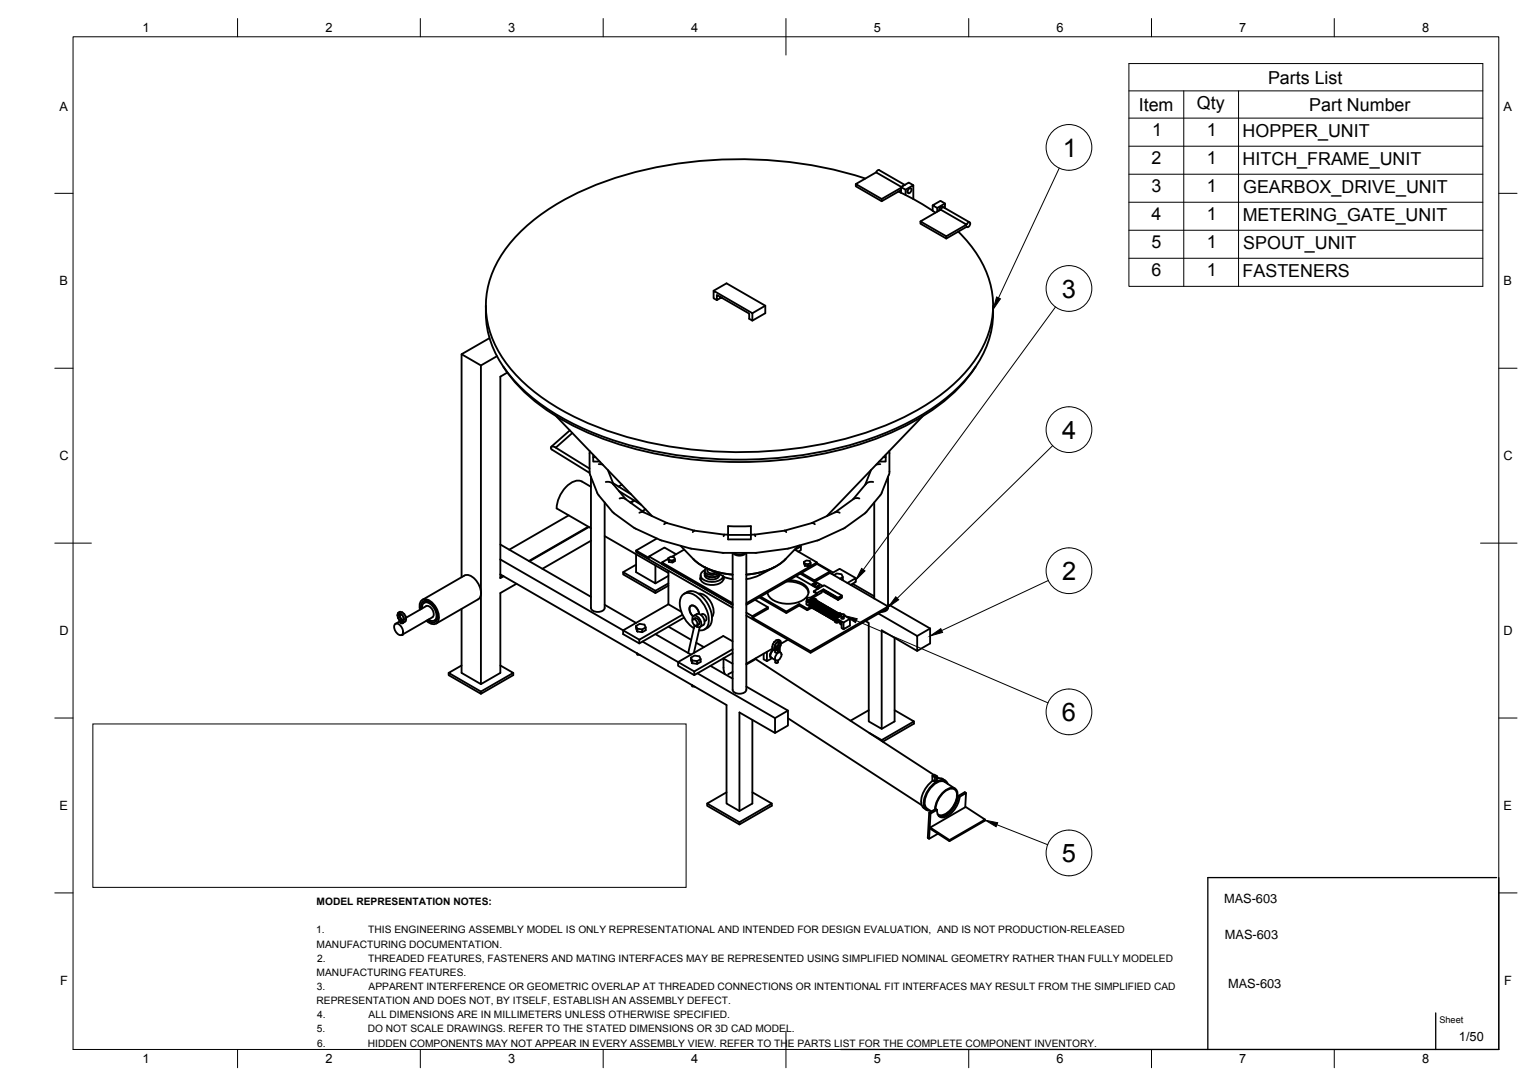
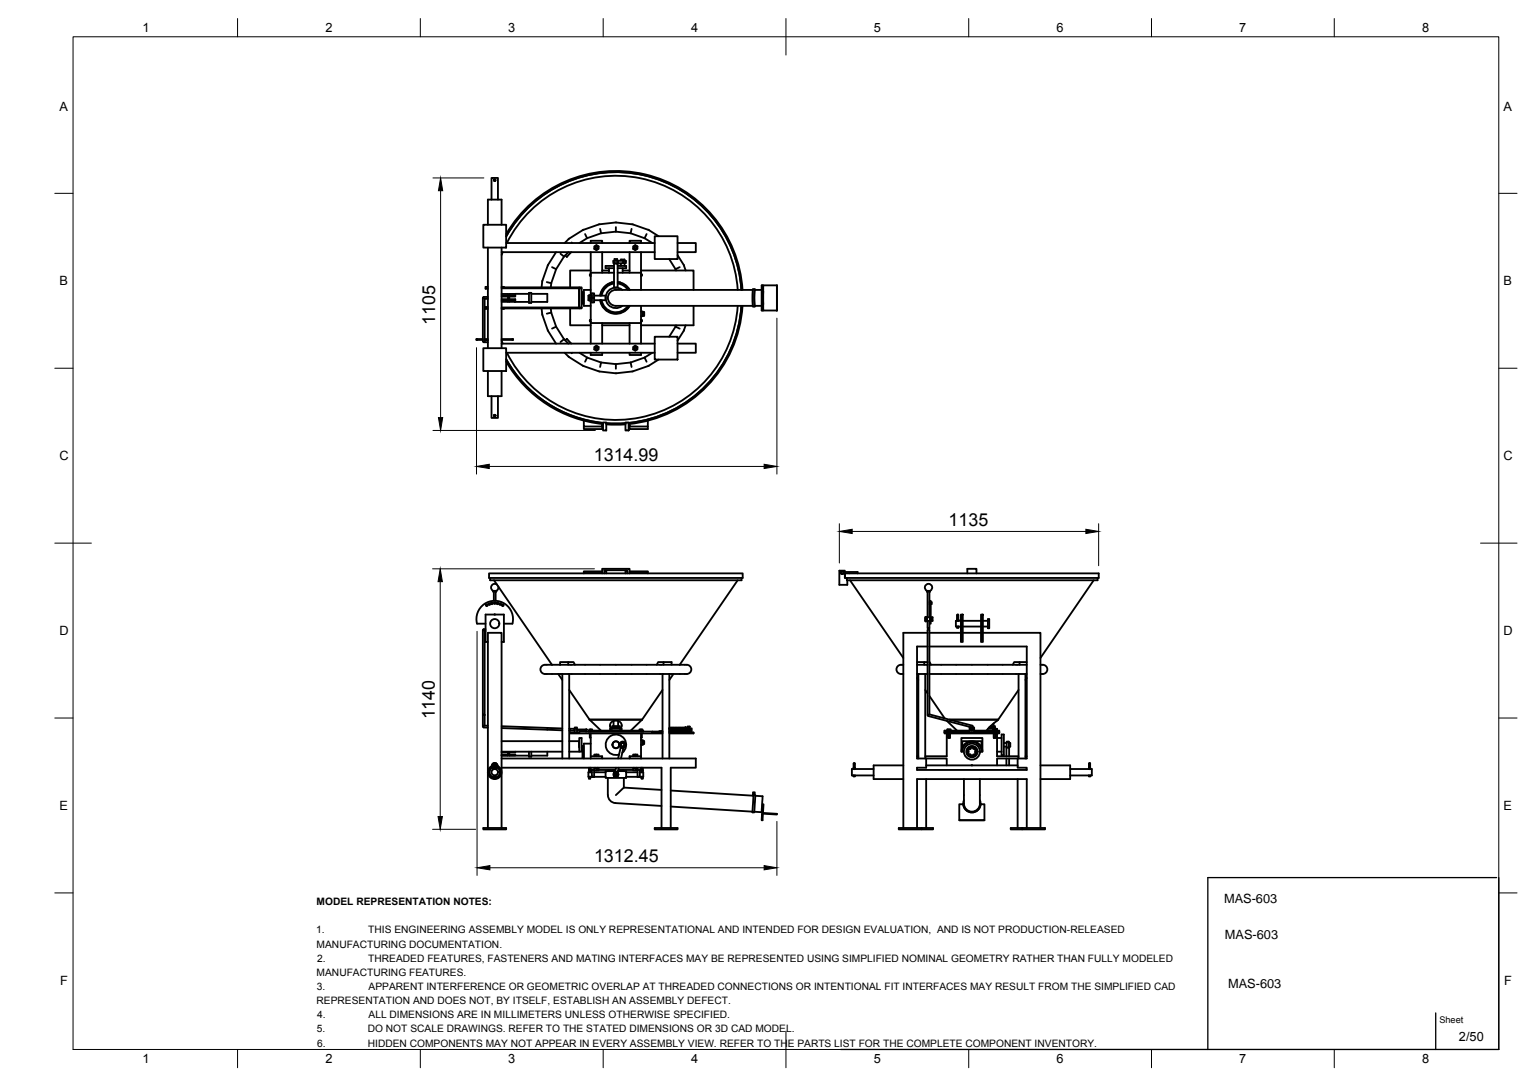
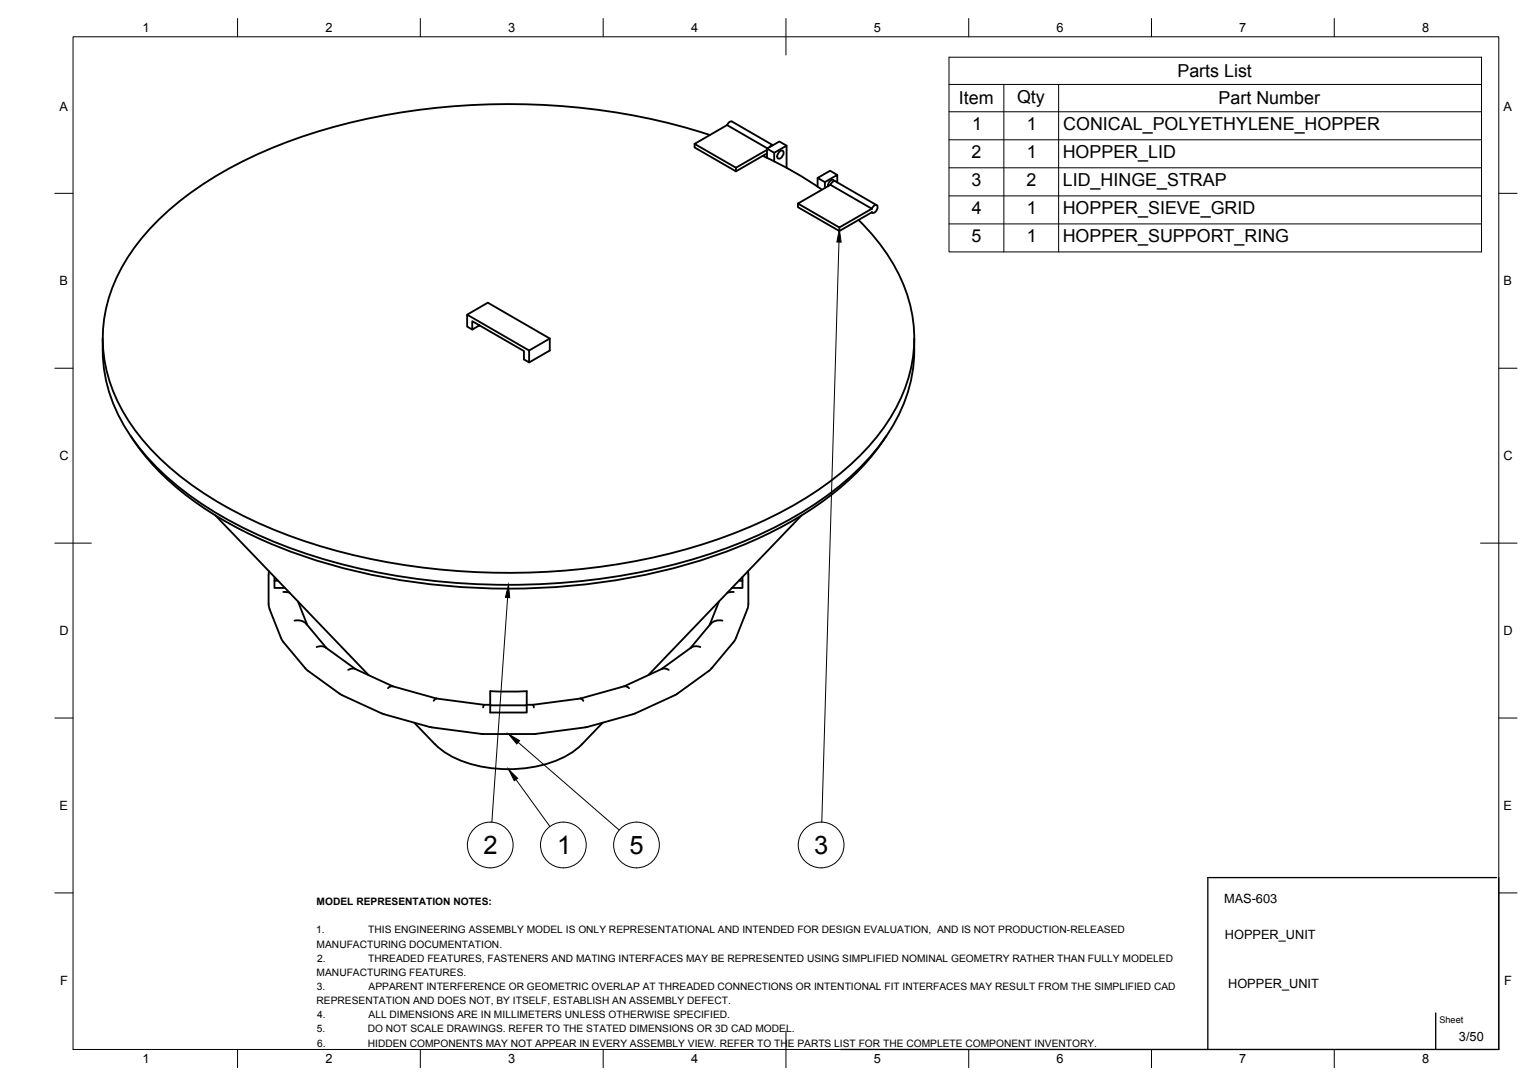
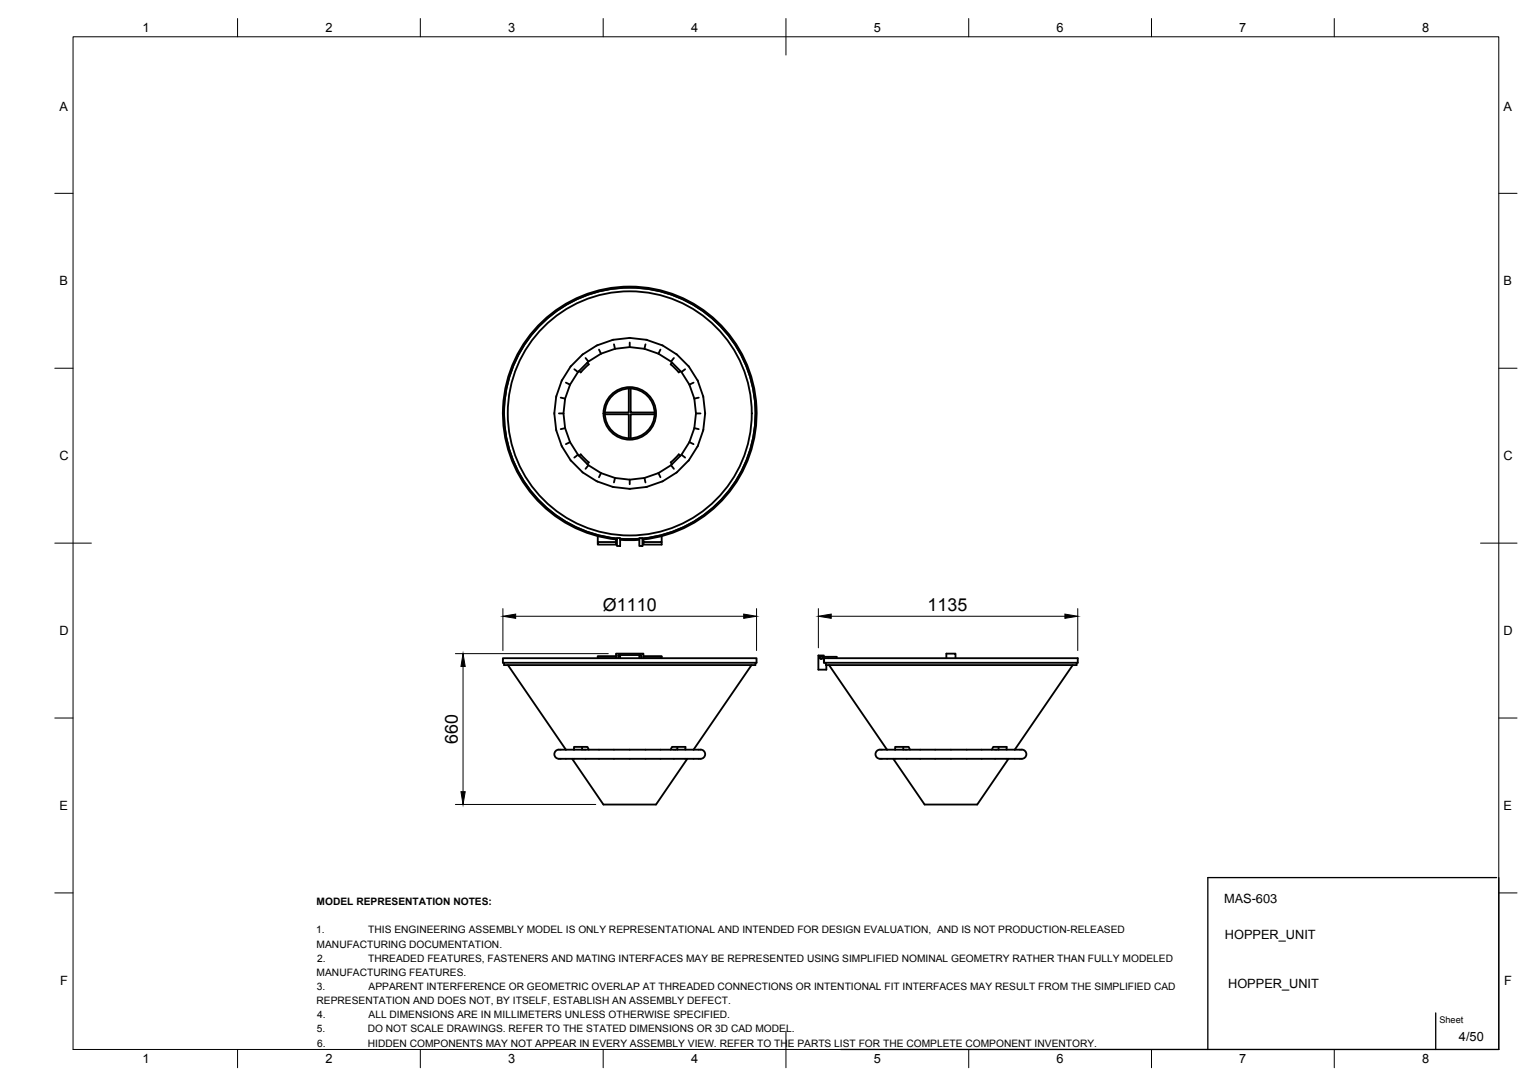
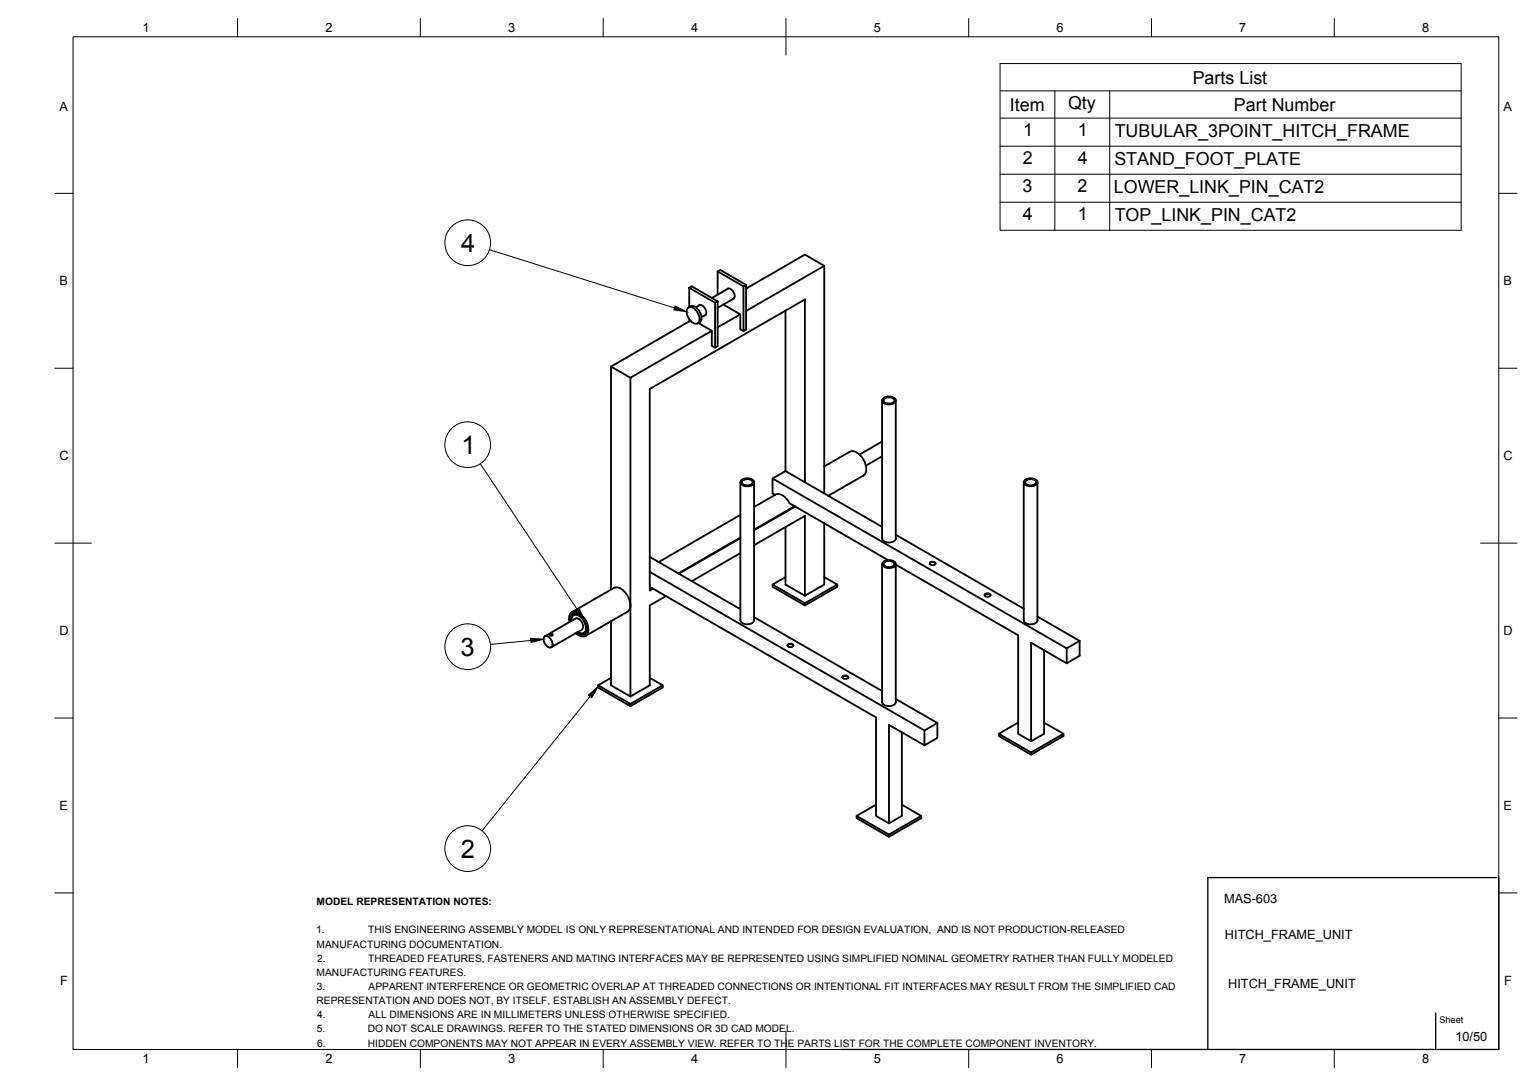
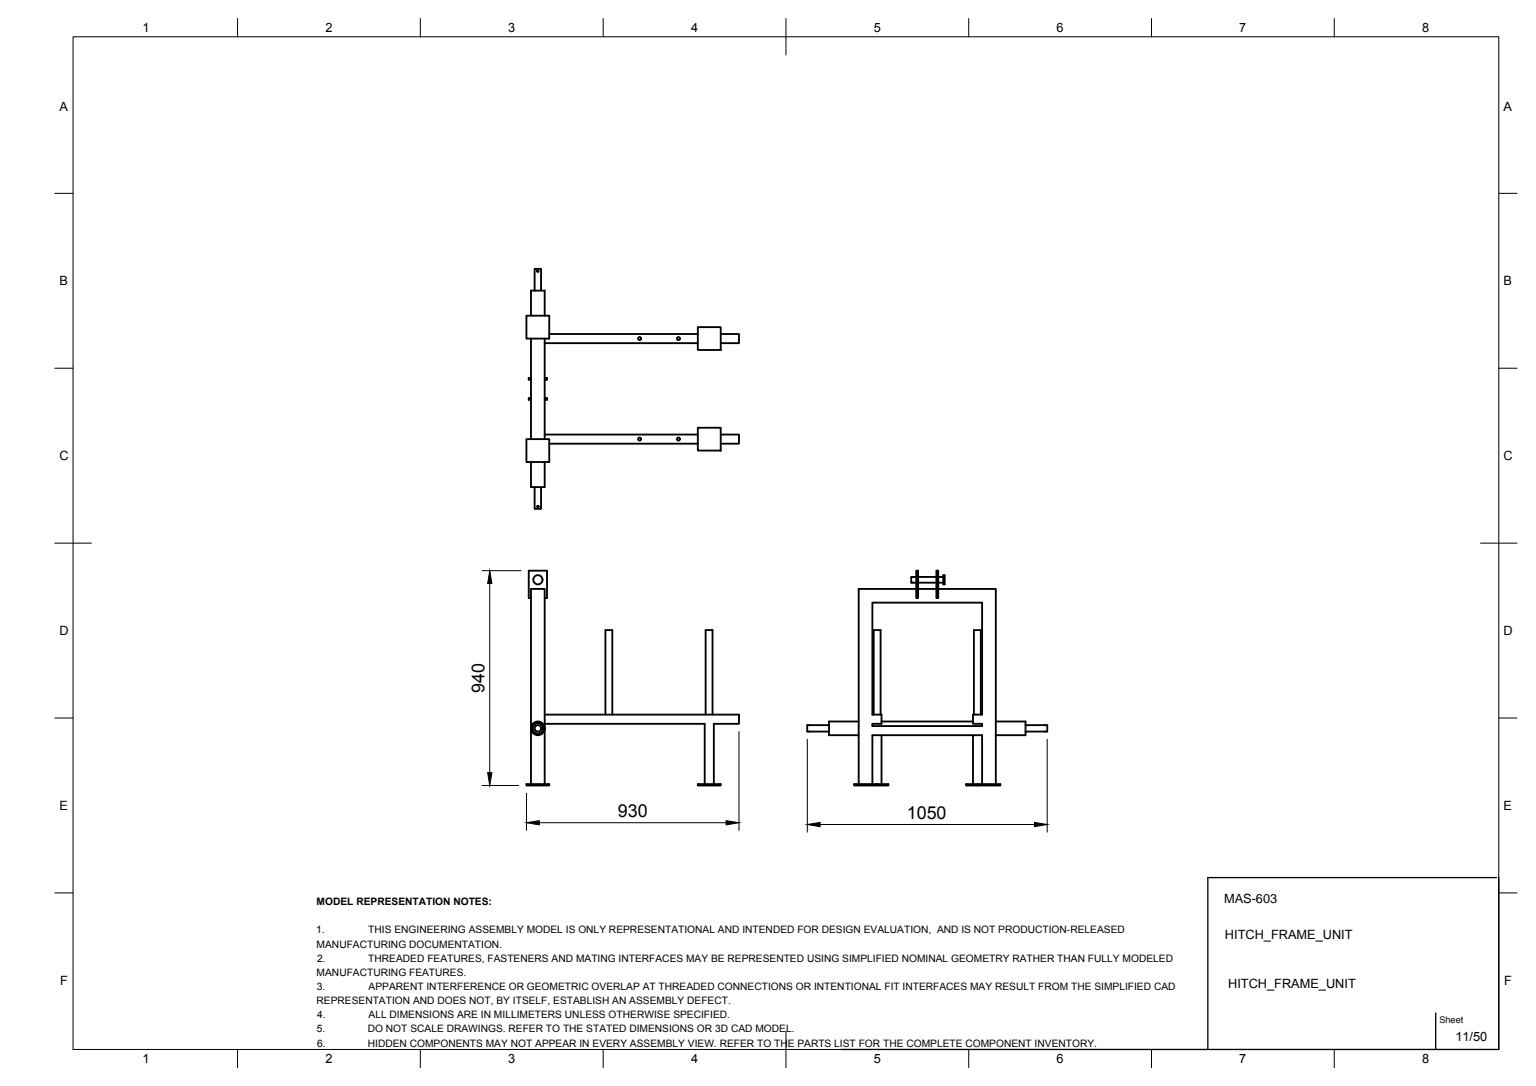
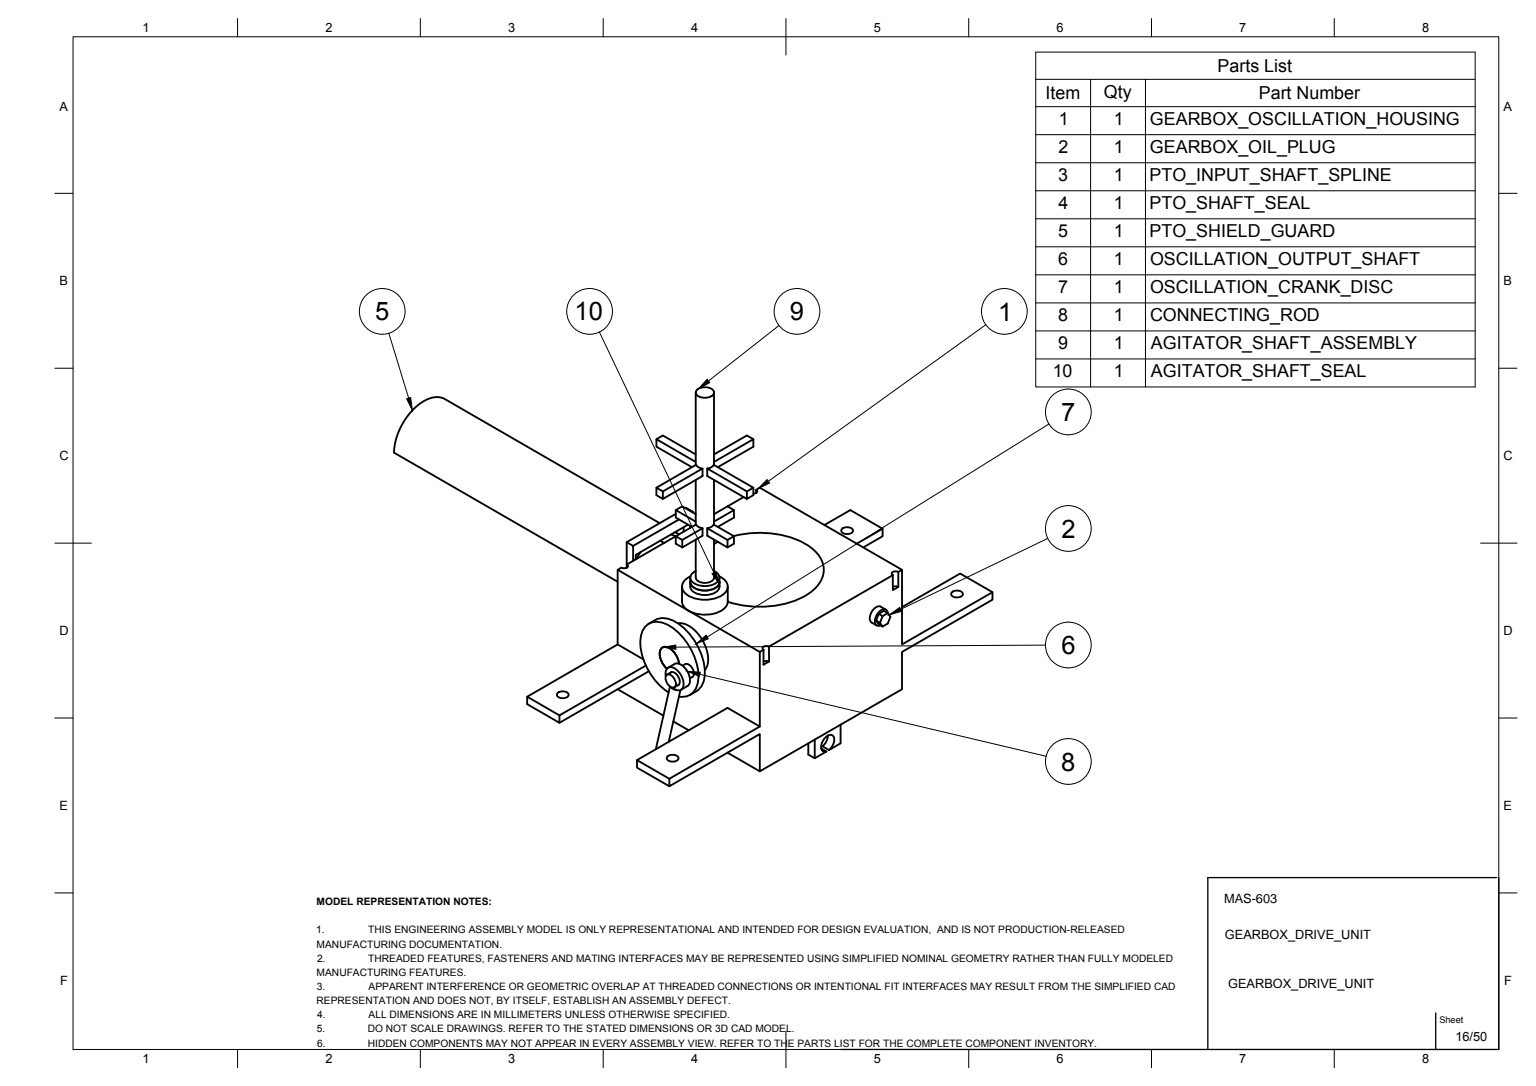
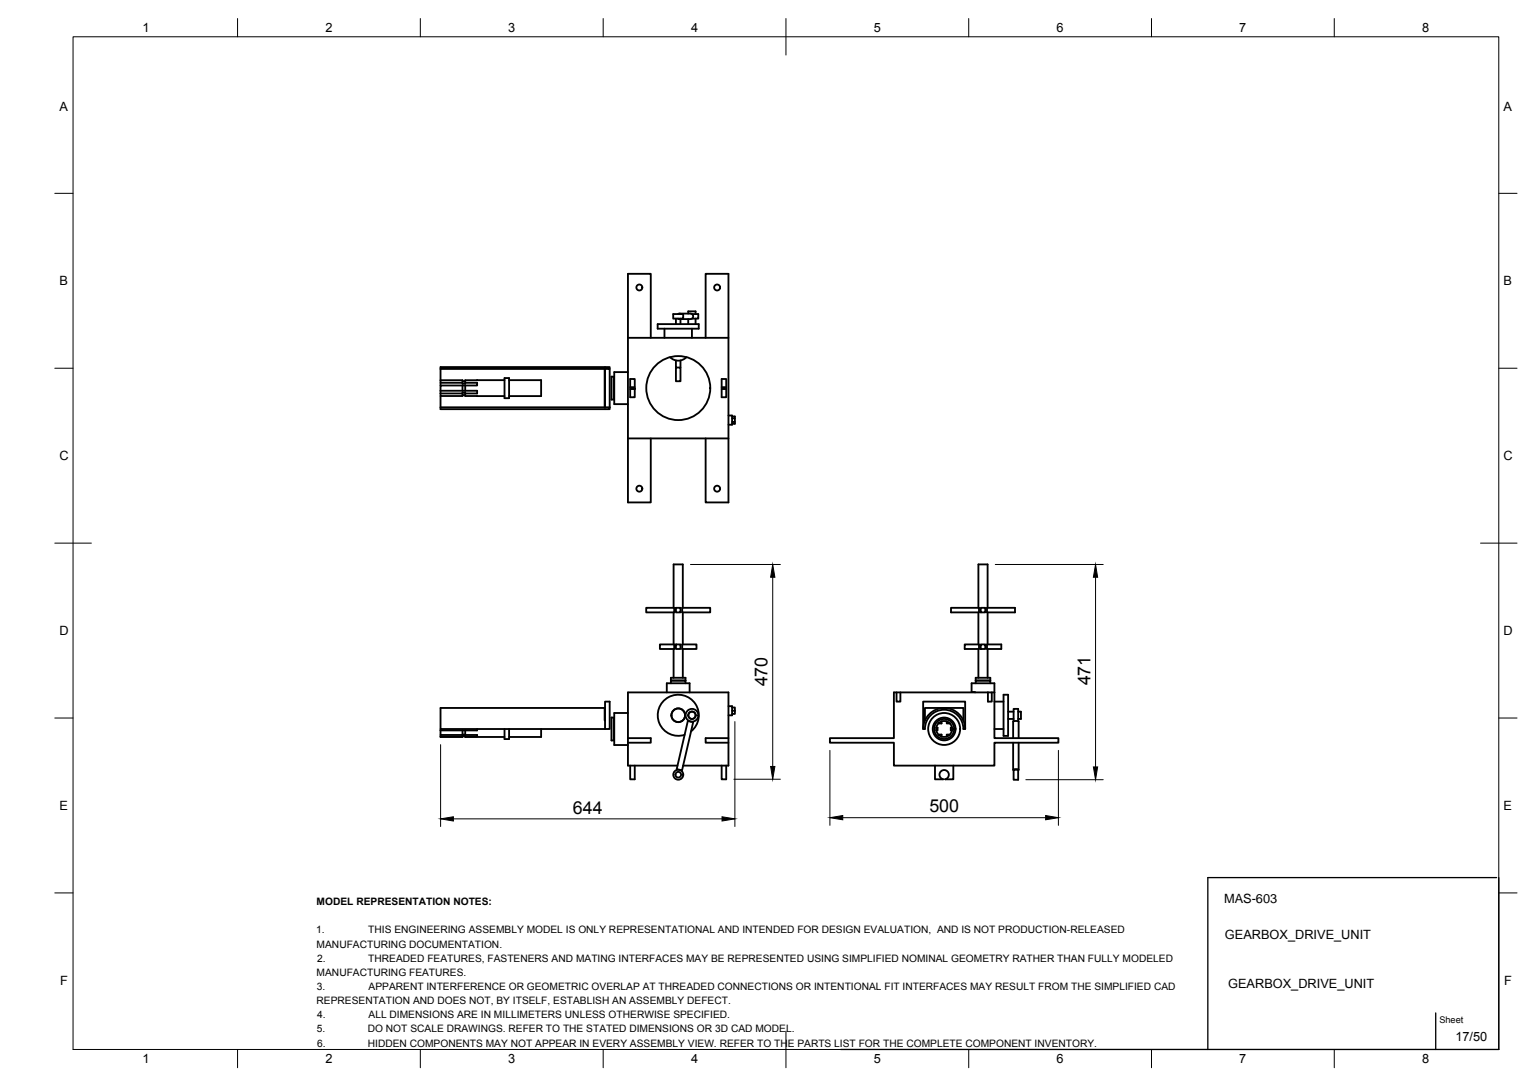
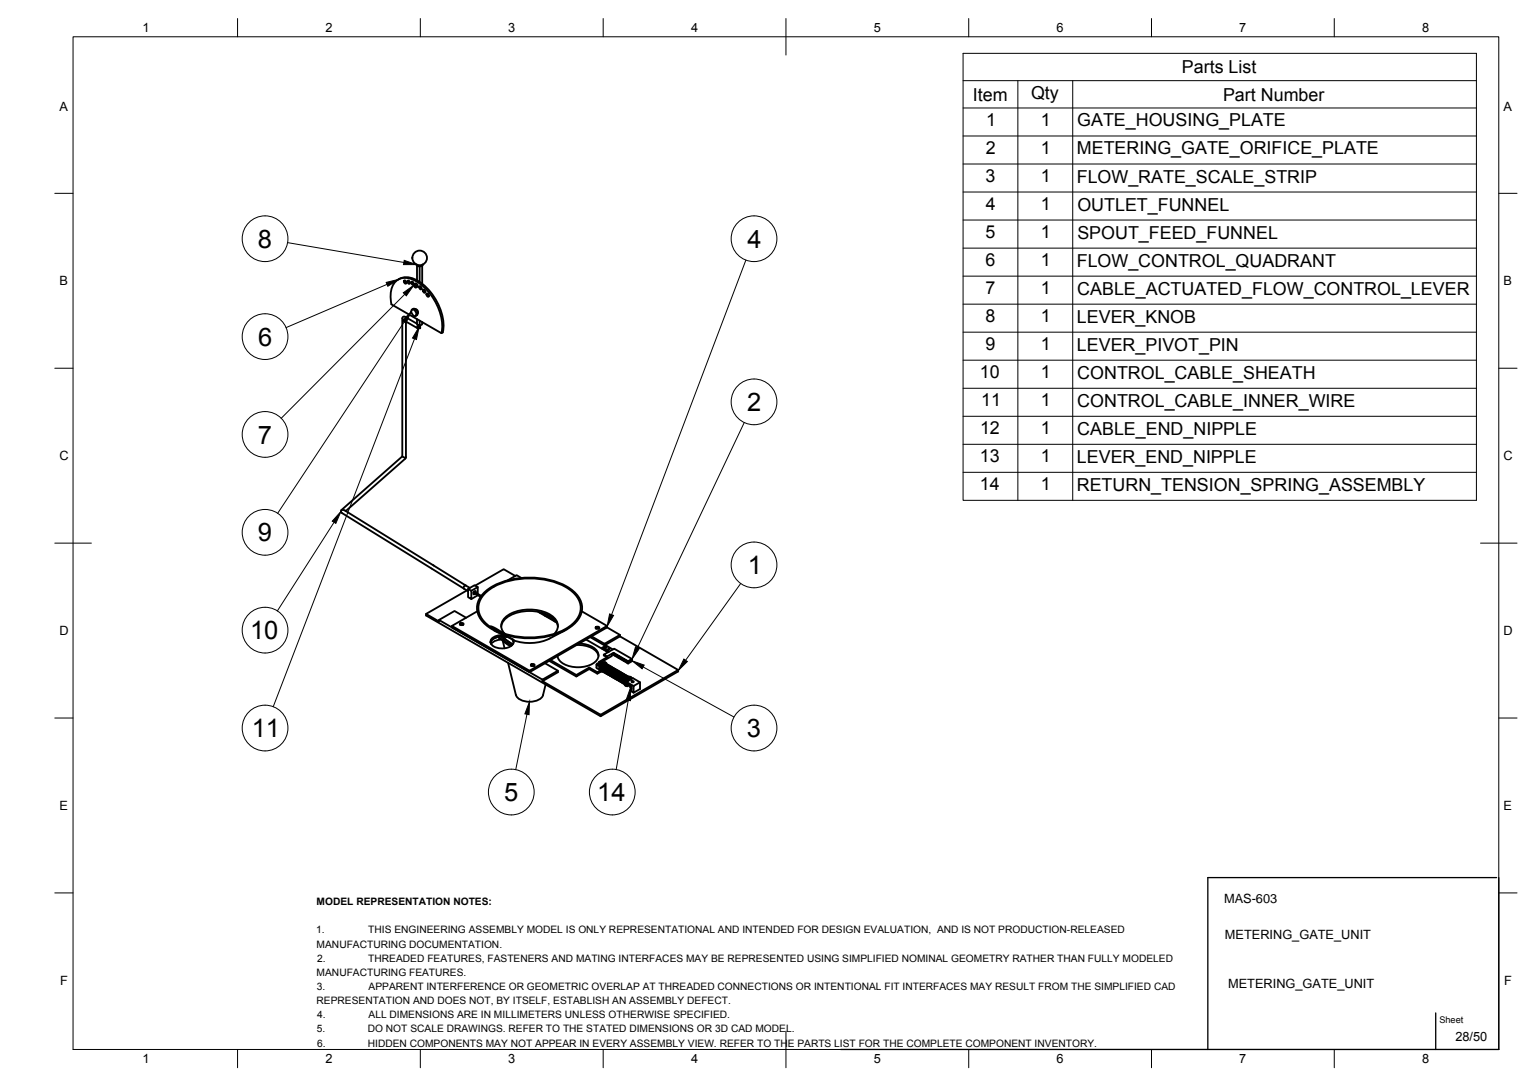
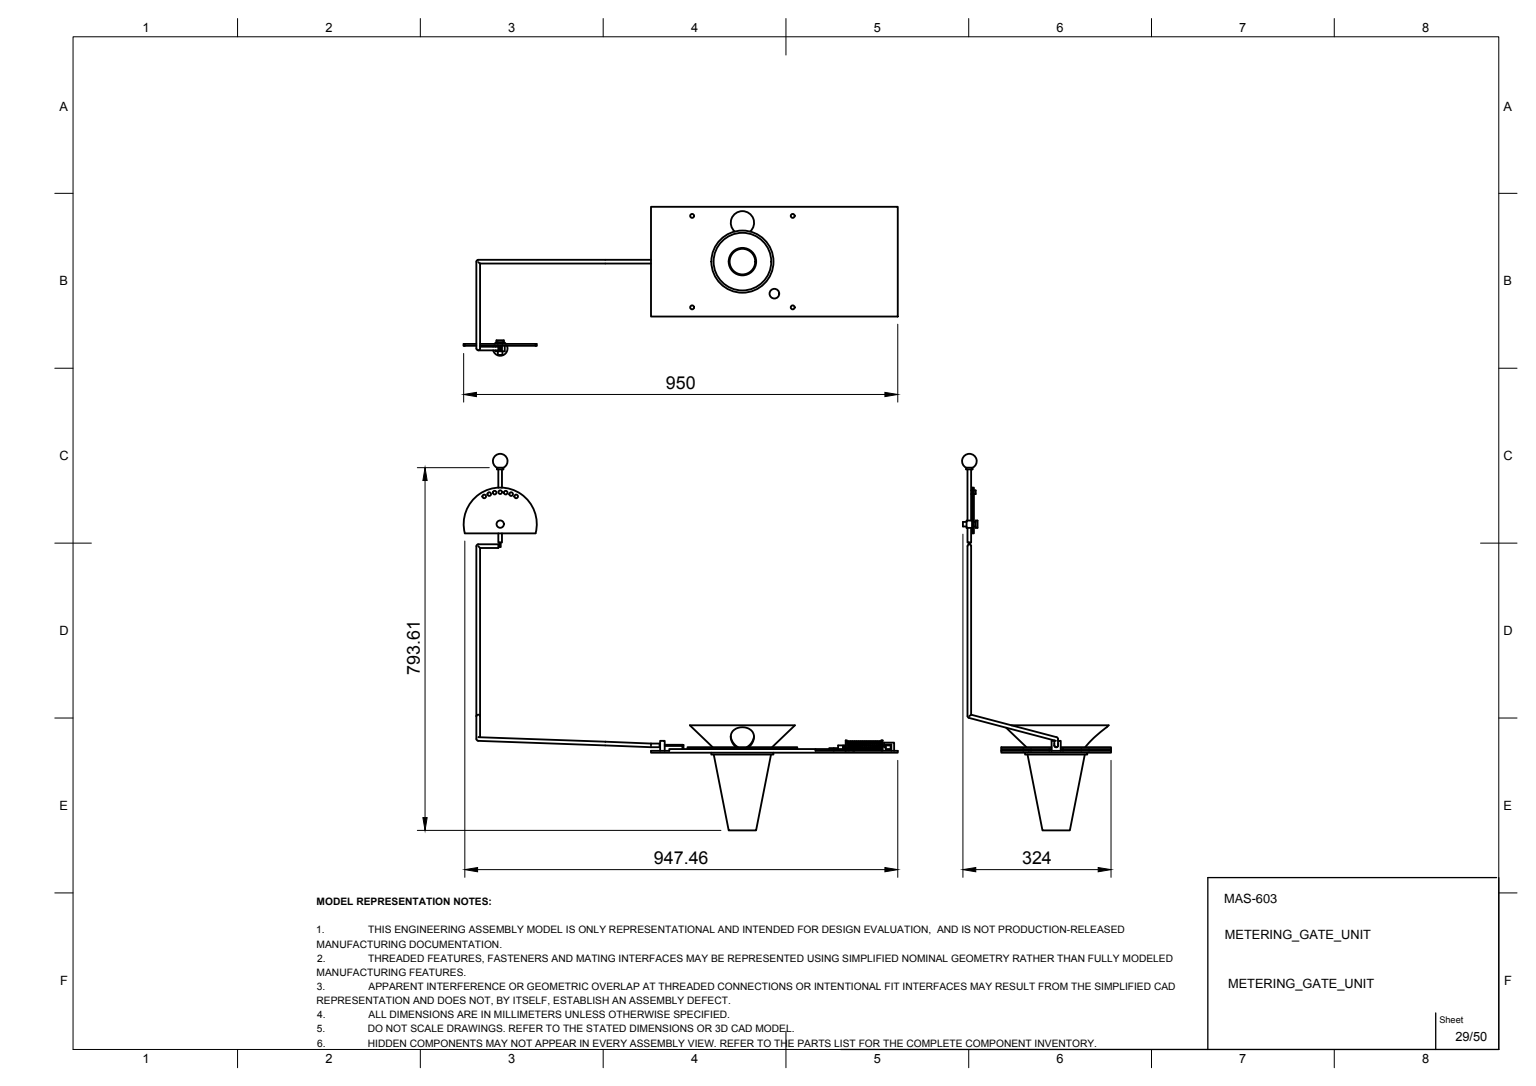
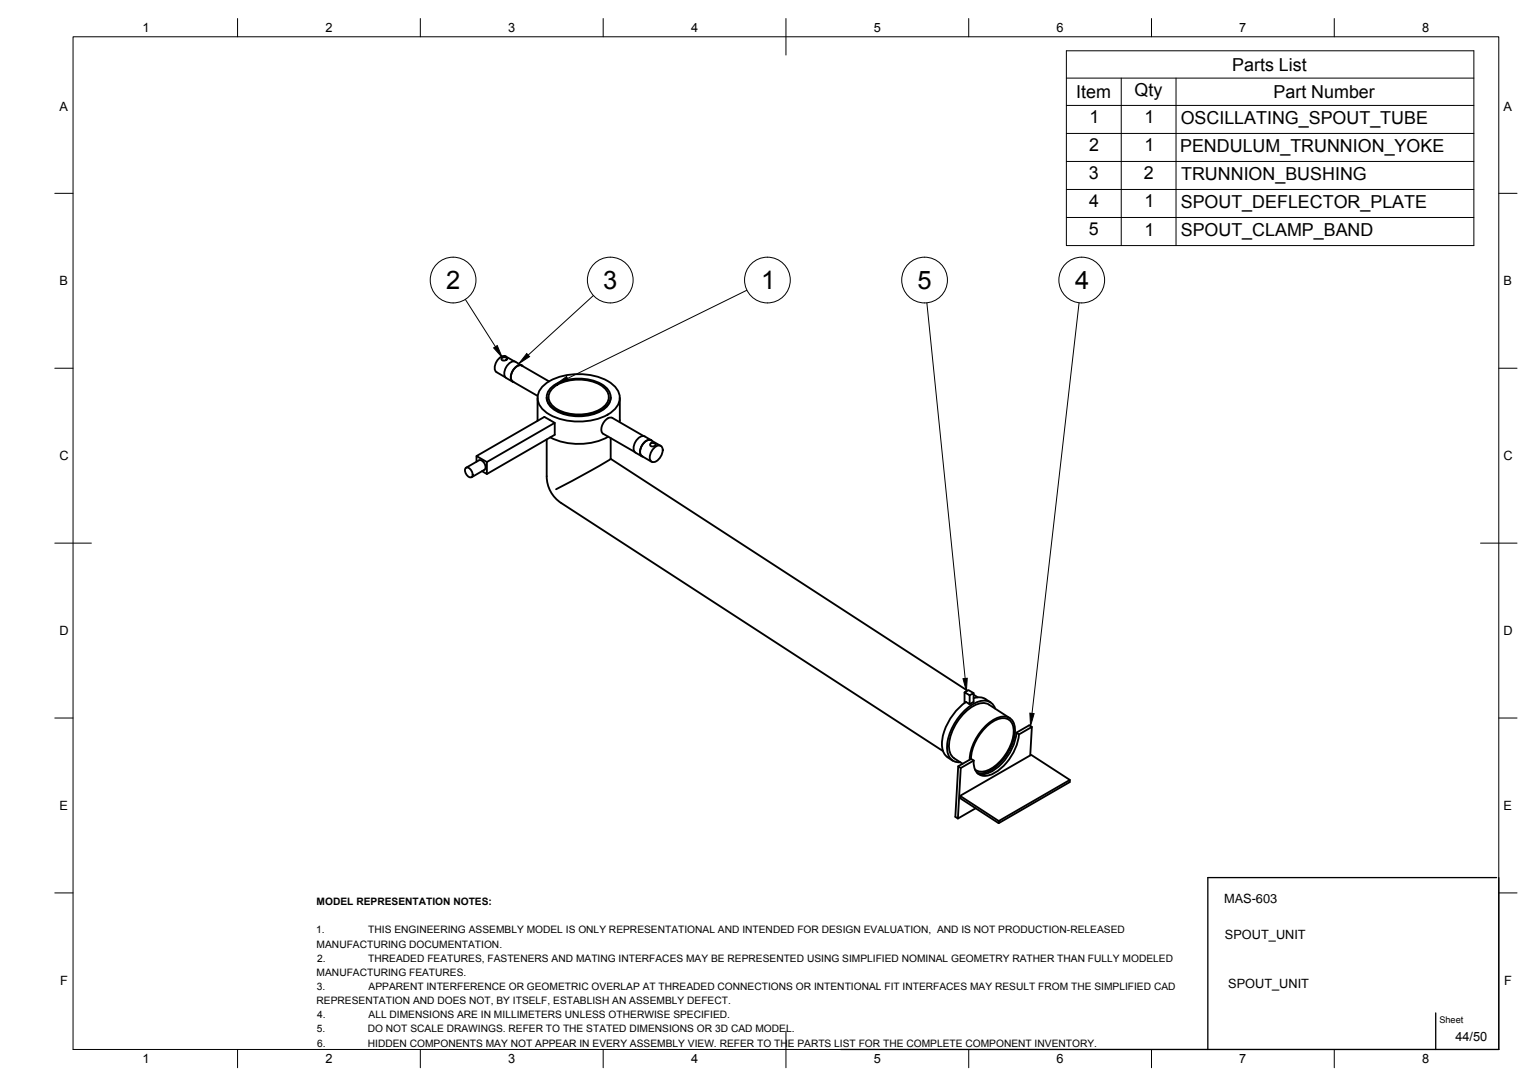
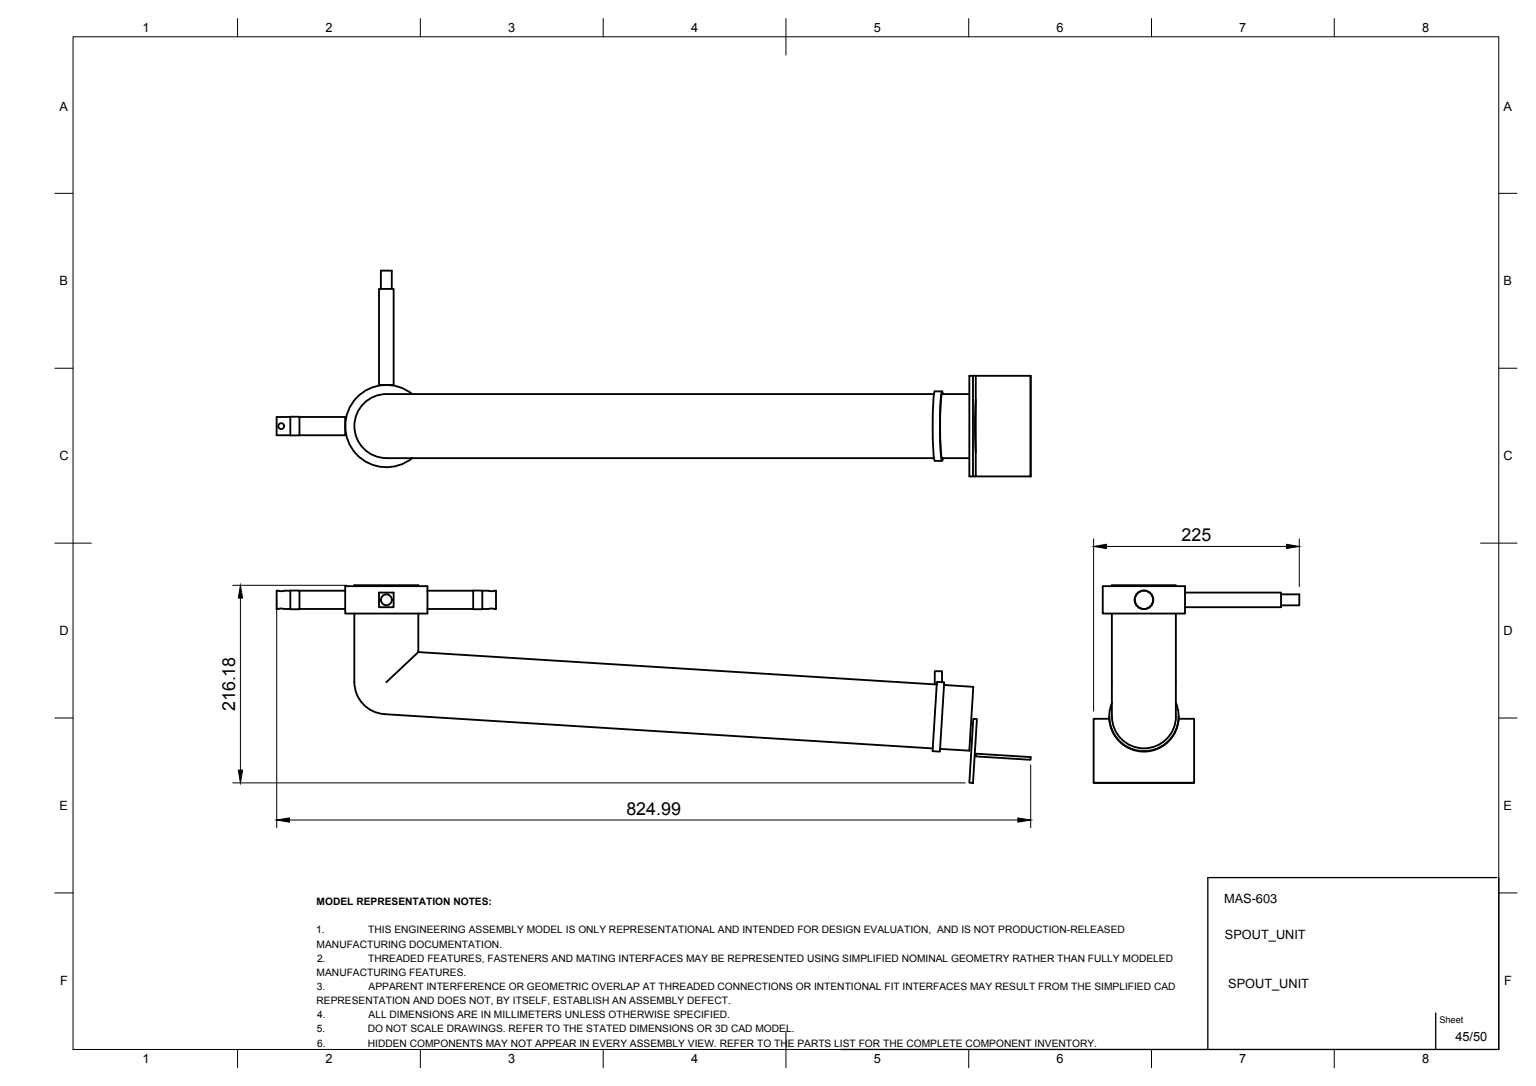
ISO-10303-21;
HEADER;
FILE_DESCRIPTION((''),'2;1');
FILE_NAME('MAS-603','2026-10-01T22:06:14-07:00',(''),(''),'','','');
FILE_SCHEMA (('AUTOMOTIVE_DESIGN { 1 0 10303 214 3 1 1 }'));
ENDSEC;
DATA;
#10 = MECHANICAL_DESIGN_GEOMETRIC_PRESENTATION_REPRESENTATION('',(#981,#982,
#983,#984,#985,#986,#987,#988,#989,#990,#991,#992,#993,#994,#995,#996,#997,
#998,#999,#1000,#1001,#1002,#1003,#1004,#1005,#1006,#1007,#1008,#1009,#1010,
#1011,#1012,#1013,#1014,#1015,#1016,#1017,#1018,#1019,#1020,#1021,#1022,
#1023,#1024,#1025,#1026,#1027,#1028,#1029,#1030,#1031,#1032,#1033,#1034,
#1035,#1036),#50440) ;
#11 = B_SPLINE_CURVE_WITH_KNOTS('',3,(#44873,#44874,#44875,#44876,#44877,
#44878,#44879,#44880,#44881,#44882,#44883,#44884,#44885,#44886,#44887,#44888,
#44889,#44890),.UNSPECIFIED.,.F.,.F.,(4,2,2,2,2,2,2,2,4),(0.,0.13245688121231,
0.264913762424621,0.39735212380502,0.529790485185418,0.662228846565817,
0.794667207946216,0.927124089158526,1.05958097037084),.UNSPECIFIED.) ;
#12 = B_SPLINE_CURVE_WITH_KNOTS('',3,(#44891,#44892,#44893,#44894,#44895,
#44896,#44897,#44898,#44899,#44900,#44901,#44902,#44903,#44904,#44905,#44906,
#44907,#44908),.UNSPECIFIED.,.F.,.F.,(4,2,2,2,2,2,2,2,4),(1.05958097037084,
1.19203785158315,1.32449473279546,1.45693309417586,1.58937145555626,1.72180981693665,
1.85424817831705,1.98670505952936,2.11916194074167),.UNSPECIFIED.) ;
#13 = B_SPLINE_CURVE_WITH_KNOTS('',3,(#44912,#44913,#44914,#44915,#44916,
#44917,#44918,#44919,#44920,#44921,#44922,#44923,#44924,#44925,#44926,#44927,
#44928,#44929),.UNSPECIFIED.,.F.,.F.,(4,2,2,2,2,2,2,2,4),(0.,0.13245688121231,
0.264913762424621,0.39735212380502,0.529790485185418,0.662228846565817,
0.794667207946216,0.927124089158526,1.05958097037084),.UNSPECIFIED.) ;
#14 = B_SPLINE_CURVE_WITH_KNOTS('',3,(#44930,#44931,#44932,#44933,#44934,
#44935,#44936,#44937,#44938,#44939,#44940,#44941,#44942,#44943,#44944,#44945,
#44946,#44947),.UNSPECIFIED.,.F.,.F.,(4,2,2,2,2,2,2,2,4),(1.05958097037084,
1.19203785158315,1.32449473279546,1.45693309417586,1.58937145555626,1.72180981693665,
1.85424817831705,1.98670505952936,2.11916194074167),.UNSPECIFIED.) ;
#15 = B_SPLINE_CURVE_WITH_KNOTS('',3,(#44967,#44968,#44969,#44970,#44971,
#44972,#44973,#44974,#44975,#44976,#44977,#44978,#44979,#44980,#44981,#44982,
#44983,#44984),.UNSPECIFIED.,.F.,.F.,(4,2,2,2,2,2,2,2,4),(0.,0.132623145855944,
0.265246291711889,0.39783980012189,0.530433308531892,0.663026816941894,
0.795620325351895,0.92824347120784,1.06086661706378),.UNSPECIFIED.) ;
#16 = B_SPLINE_CURVE_WITH_KNOTS('',3,(#44985,#44986,#44987,#44988,#44989,
#44990,#44991,#44992,#44993,#44994,#44995,#44996,#44997,#44998,#44999,#45000,
#45001,#45002),.UNSPECIFIED.,.F.,.F.,(4,2,2,2,2,2,2,2,4),(1.06086661706378,
1.19348976291973,1.32611290877567,1.45870641718567,1.59129992559568,1.72389343400568,
1.85648694241568,1.98911008827162,2.12173323412757),.UNSPECIFIED.) ;
#17 = B_SPLINE_CURVE_WITH_KNOTS('',3,(#45006,#45007,#45008,#45009,#45010,
#45011,#45012,#45013,#45014,#45015,#45016,#45017,#45018,#45019,#45020,#45021,
#45022,#45023),.UNSPECIFIED.,.F.,.F.,(4,2,2,2,2,2,2,2,4),(0.,0.132623145855943,
0.265246291711887,0.397839800121889,0.530433308531891,0.663026816941892,
0.795620325351894,0.928243471207838,1.06086661706378),.UNSPECIFIED.) ;
#18 = B_SPLINE_CURVE_WITH_KNOTS('',3,(#45024,#45025,#45026,#45027,#45028,
#45029,#45030,#45031,#45032,#45033,#45034,#45035,#45036,#45037,#45038,#45039,
#45040,#45041),.UNSPECIFIED.,.F.,.F.,(4,2,2,2,2,2,2,2,4),(1.06086661706378,
1.19348976291973,1.32611290877567,1.45870641718567,1.59129992559567,1.72389343400568,
1.85648694241568,1.98911008827162,2.12173323412757),.UNSPECIFIED.) ;
#19 = B_SPLINE_CURVE_WITH_KNOTS('',3,(#46833,#46834,#46835,#46836,#46837,
#46838,#46839,#46840,#46841,#46842,#46843,#46844,#46845,#46846,#46847,#46848,
#46849,#46850,#46851,#46852,#46853,#46854,#46855,#46856,#46857,#46858,#46859,
#46860,#46861,#46862,#46863,#46864,#46865,#46866,#46867,#46868,#46869,#46870,
#46871,#46872,#46873,#46874,#46875,#46876,#46877,#46878,#46879),
 .UNSPECIFIED.,.F.,.F.,(4,2,2,2,2,2,2,2,2,2,2,2,2,2,2,2,2,2,2,3,2,2,4),
(-13.6435660379385,-13.1032156835778,-11.9806697877857,-10.8581238919937,
-10.1062638186437,-9.35440374529371,-8.60254367194372,-7.85068359859374,
-7.19512813941189,-6.53957268023004,-5.98431731311344,-5.42906194599684,
-4.87380657888023,-4.31855121176363,-3.66299575258178,-3.00744029339993,
-2.25558022004995,-1.50372014669997,-0.751860073349981,0.,1.12254589579207,
2.24509179158414,2.78544215194592),.UNSPECIFIED.) ;
#20 = B_SPLINE_CURVE_WITH_KNOTS('',3,(#46883,#46884,#46885,#46886,#46887,
#46888,#46889,#46890,#46891,#46892,#46893,#46894,#46895,#46896,#46897,#46898,
#46899,#46900,#46901,#46902,#46903,#46904,#46905,#46906,#46907,#46908,#46909,
#46910,#46911,#46912,#46913,#46914,#46915,#46916,#46917,#46918,#46919,#46920,
#46921,#46922,#46923,#46924,#46925),.UNSPECIFIED.,.F.,.F.,(4,2,3,2,2,2,
2,2,2,2,2,2,2,2,2,2,2,2,2,2,4),(-2.23663632321178,-1.12254589579207,0.,
0.751860073349982,1.50372014669996,2.25558022004995,3.00744029339993,3.66299575258178,
4.31855121176363,4.87380657888023,5.42906194599683,5.98431731311343,6.53957268023004,
7.19512813941189,7.85068359859374,8.60254367194372,9.3544037452937,10.1062638186437,
10.8581238919937,11.9806697877857,13.0947602152054),.UNSPECIFIED.) ;
#21 = B_SPLINE_CURVE_WITH_KNOTS('',3,(#47253,#47254,#47255,#47256,#47257,
#47258,#47259,#47260,#47261,#47262),.UNSPECIFIED.,.F.,.F.,(4,2,2,2,4),(0.22845269137107,
0.285543988105223,0.342635284839377,0.399770333790758,0.45690538274214),
 .UNSPECIFIED.) ;
#22 = B_SPLINE_CURVE_WITH_KNOTS('',3,(#47263,#47264,#47265,#47266,#47267,
#47268,#47269,#47270,#47271,#47272),.UNSPECIFIED.,.F.,.F.,(4,2,2,2,4),(0.,
0.0571350489513819,0.114270097902764,0.171361394636917,0.22845269137107),
 .UNSPECIFIED.) ;
#23 = B_SPLINE_CURVE_WITH_KNOTS('',3,(#47334,#47335,#47336,#47337,#47338,
#47339,#47340,#47341,#47342,#47343,#47344,#47345,#47346,#47347,#47348,#47349,
#47350,#47351),.UNSPECIFIED.,.F.,.F.,(4,2,2,2,2,2,2,2,4),(-0.453190854157869,
-0.399487512163789,-0.342402977588613,-0.285344500479048,-0.228286023369483,
-0.171227546259919,-0.114169069150354,-0.0570845345751771,-0.00338119258109968),
 .UNSPECIFIED.) ;
#24 = B_SPLINE_CURVE_WITH_KNOTS('',3,(#47365,#47366,#47367,#47368,#47369,
#47370,#47371,#47372,#47373,#47374,#47375,#47376,#47377,#47378),
 .UNSPECIFIED.,.F.,.F.,(4,2,2,2,2,2,4),(0.577610065542725,0.589037524605606,
0.645581544002731,0.702125563399856,0.758669582796981,0.815213602194107,
0.826641061257004),.UNSPECIFIED.) ;
#25 = B_SPLINE_CURVE_WITH_KNOTS('',3,(#47382,#47383,#47384,#47385,#47386,
#47387,#47388,#47389,#47390,#47391,#47392,#47393,#47394,#47395,#47396,#47397,
#47398,#47399),.UNSPECIFIED.,.F.,.F.,(4,2,2,2,2,2,2,2,4),(0.00338117995301888,
0.0570585291380164,0.114117058276033,0.171201519148796,0.228285980021559,
0.285370440894324,0.342454901767089,0.399513430905107,0.453190780090104),
 .UNSPECIFIED.) ;
#26 = B_SPLINE_CURVE_WITH_KNOTS('',3,(#47419,#47420,#47421,#47422,#47423,
#47424,#47425,#47426,#47427,#47428,#47429,#47430,#47431,#47432,#47433,#47434,
#47435,#47436),.UNSPECIFIED.,.F.,.F.,(4,2,2,2,2,2,2,2,4),(-0.456905382742139,
-0.399770333790757,-0.342635284839376,-0.285543988105223,-0.228452691371069,
-0.171361394636916,-0.114270097902762,-0.0571350489513811,0.),
 .UNSPECIFIED.) ;
#27 = B_SPLINE_CURVE_WITH_KNOTS('',3,(#47442,#47443,#47444,#47445,#47446,
#47447,#47448,#47449,#47450,#47451,#47452,#47453,#47454,#47455),
 .UNSPECIFIED.,.F.,.F.,(4,2,2,2,2,2,4),(0.102836390905491,0.113768884994942,
0.170566995159794,0.227365105324647,0.2841632154895,0.340961325654353,0.351893819743812),
 .UNSPECIFIED.) ;
#28 = B_SPLINE_CURVE_WITH_KNOTS('',3,(#47529,#47530,#47531,#47532,#47533,
#47534,#47535,#47536,#47537,#47538),.UNSPECIFIED.,.F.,.F.,(4,2,2,2,4),(0.,
0.0609860967122279,0.121972193424456,0.180509993590844,0.239047793757233),
 .UNSPECIFIED.) ;
#29 = B_SPLINE_CURVE_WITH_KNOTS('',3,(#47539,#47540,#47541,#47542,#47543,
#47544,#47545,#47546,#47547,#47548,#47549,#47550,#47551,#47552,#47553,#47554,
#47555,#47556,#47557,#47558,#47559,#47560,#47561,#47562,#47563,#47564),
 .UNSPECIFIED.,.F.,.F.,(4,2,2,2,2,2,2,2,2,2,2,2,4),(0.239047793757233,0.297585593923622,
0.35612339409001,0.417109490802238,0.478095587514466,0.536342851072485,
0.594590114630504,0.651016946753083,0.707443778875663,0.763870610998243,
0.820297443120823,0.878544706678841,0.93679197023686),.UNSPECIFIED.) ;
#30 = B_SPLINE_CURVE_WITH_KNOTS('',3,(#47597,#47598,#47599,#47600,#47601,
#47602,#47603,#47604,#47605,#47606),.UNSPECIFIED.,.F.,.F.,(4,2,2,2,4),(1.59601342827562,
1.72868455666642,1.90688135822923,2.08609099459942,2.19153831493185),
 .UNSPECIFIED.) ;
#31 = B_SPLINE_CURVE_WITH_KNOTS('',3,(#47608,#47609,#47610,#47611,#47612,
#47613,#47614,#47615,#47616,#47617),.UNSPECIFIED.,.F.,.F.,(4,2,2,2,4),(1.59601342827561,
1.72868455666641,1.90688135822922,2.0860909945994,2.19148469566779),
 .UNSPECIFIED.) ;
#32 = B_SPLINE_CURVE_WITH_KNOTS('',3,(#47619,#47620,#47621,#47622,#47623,
#47624),.UNSPECIFIED.,.F.,.F.,(4,2,4),(1.93627902173741,2.08609099459941,
2.19148469566782),.UNSPECIFIED.) ;
#33 = B_SPLINE_CURVE_WITH_KNOTS('',3,(#49299,#49300,#49301,#49302,#49303,
#49304,#49305,#49306,#49307,#49308,#49309,#49310,#49311,#49312,#49313,#49314,
#49315,#49316),.UNSPECIFIED.,.F.,.F.,(4,2,2,2,2,2,2,2,4),(0.228893413219578,
0.285350813018225,0.341808212816873,0.399797519628014,0.457786826439155,
0.518403668051846,0.579020509664538,0.637418929805441,0.695817349946344),
 .UNSPECIFIED.) ;
#34 = B_SPLINE_CURVE_WITH_KNOTS('',3,(#49321,#49322,#49323,#49324,#49325,
#49326,#49327,#49328,#49329,#49330),.UNSPECIFIED.,.F.,.F.,(4,2,2,2,4),(0.,
0.0579893068111412,0.115978613622282,0.17243601342093,0.228893413219578),
 .UNSPECIFIED.) ;
#35 = B_SPLINE_CURVE_WITH_KNOTS('',3,(#49331,#49332,#49333,#49334,#49335,
#49336,#49337,#49338,#49339,#49340),.UNSPECIFIED.,.F.,.F.,(4,2,2,2,4),(0.695817349946344,
0.754215770087248,0.812614190228152,0.873231031840842,0.933847873453534),
 .UNSPECIFIED.) ;
#36 = B_SPLINE_CURVE_WITH_KNOTS('',3,(#49390,#49391,#49392,#49393,#49394,
#49395,#49396,#49397,#49398,#49399,#49400,#49401,#49402,#49403,#49404,#49405,
#49406,#49407,#49408,#49409,#49410,#49411,#49412,#49413,#49414,#49415,#49416,
#49417,#49418,#49419,#49420,#49421,#49422,#49423,#49424,#49425,#49426,#49427),
 .UNSPECIFIED.,.F.,.F.,(4,2,2,2,2,2,2,2,2,2,2,2,2,2,2,2,2,2,4),(11.701609895415,
11.9954810277209,12.363235333761,13.0987439458412,13.8342525579214,14.5697611700016,
15.2442090288987,15.9186568877959,16.593104746693,17.2675526055902,17.9420004644874,
18.6164483233845,19.2908961822817,19.9653440411788,20.700852653259,21.4363612653392,
22.1718698774194,22.5396241834595,22.8334953157654),.UNSPECIFIED.) ;
#37 = B_SPLINE_CURVE_WITH_KNOTS('',3,(#49445,#49446,#49447,#49448,#49449,
#49450,#49451,#49452,#49453,#49454,#49455,#49456,#49457,#49458,#49459,#49460,
#49461,#49462,#49463,#49464,#49465,#49466,#49467,#49468,#49469,#49470,#49471,
#49472,#49473,#49474,#49475,#49476,#49477,#49478,#49479,#49480,#49481,#49482),
 .UNSPECIFIED.,.F.,.F.,(4,2,2,2,2,2,2,2,2,2,2,2,2,2,2,2,2,2,4),(0.0738831737341421,
0.367754306040092,0.735508612080185,1.47101722416037,2.20652583624055,2.94203444832074,
3.61648230721789,4.29093016611505,4.9653780250122,5.63982588390936,6.31427374280651,
6.98872160170367,7.66316946060082,8.33761731949797,9.07312593157816,9.80863454365834,
10.5441431557385,10.9118974617786,11.2057685940846),.UNSPECIFIED.) ;
#38 = B_SPLINE_CURVE_WITH_KNOTS('',3,(#49556,#49557,#49558,#49559,#49560,
#49561,#49562,#49563,#49564,#49565,#49566,#49567,#49568,#49569,#49570,#49571,
#49572,#49573,#49574),.UNSPECIFIED.,.F.,.F.,(4,2,2,2,3,2,2,2,4),(1.45762049263555,
1.57906514727215,1.70050980190876,1.82200189604475,1.94349399018073,2.06498608431671,
2.18647817845269,2.3079228330893,2.42936748772591),.UNSPECIFIED.) ;
#39 = B_SPLINE_CURVE_WITH_KNOTS('',3,(#49577,#49578,#49579,#49580,#49581,
#49582,#49583,#49584,#49585,#49586,#49587,#49588,#49589,#49590,#49591,#49592,
#49593,#49594),.UNSPECIFIED.,.F.,.F.,(4,2,2,2,2,2,2,2,4),(0.485873497545182,
0.60731815218179,0.728762806818399,0.850254900954381,0.971746995090364,
1.09323908922635,1.21473118336233,1.33617583799894,1.45762049263555),
 .UNSPECIFIED.) ;
#40 = B_SPLINE_CURVE_WITH_KNOTS('',3,(#49597,#49598,#49599,#49600,#49601,
#49602,#49603,#49604,#49605,#49606,#49607,#49608,#49609,#49610,#49611,#49612,
#49613,#49614),.UNSPECIFIED.,.F.,.F.,(4,2,2,2,2,2,2,2,4),(0.485873497545182,
0.607318152181791,0.728762806818399,0.850254900954382,0.971746995090364,
1.09323908922635,1.21473118336233,1.33617583799894,1.45762049263555),
 .UNSPECIFIED.) ;
#41 = B_SPLINE_CURVE_WITH_KNOTS('',3,(#49615,#49616,#49617,#49618,#49619,
#49620,#49621,#49622,#49623,#49624,#49625,#49626,#49627,#49628,#49629,#49630,
#49631,#49632,#49633),.UNSPECIFIED.,.F.,.F.,(4,2,2,2,3,2,2,2,4),(1.45762049263555,
1.57906514727215,1.70050980190876,1.82200189604475,1.94349399018073,2.06498608431671,
2.18647817845269,2.3079228330893,2.42936748772591),.UNSPECIFIED.) ;
#42 = B_SPLINE_CURVE_WITH_KNOTS('',3,(#49640,#49641,#49642,#49643,#49644,
#49645,#49646,#49647,#49648,#49649,#49650,#49651,#49652,#49653,#49654,#49655,
#49656,#49657),.UNSPECIFIED.,.F.,.F.,(4,2,2,2,2,2,2,2,4),(0.485873497545182,
0.607318152181791,0.728762806818399,0.850254900954382,0.971746995090364,
1.09323908922635,1.21473118336233,1.33617583799894,1.45762049263555),
 .UNSPECIFIED.) ;
#43 = B_SPLINE_CURVE_WITH_KNOTS('',3,(#49658,#49659,#49660,#49661,#49662,
#49663,#49664,#49665,#49666,#49667,#49668,#49669,#49670,#49671,#49672,#49673,
#49674,#49675,#49676),.UNSPECIFIED.,.F.,.F.,(4,2,2,2,3,2,2,2,4),(1.45762049263555,
1.57906514727215,1.70050980190876,1.82200189604475,1.94349399018073,2.06498608431671,
2.18647817845269,2.3079228330893,2.42936748772591),.UNSPECIFIED.) ;
#44 = B_SPLINE_CURVE_WITH_KNOTS('',3,(#49680,#49681,#49682,#49683,#49684,
#49685,#49686,#49687,#49688,#49689,#49690,#49691,#49692,#49693,#49694,#49695,
#49696,#49697,#49698),.UNSPECIFIED.,.F.,.F.,(4,2,2,2,3,2,2,2,4),(1.45762049263555,
1.57906514727215,1.70050980190876,1.82200189604475,1.94349399018073,2.06498608431671,
2.18647817845269,2.3079228330893,2.42936748772591),.UNSPECIFIED.) ;
#45 = B_SPLINE_CURVE_WITH_KNOTS('',3,(#49699,#49700,#49701,#49702,#49703,
#49704,#49705,#49706,#49707,#49708,#49709,#49710,#49711,#49712,#49713,#49714,
#49715,#49716),.UNSPECIFIED.,.F.,.F.,(4,2,2,2,2,2,2,2,4),(0.485873497545182,
0.60731815218179,0.728762806818399,0.850254900954381,0.971746995090364,
1.09323908922635,1.21473118336233,1.33617583799894,1.45762049263555),
 .UNSPECIFIED.) ;
#46 = B_SPLINE_CURVE_WITH_KNOTS('',3,(#50119,#50120,#50121,#50122,#50123,
#50124,#50125,#50126,#50127,#50128,#50129,#50130,#50131,#50132,#50133,#50134,
#50135,#50136,#50137,#50138,#50139,#50140),.UNSPECIFIED.,.F.,.F.,(4,2,2,
2,2,2,2,2,2,2,4),(0.921102242512175,0.924013514464762,0.972179762855851,
1.06851225963803,1.16823933679329,1.26796641394856,1.36769349110382,1.46742056825909,
1.56375306504127,1.61191931343235,1.61483058538494),.UNSPECIFIED.) ;
#47 = B_SPLINE_CURVE_WITH_KNOTS('',3,(#50266,#50267,#50268,#50269,#50270,
#50271,#50272,#50273,#50274,#50275,#50276,#50277),.UNSPECIFIED.,.F.,.F.,
(4,2,2,2,2,4),(0.0455189062767866,0.0517682265718383,0.103536453143677,
0.207072906287353,0.299969895185651,0.392866884083948),.UNSPECIFIED.) ;
#48 = B_SPLINE_CURVE_WITH_KNOTS('',3,(#50281,#50282,#50283,#50284,#50285,
#50286,#50287,#50288,#50289,#50290,#50291,#50292),.UNSPECIFIED.,.F.,.F.,
(4,2,2,2,2,4),(0.392866884083948,0.485763872982246,0.578660861880544,0.68219731502422,
0.733965541596058,0.74021486189111),.UNSPECIFIED.) ;
#49 = ORIENTED_CLOSED_SHELL('',*,#28635,.F.) ;
#50 = ORIENTED_CLOSED_SHELL('',*,#28636,.F.) ;
#51 = ORIENTED_CLOSED_SHELL('',*,#28637,.F.) ;
#52 = ORIENTED_CLOSED_SHELL('',*,#28638,.F.) ;
#53 = ORIENTED_CLOSED_SHELL('',*,#28639,.F.) ;
#54 = ORIENTED_CLOSED_SHELL('',*,#28640,.F.) ;
#55 = ORIENTED_CLOSED_SHELL('',*,#28641,.F.) ;
#56 = ORIENTED_CLOSED_SHELL('',*,#28642,.F.) ;
#57 = ORIENTED_CLOSED_SHELL('',*,#28643,.F.) ;
#58 = ORIENTED_CLOSED_SHELL('',*,#28644,.F.) ;
#59 = ORIENTED_CLOSED_SHELL('',*,#28645,.F.) ;
#60 = ORIENTED_CLOSED_SHELL('',*,#28646,.F.) ;
#61 = ORIENTED_CLOSED_SHELL('',*,#28647,.F.) ;
#62 = ORIENTED_CLOSED_SHELL('',*,#28648,.F.) ;
#63 = ORIENTED_CLOSED_SHELL('',*,#28649,.F.) ;
#64 = ORIENTED_CLOSED_SHELL('',*,#28650,.F.) ;
#65 = ORIENTED_CLOSED_SHELL('',*,#28651,.F.) ;
#66 = ORIENTED_CLOSED_SHELL('',*,#28652,.F.) ;
#67 = ORIENTED_CLOSED_SHELL('',*,#28653,.F.) ;
#68 = ORIENTED_CLOSED_SHELL('',*,#28679,.F.) ;
#69 = ORIENTED_CLOSED_SHELL('',*,#28680,.F.) ;
#70 = ORIENTED_CLOSED_SHELL('',*,#28681,.F.) ;
#71 = ORIENTED_CLOSED_SHELL('',*,#28682,.F.) ;
#72 = ORIENTED_CLOSED_SHELL('',*,#28684,.F.) ;
#73 = ORIENTED_CLOSED_SHELL('',*,#28685,.F.) ;
#74 = ORIENTED_CLOSED_SHELL('',*,#28686,.F.) ;
#75 = ORIENTED_CLOSED_SHELL('',*,#28687,.F.) ;
#76 = ORIENTED_CLOSED_SHELL('',*,#28688,.F.) ;
#77 = ORIENTED_CLOSED_SHELL('',*,#28697,.F.) ;
#78 = ORIENTED_CLOSED_SHELL('',*,#28698,.F.) ;
#79 = BREP_WITH_VOIDS('TUBULAR_3POINT_HITCH_FRAME',#28634,(#49,#50,#51,#52,
#53,#54,#55,#56,#57,#58,#59,#60,#61,#62,#63,#64,#65,#66,#67)) ;
#80 = BREP_WITH_VOIDS('CONTROL_CABLE_SHEATH',#28683,(#68,#69,#70,#71,#72,
#73,#74,#75,#76)) ;
#81 = BREP_WITH_VOIDS('OSCILLATING_SPOUT_TUBE',#28699,(#77,#78)) ;
#82 = ITEM_DEFINED_TRANSFORMATION($,$,#29213,#29914) ;
#83 = ITEM_DEFINED_TRANSFORMATION($,$,#29312,#29915) ;
#84 = ITEM_DEFINED_TRANSFORMATION($,$,#29330,#29916) ;
#85 = ITEM_DEFINED_TRANSFORMATION($,$,#29330,#29917) ;
#86 = ITEM_DEFINED_TRANSFORMATION($,$,#29339,#29918) ;
#87 = ITEM_DEFINED_TRANSFORMATION($,$,#29730,#29919) ;
#88 = ITEM_DEFINED_TRANSFORMATION($,$,#29921,#30275) ;
#89 = ITEM_DEFINED_TRANSFORMATION($,$,#30246,#30276) ;
#90 = ITEM_DEFINED_TRANSFORMATION($,$,#30246,#30277) ;
#91 = ITEM_DEFINED_TRANSFORMATION($,$,#30246,#30278) ;
#92 = ITEM_DEFINED_TRANSFORMATION($,$,#30246,#30279) ;
#93 = ITEM_DEFINED_TRANSFORMATION($,$,#30253,#30280) ;
#94 = ITEM_DEFINED_TRANSFORMATION($,$,#30253,#30281) ;
#95 = ITEM_DEFINED_TRANSFORMATION($,$,#30264,#30282) ;
#96 = ITEM_DEFINED_TRANSFORMATION($,$,#30284,#30663) ;
#97 = ITEM_DEFINED_TRANSFORMATION($,$,#30394,#30664) ;
#98 = ITEM_DEFINED_TRANSFORMATION($,$,#30407,#30665) ;
#99 = ITEM_DEFINED_TRANSFORMATION($,$,#30509,#30666) ;
#100 = ITEM_DEFINED_TRANSFORMATION($,$,#30518,#30667) ;
#101 = ITEM_DEFINED_TRANSFORMATION($,$,#30539,#30668) ;
#102 = ITEM_DEFINED_TRANSFORMATION($,$,#30545,#30669) ;
#103 = ITEM_DEFINED_TRANSFORMATION($,$,#30558,#30670) ;
#104 = ITEM_DEFINED_TRANSFORMATION($,$,#30580,#30671) ;
#105 = ITEM_DEFINED_TRANSFORMATION($,$,#30654,#30672) ;
#106 = ITEM_DEFINED_TRANSFORMATION($,$,#30674,#32067) ;
#107 = ITEM_DEFINED_TRANSFORMATION($,$,#30734,#32068) ;
#108 = ITEM_DEFINED_TRANSFORMATION($,$,#30765,#32069) ;
#109 = ITEM_DEFINED_TRANSFORMATION($,$,#30808,#32070) ;
#110 = ITEM_DEFINED_TRANSFORMATION($,$,#30841,#32071) ;
#111 = ITEM_DEFINED_TRANSFORMATION($,$,#30860,#32072) ;
#112 = ITEM_DEFINED_TRANSFORMATION($,$,#30891,#32073) ;
#113 = ITEM_DEFINED_TRANSFORMATION($,$,#30925,#32074) ;
#114 = ITEM_DEFINED_TRANSFORMATION($,$,#30932,#32075) ;
#115 = ITEM_DEFINED_TRANSFORMATION($,$,#30942,#32076) ;
#116 = ITEM_DEFINED_TRANSFORMATION($,$,#31036,#32077) ;
#117 = ITEM_DEFINED_TRANSFORMATION($,$,#31057,#32078) ;
#118 = ITEM_DEFINED_TRANSFORMATION($,$,#31063,#32079) ;
#119 = ITEM_DEFINED_TRANSFORMATION($,$,#31069,#32080) ;
#120 = ITEM_DEFINED_TRANSFORMATION($,$,#32082,#32200) ;
#121 = ITEM_DEFINED_TRANSFORMATION($,$,#32118,#32201) ;
#122 = ITEM_DEFINED_TRANSFORMATION($,$,#32157,#32202) ;
#123 = ITEM_DEFINED_TRANSFORMATION($,$,#32157,#32203) ;
#124 = ITEM_DEFINED_TRANSFORMATION($,$,#32166,#32204) ;
#125 = ITEM_DEFINED_TRANSFORMATION($,$,#32183,#32205) ;
#126 = ITEM_DEFINED_TRANSFORMATION($,$,#32277,#32365) ;
#127 = ITEM_DEFINED_TRANSFORMATION($,$,#32277,#32366) ;
#128 = ITEM_DEFINED_TRANSFORMATION($,$,#32277,#32367) ;
#129 = ITEM_DEFINED_TRANSFORMATION($,$,#32207,#32368) ;
#130 = ITEM_DEFINED_TRANSFORMATION($,$,#32207,#32369) ;
#131 = ITEM_DEFINED_TRANSFORMATION($,$,#32207,#32370) ;
#132 = ITEM_DEFINED_TRANSFORMATION($,$,#32207,#32371) ;
#133 = ITEM_DEFINED_TRANSFORMATION($,$,#32220,#32372) ;
#134 = ITEM_DEFINED_TRANSFORMATION($,$,#32220,#32373) ;
#135 = ITEM_DEFINED_TRANSFORMATION($,$,#32220,#32374) ;
#136 = ITEM_DEFINED_TRANSFORMATION($,$,#32220,#32375) ;
#137 = ITEM_DEFINED_TRANSFORMATION($,$,#32232,#32376) ;
#138 = ITEM_DEFINED_TRANSFORMATION($,$,#32232,#32377) ;
#139 = ITEM_DEFINED_TRANSFORMATION($,$,#32232,#32378) ;
#140 = ITEM_DEFINED_TRANSFORMATION($,$,#32232,#32379) ;
#141 = ITEM_DEFINED_TRANSFORMATION($,$,#32245,#32380) ;
#142 = ITEM_DEFINED_TRANSFORMATION($,$,#32257,#32381) ;
#143 = ITEM_DEFINED_TRANSFORMATION($,$,#32267,#32382) ;
#144 = ITEM_DEFINED_TRANSFORMATION($,$,#32277,#32383) ;
#145 = ITEM_DEFINED_TRANSFORMATION($,$,#32277,#32384) ;
#146 = ITEM_DEFINED_TRANSFORMATION($,$,#29212,#32385) ;
#147 = ITEM_DEFINED_TRANSFORMATION($,$,#29920,#32386) ;
#148 = ITEM_DEFINED_TRANSFORMATION($,$,#30283,#32387) ;
#149 = ITEM_DEFINED_TRANSFORMATION($,$,#30673,#32388) ;
#150 = ITEM_DEFINED_TRANSFORMATION($,$,#32081,#32389) ;
#151 = ITEM_DEFINED_TRANSFORMATION($,$,#32206,#32390) ;
#152 = (
REPRESENTATION_RELATIONSHIP($,$,#50621,#50620)
REPRESENTATION_RELATIONSHIP_WITH_TRANSFORMATION(#82)
SHAPE_REPRESENTATION_RELATIONSHIP()
) ;
#153 = (
REPRESENTATION_RELATIONSHIP($,$,#50622,#50620)
REPRESENTATION_RELATIONSHIP_WITH_TRANSFORMATION(#83)
SHAPE_REPRESENTATION_RELATIONSHIP()
) ;
#154 = (
REPRESENTATION_RELATIONSHIP($,$,#50623,#50620)
REPRESENTATION_RELATIONSHIP_WITH_TRANSFORMATION(#84)
SHAPE_REPRESENTATION_RELATIONSHIP()
) ;
#155 = (
REPRESENTATION_RELATIONSHIP($,$,#50623,#50620)
REPRESENTATION_RELATIONSHIP_WITH_TRANSFORMATION(#85)
SHAPE_REPRESENTATION_RELATIONSHIP()
) ;
#156 = (
REPRESENTATION_RELATIONSHIP($,$,#50624,#50620)
REPRESENTATION_RELATIONSHIP_WITH_TRANSFORMATION(#86)
SHAPE_REPRESENTATION_RELATIONSHIP()
) ;
#157 = (
REPRESENTATION_RELATIONSHIP($,$,#50625,#50620)
REPRESENTATION_RELATIONSHIP_WITH_TRANSFORMATION(#87)
SHAPE_REPRESENTATION_RELATIONSHIP()
) ;
#158 = (
REPRESENTATION_RELATIONSHIP($,$,#50627,#50626)
REPRESENTATION_RELATIONSHIP_WITH_TRANSFORMATION(#88)
SHAPE_REPRESENTATION_RELATIONSHIP()
) ;
#159 = (
REPRESENTATION_RELATIONSHIP($,$,#50628,#50626)
REPRESENTATION_RELATIONSHIP_WITH_TRANSFORMATION(#89)
SHAPE_REPRESENTATION_RELATIONSHIP()
) ;
#160 = (
REPRESENTATION_RELATIONSHIP($,$,#50628,#50626)
REPRESENTATION_RELATIONSHIP_WITH_TRANSFORMATION(#90)
SHAPE_REPRESENTATION_RELATIONSHIP()
) ;
#161 = (
REPRESENTATION_RELATIONSHIP($,$,#50628,#50626)
REPRESENTATION_RELATIONSHIP_WITH_TRANSFORMATION(#91)
SHAPE_REPRESENTATION_RELATIONSHIP()
) ;
#162 = (
REPRESENTATION_RELATIONSHIP($,$,#50628,#50626)
REPRESENTATION_RELATIONSHIP_WITH_TRANSFORMATION(#92)
SHAPE_REPRESENTATION_RELATIONSHIP()
) ;
#163 = (
REPRESENTATION_RELATIONSHIP($,$,#50629,#50626)
REPRESENTATION_RELATIONSHIP_WITH_TRANSFORMATION(#93)
SHAPE_REPRESENTATION_RELATIONSHIP()
) ;
#164 = (
REPRESENTATION_RELATIONSHIP($,$,#50629,#50626)
REPRESENTATION_RELATIONSHIP_WITH_TRANSFORMATION(#94)
SHAPE_REPRESENTATION_RELATIONSHIP()
) ;
#165 = (
REPRESENTATION_RELATIONSHIP($,$,#50630,#50626)
REPRESENTATION_RELATIONSHIP_WITH_TRANSFORMATION(#95)
SHAPE_REPRESENTATION_RELATIONSHIP()
) ;
#166 = (
REPRESENTATION_RELATIONSHIP($,$,#50632,#50631)
REPRESENTATION_RELATIONSHIP_WITH_TRANSFORMATION(#96)
SHAPE_REPRESENTATION_RELATIONSHIP()
) ;
#167 = (
REPRESENTATION_RELATIONSHIP($,$,#50633,#50631)
REPRESENTATION_RELATIONSHIP_WITH_TRANSFORMATION(#97)
SHAPE_REPRESENTATION_RELATIONSHIP()
) ;
#168 = (
REPRESENTATION_RELATIONSHIP($,$,#50634,#50631)
REPRESENTATION_RELATIONSHIP_WITH_TRANSFORMATION(#98)
SHAPE_REPRESENTATION_RELATIONSHIP()
) ;
#169 = (
REPRESENTATION_RELATIONSHIP($,$,#50635,#50631)
REPRESENTATION_RELATIONSHIP_WITH_TRANSFORMATION(#99)
SHAPE_REPRESENTATION_RELATIONSHIP()
) ;
#170 = (
REPRESENTATION_RELATIONSHIP($,$,#50636,#50631)
REPRESENTATION_RELATIONSHIP_WITH_TRANSFORMATION(#100)
SHAPE_REPRESENTATION_RELATIONSHIP()
) ;
#171 = (
REPRESENTATION_RELATIONSHIP($,$,#50637,#50631)
REPRESENTATION_RELATIONSHIP_WITH_TRANSFORMATION(#101)
SHAPE_REPRESENTATION_RELATIONSHIP()
) ;
#172 = (
REPRESENTATION_RELATIONSHIP($,$,#50638,#50631)
REPRESENTATION_RELATIONSHIP_WITH_TRANSFORMATION(#102)
SHAPE_REPRESENTATION_RELATIONSHIP()
) ;
#173 = (
REPRESENTATION_RELATIONSHIP($,$,#50639,#50631)
REPRESENTATION_RELATIONSHIP_WITH_TRANSFORMATION(#103)
SHAPE_REPRESENTATION_RELATIONSHIP()
) ;
#174 = (
REPRESENTATION_RELATIONSHIP($,$,#50640,#50631)
REPRESENTATION_RELATIONSHIP_WITH_TRANSFORMATION(#104)
SHAPE_REPRESENTATION_RELATIONSHIP()
) ;
#175 = (
REPRESENTATION_RELATIONSHIP($,$,#50641,#50631)
REPRESENTATION_RELATIONSHIP_WITH_TRANSFORMATION(#105)
SHAPE_REPRESENTATION_RELATIONSHIP()
) ;
#176 = (
REPRESENTATION_RELATIONSHIP($,$,#50643,#50642)
REPRESENTATION_RELATIONSHIP_WITH_TRANSFORMATION(#106)
SHAPE_REPRESENTATION_RELATIONSHIP()
) ;
#177 = (
REPRESENTATION_RELATIONSHIP($,$,#50644,#50642)
REPRESENTATION_RELATIONSHIP_WITH_TRANSFORMATION(#107)
SHAPE_REPRESENTATION_RELATIONSHIP()
) ;
#178 = (
REPRESENTATION_RELATIONSHIP($,$,#50645,#50642)
REPRESENTATION_RELATIONSHIP_WITH_TRANSFORMATION(#108)
SHAPE_REPRESENTATION_RELATIONSHIP()
) ;
#179 = (
REPRESENTATION_RELATIONSHIP($,$,#50646,#50642)
REPRESENTATION_RELATIONSHIP_WITH_TRANSFORMATION(#109)
SHAPE_REPRESENTATION_RELATIONSHIP()
) ;
#180 = (
REPRESENTATION_RELATIONSHIP($,$,#50647,#50642)
REPRESENTATION_RELATIONSHIP_WITH_TRANSFORMATION(#110)
SHAPE_REPRESENTATION_RELATIONSHIP()
) ;
#181 = (
REPRESENTATION_RELATIONSHIP($,$,#50648,#50642)
REPRESENTATION_RELATIONSHIP_WITH_TRANSFORMATION(#111)
SHAPE_REPRESENTATION_RELATIONSHIP()
) ;
#182 = (
REPRESENTATION_RELATIONSHIP($,$,#50649,#50642)
REPRESENTATION_RELATIONSHIP_WITH_TRANSFORMATION(#112)
SHAPE_REPRESENTATION_RELATIONSHIP()
) ;
#183 = (
REPRESENTATION_RELATIONSHIP($,$,#50650,#50642)
REPRESENTATION_RELATIONSHIP_WITH_TRANSFORMATION(#113)
SHAPE_REPRESENTATION_RELATIONSHIP()
) ;
#184 = (
REPRESENTATION_RELATIONSHIP($,$,#50651,#50642)
REPRESENTATION_RELATIONSHIP_WITH_TRANSFORMATION(#114)
SHAPE_REPRESENTATION_RELATIONSHIP()
) ;
#185 = (
REPRESENTATION_RELATIONSHIP($,$,#50652,#50642)
REPRESENTATION_RELATIONSHIP_WITH_TRANSFORMATION(#115)
SHAPE_REPRESENTATION_RELATIONSHIP()
) ;
#186 = (
REPRESENTATION_RELATIONSHIP($,$,#50653,#50642)
REPRESENTATION_RELATIONSHIP_WITH_TRANSFORMATION(#116)
SHAPE_REPRESENTATION_RELATIONSHIP()
) ;
#187 = (
REPRESENTATION_RELATIONSHIP($,$,#50654,#50642)
REPRESENTATION_RELATIONSHIP_WITH_TRANSFORMATION(#117)
SHAPE_REPRESENTATION_RELATIONSHIP()
) ;
#188 = (
REPRESENTATION_RELATIONSHIP($,$,#50655,#50642)
REPRESENTATION_RELATIONSHIP_WITH_TRANSFORMATION(#118)
SHAPE_REPRESENTATION_RELATIONSHIP()
) ;
#189 = (
REPRESENTATION_RELATIONSHIP($,$,#50656,#50642)
REPRESENTATION_RELATIONSHIP_WITH_TRANSFORMATION(#119)
SHAPE_REPRESENTATION_RELATIONSHIP()
) ;
#190 = (
REPRESENTATION_RELATIONSHIP($,$,#50658,#50657)
REPRESENTATION_RELATIONSHIP_WITH_TRANSFORMATION(#120)
SHAPE_REPRESENTATION_RELATIONSHIP()
) ;
#191 = (
REPRESENTATION_RELATIONSHIP($,$,#50659,#50657)
REPRESENTATION_RELATIONSHIP_WITH_TRANSFORMATION(#121)
SHAPE_REPRESENTATION_RELATIONSHIP()
) ;
#192 = (
REPRESENTATION_RELATIONSHIP($,$,#50660,#50657)
REPRESENTATION_RELATIONSHIP_WITH_TRANSFORMATION(#122)
SHAPE_REPRESENTATION_RELATIONSHIP()
) ;
#193 = (
REPRESENTATION_RELATIONSHIP($,$,#50660,#50657)
REPRESENTATION_RELATIONSHIP_WITH_TRANSFORMATION(#123)
SHAPE_REPRESENTATION_RELATIONSHIP()
) ;
#194 = (
REPRESENTATION_RELATIONSHIP($,$,#50661,#50657)
REPRESENTATION_RELATIONSHIP_WITH_TRANSFORMATION(#124)
SHAPE_REPRESENTATION_RELATIONSHIP()
) ;
#195 = (
REPRESENTATION_RELATIONSHIP($,$,#50662,#50657)
REPRESENTATION_RELATIONSHIP_WITH_TRANSFORMATION(#125)
SHAPE_REPRESENTATION_RELATIONSHIP()
) ;
#196 = (
REPRESENTATION_RELATIONSHIP($,$,#50670,#50663)
REPRESENTATION_RELATIONSHIP_WITH_TRANSFORMATION(#126)
SHAPE_REPRESENTATION_RELATIONSHIP()
) ;
#197 = (
REPRESENTATION_RELATIONSHIP($,$,#50670,#50663)
REPRESENTATION_RELATIONSHIP_WITH_TRANSFORMATION(#127)
SHAPE_REPRESENTATION_RELATIONSHIP()
) ;
#198 = (
REPRESENTATION_RELATIONSHIP($,$,#50670,#50663)
REPRESENTATION_RELATIONSHIP_WITH_TRANSFORMATION(#128)
SHAPE_REPRESENTATION_RELATIONSHIP()
) ;
#199 = (
REPRESENTATION_RELATIONSHIP($,$,#50664,#50663)
REPRESENTATION_RELATIONSHIP_WITH_TRANSFORMATION(#129)
SHAPE_REPRESENTATION_RELATIONSHIP()
) ;
#200 = (
REPRESENTATION_RELATIONSHIP($,$,#50664,#50663)
REPRESENTATION_RELATIONSHIP_WITH_TRANSFORMATION(#130)
SHAPE_REPRESENTATION_RELATIONSHIP()
) ;
#201 = (
REPRESENTATION_RELATIONSHIP($,$,#50664,#50663)
REPRESENTATION_RELATIONSHIP_WITH_TRANSFORMATION(#131)
SHAPE_REPRESENTATION_RELATIONSHIP()
) ;
#202 = (
REPRESENTATION_RELATIONSHIP($,$,#50664,#50663)
REPRESENTATION_RELATIONSHIP_WITH_TRANSFORMATION(#132)
SHAPE_REPRESENTATION_RELATIONSHIP()
) ;
#203 = (
REPRESENTATION_RELATIONSHIP($,$,#50665,#50663)
REPRESENTATION_RELATIONSHIP_WITH_TRANSFORMATION(#133)
SHAPE_REPRESENTATION_RELATIONSHIP()
) ;
#204 = (
REPRESENTATION_RELATIONSHIP($,$,#50665,#50663)
REPRESENTATION_RELATIONSHIP_WITH_TRANSFORMATION(#134)
SHAPE_REPRESENTATION_RELATIONSHIP()
) ;
#205 = (
REPRESENTATION_RELATIONSHIP($,$,#50665,#50663)
REPRESENTATION_RELATIONSHIP_WITH_TRANSFORMATION(#135)
SHAPE_REPRESENTATION_RELATIONSHIP()
) ;
#206 = (
REPRESENTATION_RELATIONSHIP($,$,#50665,#50663)
REPRESENTATION_RELATIONSHIP_WITH_TRANSFORMATION(#136)
SHAPE_REPRESENTATION_RELATIONSHIP()
) ;
#207 = (
REPRESENTATION_RELATIONSHIP($,$,#50666,#50663)
REPRESENTATION_RELATIONSHIP_WITH_TRANSFORMATION(#137)
SHAPE_REPRESENTATION_RELATIONSHIP()
) ;
#208 = (
REPRESENTATION_RELATIONSHIP($,$,#50666,#50663)
REPRESENTATION_RELATIONSHIP_WITH_TRANSFORMATION(#138)
SHAPE_REPRESENTATION_RELATIONSHIP()
) ;
#209 = (
REPRESENTATION_RELATIONSHIP($,$,#50666,#50663)
REPRESENTATION_RELATIONSHIP_WITH_TRANSFORMATION(#139)
SHAPE_REPRESENTATION_RELATIONSHIP()
) ;
#210 = (
REPRESENTATION_RELATIONSHIP($,$,#50666,#50663)
REPRESENTATION_RELATIONSHIP_WITH_TRANSFORMATION(#140)
SHAPE_REPRESENTATION_RELATIONSHIP()
) ;
#211 = (
REPRESENTATION_RELATIONSHIP($,$,#50667,#50663)
REPRESENTATION_RELATIONSHIP_WITH_TRANSFORMATION(#141)
SHAPE_REPRESENTATION_RELATIONSHIP()
) ;
#212 = (
REPRESENTATION_RELATIONSHIP($,$,#50668,#50663)
REPRESENTATION_RELATIONSHIP_WITH_TRANSFORMATION(#142)
SHAPE_REPRESENTATION_RELATIONSHIP()
) ;
#213 = (
REPRESENTATION_RELATIONSHIP($,$,#50669,#50663)
REPRESENTATION_RELATIONSHIP_WITH_TRANSFORMATION(#143)
SHAPE_REPRESENTATION_RELATIONSHIP()
) ;
#214 = (
REPRESENTATION_RELATIONSHIP($,$,#50670,#50663)
REPRESENTATION_RELATIONSHIP_WITH_TRANSFORMATION(#144)
SHAPE_REPRESENTATION_RELATIONSHIP()
) ;
#215 = (
REPRESENTATION_RELATIONSHIP($,$,#50670,#50663)
REPRESENTATION_RELATIONSHIP_WITH_TRANSFORMATION(#145)
SHAPE_REPRESENTATION_RELATIONSHIP()
) ;
#216 = (
REPRESENTATION_RELATIONSHIP($,$,#50620,#50619)
REPRESENTATION_RELATIONSHIP_WITH_TRANSFORMATION(#146)
SHAPE_REPRESENTATION_RELATIONSHIP()
) ;
#217 = (
REPRESENTATION_RELATIONSHIP($,$,#50626,#50619)
REPRESENTATION_RELATIONSHIP_WITH_TRANSFORMATION(#147)
SHAPE_REPRESENTATION_RELATIONSHIP()
) ;
#218 = (
REPRESENTATION_RELATIONSHIP($,$,#50631,#50619)
REPRESENTATION_RELATIONSHIP_WITH_TRANSFORMATION(#148)
SHAPE_REPRESENTATION_RELATIONSHIP()
) ;
#219 = (
REPRESENTATION_RELATIONSHIP($,$,#50642,#50619)
REPRESENTATION_RELATIONSHIP_WITH_TRANSFORMATION(#149)
SHAPE_REPRESENTATION_RELATIONSHIP()
) ;
#220 = (
REPRESENTATION_RELATIONSHIP($,$,#50657,#50619)
REPRESENTATION_RELATIONSHIP_WITH_TRANSFORMATION(#150)
SHAPE_REPRESENTATION_RELATIONSHIP()
) ;
#221 = (
REPRESENTATION_RELATIONSHIP($,$,#50663,#50619)
REPRESENTATION_RELATIONSHIP_WITH_TRANSFORMATION(#151)
SHAPE_REPRESENTATION_RELATIONSHIP()
) ;
#222 = CONTEXT_DEPENDENT_SHAPE_REPRESENTATION(#152,#50504) ;
#223 = CONTEXT_DEPENDENT_SHAPE_REPRESENTATION(#153,#50505) ;
#224 = CONTEXT_DEPENDENT_SHAPE_REPRESENTATION(#154,#50506) ;
#225 = CONTEXT_DEPENDENT_SHAPE_REPRESENTATION(#155,#50507) ;
#226 = CONTEXT_DEPENDENT_SHAPE_REPRESENTATION(#156,#50508) ;
#227 = CONTEXT_DEPENDENT_SHAPE_REPRESENTATION(#157,#50509) ;
#228 = CONTEXT_DEPENDENT_SHAPE_REPRESENTATION(#158,#50515) ;
#229 = CONTEXT_DEPENDENT_SHAPE_REPRESENTATION(#159,#50516) ;
#230 = CONTEXT_DEPENDENT_SHAPE_REPRESENTATION(#160,#50517) ;
#231 = CONTEXT_DEPENDENT_SHAPE_REPRESENTATION(#161,#50518) ;
#232 = CONTEXT_DEPENDENT_SHAPE_REPRESENTATION(#162,#50519) ;
#233 = CONTEXT_DEPENDENT_SHAPE_REPRESENTATION(#163,#50520) ;
#234 = CONTEXT_DEPENDENT_SHAPE_REPRESENTATION(#164,#50521) ;
#235 = CONTEXT_DEPENDENT_SHAPE_REPRESENTATION(#165,#50522) ;
#236 = CONTEXT_DEPENDENT_SHAPE_REPRESENTATION(#166,#50534) ;
#237 = CONTEXT_DEPENDENT_SHAPE_REPRESENTATION(#167,#50535) ;
#238 = CONTEXT_DEPENDENT_SHAPE_REPRESENTATION(#168,#50536) ;
#239 = CONTEXT_DEPENDENT_SHAPE_REPRESENTATION(#169,#50537) ;
#240 = CONTEXT_DEPENDENT_SHAPE_REPRESENTATION(#170,#50538) ;
#241 = CONTEXT_DEPENDENT_SHAPE_REPRESENTATION(#171,#50539) ;
#242 = CONTEXT_DEPENDENT_SHAPE_REPRESENTATION(#172,#50540) ;
#243 = CONTEXT_DEPENDENT_SHAPE_REPRESENTATION(#173,#50541) ;
#244 = CONTEXT_DEPENDENT_SHAPE_REPRESENTATION(#174,#50542) ;
#245 = CONTEXT_DEPENDENT_SHAPE_REPRESENTATION(#175,#50543) ;
#246 = CONTEXT_DEPENDENT_SHAPE_REPRESENTATION(#176,#50559) ;
#247 = CONTEXT_DEPENDENT_SHAPE_REPRESENTATION(#177,#50560) ;
#248 = CONTEXT_DEPENDENT_SHAPE_REPRESENTATION(#178,#50561) ;
#249 = CONTEXT_DEPENDENT_SHAPE_REPRESENTATION(#179,#50562) ;
#250 = CONTEXT_DEPENDENT_SHAPE_REPRESENTATION(#180,#50563) ;
#251 = CONTEXT_DEPENDENT_SHAPE_REPRESENTATION(#181,#50564) ;
#252 = CONTEXT_DEPENDENT_SHAPE_REPRESENTATION(#182,#50565) ;
#253 = CONTEXT_DEPENDENT_SHAPE_REPRESENTATION(#183,#50566) ;
#254 = CONTEXT_DEPENDENT_SHAPE_REPRESENTATION(#184,#50567) ;
#255 = CONTEXT_DEPENDENT_SHAPE_REPRESENTATION(#185,#50568) ;
#256 = CONTEXT_DEPENDENT_SHAPE_REPRESENTATION(#186,#50569) ;
#257 = CONTEXT_DEPENDENT_SHAPE_REPRESENTATION(#187,#50570) ;
#258 = CONTEXT_DEPENDENT_SHAPE_REPRESENTATION(#188,#50571) ;
#259 = CONTEXT_DEPENDENT_SHAPE_REPRESENTATION(#189,#50572) ;
#260 = CONTEXT_DEPENDENT_SHAPE_REPRESENTATION(#190,#50579) ;
#261 = CONTEXT_DEPENDENT_SHAPE_REPRESENTATION(#191,#50580) ;
#262 = CONTEXT_DEPENDENT_SHAPE_REPRESENTATION(#192,#50581) ;
#263 = CONTEXT_DEPENDENT_SHAPE_REPRESENTATION(#193,#50582) ;
#264 = CONTEXT_DEPENDENT_SHAPE_REPRESENTATION(#194,#50583) ;
#265 = CONTEXT_DEPENDENT_SHAPE_REPRESENTATION(#195,#50584) ;
#266 = CONTEXT_DEPENDENT_SHAPE_REPRESENTATION(#196,#50593) ;
#267 = CONTEXT_DEPENDENT_SHAPE_REPRESENTATION(#197,#50594) ;
#268 = CONTEXT_DEPENDENT_SHAPE_REPRESENTATION(#198,#50595) ;
#269 = CONTEXT_DEPENDENT_SHAPE_REPRESENTATION(#199,#50596) ;
#270 = CONTEXT_DEPENDENT_SHAPE_REPRESENTATION(#200,#50597) ;
#271 = CONTEXT_DEPENDENT_SHAPE_REPRESENTATION(#201,#50598) ;
#272 = CONTEXT_DEPENDENT_SHAPE_REPRESENTATION(#202,#50599) ;
#273 = CONTEXT_DEPENDENT_SHAPE_REPRESENTATION(#203,#50600) ;
#274 = CONTEXT_DEPENDENT_SHAPE_REPRESENTATION(#204,#50601) ;
#275 = CONTEXT_DEPENDENT_SHAPE_REPRESENTATION(#205,#50602) ;
#276 = CONTEXT_DEPENDENT_SHAPE_REPRESENTATION(#206,#50603) ;
#277 = CONTEXT_DEPENDENT_SHAPE_REPRESENTATION(#207,#50604) ;
#278 = CONTEXT_DEPENDENT_SHAPE_REPRESENTATION(#208,#50605) ;
#279 = CONTEXT_DEPENDENT_SHAPE_REPRESENTATION(#209,#50606) ;
#280 = CONTEXT_DEPENDENT_SHAPE_REPRESENTATION(#210,#50607) ;
#281 = CONTEXT_DEPENDENT_SHAPE_REPRESENTATION(#211,#50608) ;
#282 = CONTEXT_DEPENDENT_SHAPE_REPRESENTATION(#212,#50609) ;
#283 = CONTEXT_DEPENDENT_SHAPE_REPRESENTATION(#213,#50610) ;
#284 = CONTEXT_DEPENDENT_SHAPE_REPRESENTATION(#214,#50611) ;
#285 = CONTEXT_DEPENDENT_SHAPE_REPRESENTATION(#215,#50612) ;
#286 = CONTEXT_DEPENDENT_SHAPE_REPRESENTATION(#216,#50613) ;
#287 = CONTEXT_DEPENDENT_SHAPE_REPRESENTATION(#217,#50614) ;
#288 = CONTEXT_DEPENDENT_SHAPE_REPRESENTATION(#218,#50615) ;
#289 = CONTEXT_DEPENDENT_SHAPE_REPRESENTATION(#219,#50616) ;
#290 = CONTEXT_DEPENDENT_SHAPE_REPRESENTATION(#220,#50617) ;
#291 = CONTEXT_DEPENDENT_SHAPE_REPRESENTATION(#221,#50618) ;
#292 = NEXT_ASSEMBLY_USAGE_OCCURRENCE('CONICAL_POLYETHYLENE_HOPPER:1',
'CONICAL_POLYETHYLENE_HOPPER:1','CONICAL_POLYETHYLENE_HOPPER:1',#50673,
#50674,'CONICAL_POLYETHYLENE_HOPPER:1') ;
#293 = NEXT_ASSEMBLY_USAGE_OCCURRENCE('HOPPER_LID:1','HOPPER_LID:1',
'HOPPER_LID:1',#50673,#50675,'HOPPER_LID:1') ;
#294 = NEXT_ASSEMBLY_USAGE_OCCURRENCE('LID_HINGE_STRAP:1',
'LID_HINGE_STRAP:1','LID_HINGE_STRAP:1',#50673,#50676,
'LID_HINGE_STRAP:1') ;
#295 = NEXT_ASSEMBLY_USAGE_OCCURRENCE('LID_HINGE_STRAP:2',
'LID_HINGE_STRAP:2','LID_HINGE_STRAP:2',#50673,#50676,
'LID_HINGE_STRAP:2') ;
#296 = NEXT_ASSEMBLY_USAGE_OCCURRENCE('HOPPER_SIEVE_GRID:1',
'HOPPER_SIEVE_GRID:1','HOPPER_SIEVE_GRID:1',#50673,#50677,
'HOPPER_SIEVE_GRID:1') ;
#297 = NEXT_ASSEMBLY_USAGE_OCCURRENCE('HOPPER_SUPPORT_RING:1',
'HOPPER_SUPPORT_RING:1','HOPPER_SUPPORT_RING:1',#50673,#50678,
'HOPPER_SUPPORT_RING:1') ;
#298 = NEXT_ASSEMBLY_USAGE_OCCURRENCE('TUBULAR_3POINT_HITCH_FRAME:1',
'TUBULAR_3POINT_HITCH_FRAME:1','TUBULAR_3POINT_HITCH_FRAME:1',#50679,#50680,
'TUBULAR_3POINT_HITCH_FRAME:1') ;
#299 = NEXT_ASSEMBLY_USAGE_OCCURRENCE('STAND_FOOT_PLATE:1',
'STAND_FOOT_PLATE:1','STAND_FOOT_PLATE:1',#50679,#50681,
'STAND_FOOT_PLATE:1') ;
#300 = NEXT_ASSEMBLY_USAGE_OCCURRENCE('STAND_FOOT_PLATE:2',
'STAND_FOOT_PLATE:2','STAND_FOOT_PLATE:2',#50679,#50681,
'STAND_FOOT_PLATE:2') ;
#301 = NEXT_ASSEMBLY_USAGE_OCCURRENCE('STAND_FOOT_PLATE:3',
'STAND_FOOT_PLATE:3','STAND_FOOT_PLATE:3',#50679,#50681,
'STAND_FOOT_PLATE:3') ;
#302 = NEXT_ASSEMBLY_USAGE_OCCURRENCE('STAND_FOOT_PLATE:4',
'STAND_FOOT_PLATE:4','STAND_FOOT_PLATE:4',#50679,#50681,
'STAND_FOOT_PLATE:4') ;
#303 = NEXT_ASSEMBLY_USAGE_OCCURRENCE('LOWER_LINK_PIN_CAT2:1',
'LOWER_LINK_PIN_CAT2:1','LOWER_LINK_PIN_CAT2:1',#50679,#50682,
'LOWER_LINK_PIN_CAT2:1') ;
#304 = NEXT_ASSEMBLY_USAGE_OCCURRENCE('LOWER_LINK_PIN_CAT2:2',
'LOWER_LINK_PIN_CAT2:2','LOWER_LINK_PIN_CAT2:2',#50679,#50682,
'LOWER_LINK_PIN_CAT2:2') ;
#305 = NEXT_ASSEMBLY_USAGE_OCCURRENCE('TOP_LINK_PIN_CAT2:1',
'TOP_LINK_PIN_CAT2:1','TOP_LINK_PIN_CAT2:1',#50679,#50683,
'TOP_LINK_PIN_CAT2:1') ;
#306 = NEXT_ASSEMBLY_USAGE_OCCURRENCE('GEARBOX_OSCILLATION_HOUSING:1',
'GEARBOX_OSCILLATION_HOUSING:1','GEARBOX_OSCILLATION_HOUSING:1',#50684,
#50685,'GEARBOX_OSCILLATION_HOUSING:1') ;
#307 = NEXT_ASSEMBLY_USAGE_OCCURRENCE('GEARBOX_OIL_PLUG:1',
'GEARBOX_OIL_PLUG:1','GEARBOX_OIL_PLUG:1',#50684,#50686,
'GEARBOX_OIL_PLUG:1') ;
#308 = NEXT_ASSEMBLY_USAGE_OCCURRENCE('PTO_INPUT_SHAFT_SPLINE:1',
'PTO_INPUT_SHAFT_SPLINE:1','PTO_INPUT_SHAFT_SPLINE:1',#50684,#50687,
'PTO_INPUT_SHAFT_SPLINE:1') ;
#309 = NEXT_ASSEMBLY_USAGE_OCCURRENCE('PTO_SHAFT_SEAL:1',
'PTO_SHAFT_SEAL:1','PTO_SHAFT_SEAL:1',#50684,#50688,'PTO_SHAFT_SEAL:1') ;
#310 = NEXT_ASSEMBLY_USAGE_OCCURRENCE('PTO_SHIELD_GUARD:1',
'PTO_SHIELD_GUARD:1','PTO_SHIELD_GUARD:1',#50684,#50689,
'PTO_SHIELD_GUARD:1') ;
#311 = NEXT_ASSEMBLY_USAGE_OCCURRENCE('OSCILLATION_OUTPUT_SHAFT:1',
'OSCILLATION_OUTPUT_SHAFT:1','OSCILLATION_OUTPUT_SHAFT:1',#50684,#50690,
'OSCILLATION_OUTPUT_SHAFT:1') ;
#312 = NEXT_ASSEMBLY_USAGE_OCCURRENCE('OSCILLATION_CRANK_DISC:1',
'OSCILLATION_CRANK_DISC:1','OSCILLATION_CRANK_DISC:1',#50684,#50691,
'OSCILLATION_CRANK_DISC:1') ;
#313 = NEXT_ASSEMBLY_USAGE_OCCURRENCE('CONNECTING_ROD:1',
'CONNECTING_ROD:1','CONNECTING_ROD:1',#50684,#50692,'CONNECTING_ROD:1') ;
#314 = NEXT_ASSEMBLY_USAGE_OCCURRENCE('AGITATOR_SHAFT_ASSEMBLY:1',
'AGITATOR_SHAFT_ASSEMBLY:1','AGITATOR_SHAFT_ASSEMBLY:1',#50684,#50693,
'AGITATOR_SHAFT_ASSEMBLY:1') ;
#315 = NEXT_ASSEMBLY_USAGE_OCCURRENCE('AGITATOR_SHAFT_SEAL:1',
'AGITATOR_SHAFT_SEAL:1','AGITATOR_SHAFT_SEAL:1',#50684,#50694,
'AGITATOR_SHAFT_SEAL:1') ;
#316 = NEXT_ASSEMBLY_USAGE_OCCURRENCE('GATE_HOUSING_PLATE:1',
'GATE_HOUSING_PLATE:1','GATE_HOUSING_PLATE:1',#50695,#50696,
'GATE_HOUSING_PLATE:1') ;
#317 = NEXT_ASSEMBLY_USAGE_OCCURRENCE('METERING_GATE_ORIFICE_PLATE:1',
'METERING_GATE_ORIFICE_PLATE:1','METERING_GATE_ORIFICE_PLATE:1',#50695,
#50697,'METERING_GATE_ORIFICE_PLATE:1') ;
#318 = NEXT_ASSEMBLY_USAGE_OCCURRENCE('FLOW_RATE_SCALE_STRIP:1',
'FLOW_RATE_SCALE_STRIP:1','FLOW_RATE_SCALE_STRIP:1',#50695,#50698,
'FLOW_RATE_SCALE_STRIP:1') ;
#319 = NEXT_ASSEMBLY_USAGE_OCCURRENCE('OUTLET_FUNNEL:1','OUTLET_FUNNEL:1',
'OUTLET_FUNNEL:1',#50695,#50699,'OUTLET_FUNNEL:1') ;
#320 = NEXT_ASSEMBLY_USAGE_OCCURRENCE('SPOUT_FEED_FUNNEL:1',
'SPOUT_FEED_FUNNEL:1','SPOUT_FEED_FUNNEL:1',#50695,#50700,
'SPOUT_FEED_FUNNEL:1') ;
#321 = NEXT_ASSEMBLY_USAGE_OCCURRENCE('FLOW_CONTROL_QUADRANT:1',
'FLOW_CONTROL_QUADRANT:1','FLOW_CONTROL_QUADRANT:1',#50695,#50701,
'FLOW_CONTROL_QUADRANT:1') ;
#322 = NEXT_ASSEMBLY_USAGE_OCCURRENCE(
'CABLE_ACTUATED_FLOW_CONTROL_LEVER:1',
'CABLE_ACTUATED_FLOW_CONTROL_LEVER:1',
'CABLE_ACTUATED_FLOW_CONTROL_LEVER:1',#50695,#50702,
'CABLE_ACTUATED_FLOW_CONTROL_LEVER:1') ;
#323 = NEXT_ASSEMBLY_USAGE_OCCURRENCE('LEVER_KNOB:1','LEVER_KNOB:1',
'LEVER_KNOB:1',#50695,#50703,'LEVER_KNOB:1') ;
#324 = NEXT_ASSEMBLY_USAGE_OCCURRENCE('LEVER_PIVOT_PIN:1',
'LEVER_PIVOT_PIN:1','LEVER_PIVOT_PIN:1',#50695,#50704,
'LEVER_PIVOT_PIN:1') ;
#325 = NEXT_ASSEMBLY_USAGE_OCCURRENCE('CONTROL_CABLE_SHEATH:1',
'CONTROL_CABLE_SHEATH:1','CONTROL_CABLE_SHEATH:1',#50695,#50705,
'CONTROL_CABLE_SHEATH:1') ;
#326 = NEXT_ASSEMBLY_USAGE_OCCURRENCE('CONTROL_CABLE_INNER_WIRE:1',
'CONTROL_CABLE_INNER_WIRE:1','CONTROL_CABLE_INNER_WIRE:1',#50695,#50706,
'CONTROL_CABLE_INNER_WIRE:1') ;
#327 = NEXT_ASSEMBLY_USAGE_OCCURRENCE('CABLE_END_NIPPLE:1',
'CABLE_END_NIPPLE:1','CABLE_END_NIPPLE:1',#50695,#50707,
'CABLE_END_NIPPLE:1') ;
#328 = NEXT_ASSEMBLY_USAGE_OCCURRENCE('LEVER_END_NIPPLE:1',
'LEVER_END_NIPPLE:1','LEVER_END_NIPPLE:1',#50695,#50708,
'LEVER_END_NIPPLE:1') ;
#329 = NEXT_ASSEMBLY_USAGE_OCCURRENCE('RETURN_TENSION_SPRING_ASSEMBLY:1',
'RETURN_TENSION_SPRING_ASSEMBLY:1','RETURN_TENSION_SPRING_ASSEMBLY:1',#50695,
#50709,'RETURN_TENSION_SPRING_ASSEMBLY:1') ;
#330 = NEXT_ASSEMBLY_USAGE_OCCURRENCE('OSCILLATING_SPOUT_TUBE:1',
'OSCILLATING_SPOUT_TUBE:1','OSCILLATING_SPOUT_TUBE:1',#50710,#50711,
'OSCILLATING_SPOUT_TUBE:1') ;
#331 = NEXT_ASSEMBLY_USAGE_OCCURRENCE('PENDULUM_TRUNNION_YOKE:1',
'PENDULUM_TRUNNION_YOKE:1','PENDULUM_TRUNNION_YOKE:1',#50710,#50712,
'PENDULUM_TRUNNION_YOKE:1') ;
#332 = NEXT_ASSEMBLY_USAGE_OCCURRENCE('TRUNNION_BUSHING:1',
'TRUNNION_BUSHING:1','TRUNNION_BUSHING:1',#50710,#50713,
'TRUNNION_BUSHING:1') ;
#333 = NEXT_ASSEMBLY_USAGE_OCCURRENCE('TRUNNION_BUSHING:2',
'TRUNNION_BUSHING:2','TRUNNION_BUSHING:2',#50710,#50713,
'TRUNNION_BUSHING:2') ;
#334 = NEXT_ASSEMBLY_USAGE_OCCURRENCE('SPOUT_DEFLECTOR_PLATE:1',
'SPOUT_DEFLECTOR_PLATE:1','SPOUT_DEFLECTOR_PLATE:1',#50710,#50714,
'SPOUT_DEFLECTOR_PLATE:1') ;
#335 = NEXT_ASSEMBLY_USAGE_OCCURRENCE('SPOUT_CLAMP_BAND:1',
'SPOUT_CLAMP_BAND:1','SPOUT_CLAMP_BAND:1',#50710,#50715,
'SPOUT_CLAMP_BAND:1') ;
#336 = NEXT_ASSEMBLY_USAGE_OCCURRENCE('LINCH_PIN:1','LINCH_PIN:1',
'LINCH_PIN:1',#50716,#50723,'LINCH_PIN:1') ;
#337 = NEXT_ASSEMBLY_USAGE_OCCURRENCE('LINCH_PIN:2','LINCH_PIN:2',
'LINCH_PIN:2',#50716,#50723,'LINCH_PIN:2') ;
#338 = NEXT_ASSEMBLY_USAGE_OCCURRENCE('LINCH_PIN:3','LINCH_PIN:3',
'LINCH_PIN:3',#50716,#50723,'LINCH_PIN:3') ;
#339 = NEXT_ASSEMBLY_USAGE_OCCURRENCE('GEARBOX_MOUNT_BOLT_M12x65:1',
'GEARBOX_MOUNT_BOLT_M12x65:1','GEARBOX_MOUNT_BOLT_M12x65:1',#50716,#50717,
'GEARBOX_MOUNT_BOLT_M12x65:1') ;
#340 = NEXT_ASSEMBLY_USAGE_OCCURRENCE('GEARBOX_MOUNT_BOLT_M12x65:2',
'GEARBOX_MOUNT_BOLT_M12x65:2','GEARBOX_MOUNT_BOLT_M12x65:2',#50716,#50717,
'GEARBOX_MOUNT_BOLT_M12x65:2') ;
#341 = NEXT_ASSEMBLY_USAGE_OCCURRENCE('GEARBOX_MOUNT_BOLT_M12x65:3',
'GEARBOX_MOUNT_BOLT_M12x65:3','GEARBOX_MOUNT_BOLT_M12x65:3',#50716,#50717,
'GEARBOX_MOUNT_BOLT_M12x65:3') ;
#342 = NEXT_ASSEMBLY_USAGE_OCCURRENCE('GEARBOX_MOUNT_BOLT_M12x65:4',
'GEARBOX_MOUNT_BOLT_M12x65:4','GEARBOX_MOUNT_BOLT_M12x65:4',#50716,#50717,
'GEARBOX_MOUNT_BOLT_M12x65:4') ;
#343 = NEXT_ASSEMBLY_USAGE_OCCURRENCE('GEARBOX_MOUNT_NUT_M12:1',
'GEARBOX_MOUNT_NUT_M12:1','GEARBOX_MOUNT_NUT_M12:1',#50716,#50718,
'GEARBOX_MOUNT_NUT_M12:1') ;
#344 = NEXT_ASSEMBLY_USAGE_OCCURRENCE('GEARBOX_MOUNT_NUT_M12:2',
'GEARBOX_MOUNT_NUT_M12:2','GEARBOX_MOUNT_NUT_M12:2',#50716,#50718,
'GEARBOX_MOUNT_NUT_M12:2') ;
#345 = NEXT_ASSEMBLY_USAGE_OCCURRENCE('GEARBOX_MOUNT_NUT_M12:3',
'GEARBOX_MOUNT_NUT_M12:3','GEARBOX_MOUNT_NUT_M12:3',#50716,#50718,
'GEARBOX_MOUNT_NUT_M12:3') ;
#346 = NEXT_ASSEMBLY_USAGE_OCCURRENCE('GEARBOX_MOUNT_NUT_M12:4',
'GEARBOX_MOUNT_NUT_M12:4','GEARBOX_MOUNT_NUT_M12:4',#50716,#50718,
'GEARBOX_MOUNT_NUT_M12:4') ;
#347 = NEXT_ASSEMBLY_USAGE_OCCURRENCE('GATE_HOUSING_BOLT_M8x30:1',
'GATE_HOUSING_BOLT_M8x30:1','GATE_HOUSING_BOLT_M8x30:1',#50716,#50719,
'GATE_HOUSING_BOLT_M8x30:1') ;
#348 = NEXT_ASSEMBLY_USAGE_OCCURRENCE('GATE_HOUSING_BOLT_M8x30:2',
'GATE_HOUSING_BOLT_M8x30:2','GATE_HOUSING_BOLT_M8x30:2',#50716,#50719,
'GATE_HOUSING_BOLT_M8x30:2') ;
#349 = NEXT_ASSEMBLY_USAGE_OCCURRENCE('GATE_HOUSING_BOLT_M8x30:3',
'GATE_HOUSING_BOLT_M8x30:3','GATE_HOUSING_BOLT_M8x30:3',#50716,#50719,
'GATE_HOUSING_BOLT_M8x30:3') ;
#350 = NEXT_ASSEMBLY_USAGE_OCCURRENCE('GATE_HOUSING_BOLT_M8x30:4',
'GATE_HOUSING_BOLT_M8x30:4','GATE_HOUSING_BOLT_M8x30:4',#50716,#50719,
'GATE_HOUSING_BOLT_M8x30:4') ;
#351 = NEXT_ASSEMBLY_USAGE_OCCURRENCE('LEVER_PIVOT_NUT_M10:1',
'LEVER_PIVOT_NUT_M10:1','LEVER_PIVOT_NUT_M10:1',#50716,#50720,
'LEVER_PIVOT_NUT_M10:1') ;
#352 = NEXT_ASSEMBLY_USAGE_OCCURRENCE('SPRING_HOOK_PIN:1',
'SPRING_HOOK_PIN:1','SPRING_HOOK_PIN:1',#50716,#50721,
'SPRING_HOOK_PIN:1') ;
#353 = NEXT_ASSEMBLY_USAGE_OCCURRENCE('SPRING_ANCHOR_PIN:1',
'SPRING_ANCHOR_PIN:1','SPRING_ANCHOR_PIN:1',#50716,#50722,
'SPRING_ANCHOR_PIN:1') ;
#354 = NEXT_ASSEMBLY_USAGE_OCCURRENCE('LINCH_PIN:4','LINCH_PIN:4',
'LINCH_PIN:4',#50716,#50723,'LINCH_PIN:4') ;
#355 = NEXT_ASSEMBLY_USAGE_OCCURRENCE('LINCH_PIN:5','LINCH_PIN:5',
'LINCH_PIN:5',#50716,#50723,'LINCH_PIN:5') ;
#356 = NEXT_ASSEMBLY_USAGE_OCCURRENCE('HOPPER_UNIT:1','HOPPER_UNIT:1',
'HOPPER_UNIT:1',#50672,#50673,'HOPPER_UNIT:1') ;
#357 = NEXT_ASSEMBLY_USAGE_OCCURRENCE('HITCH_FRAME_UNIT:1',
'HITCH_FRAME_UNIT:1','HITCH_FRAME_UNIT:1',#50672,#50679,
'HITCH_FRAME_UNIT:1') ;
#358 = NEXT_ASSEMBLY_USAGE_OCCURRENCE('GEARBOX_DRIVE_UNIT:1',
'GEARBOX_DRIVE_UNIT:1','GEARBOX_DRIVE_UNIT:1',#50672,#50684,
'GEARBOX_DRIVE_UNIT:1') ;
#359 = NEXT_ASSEMBLY_USAGE_OCCURRENCE('METERING_GATE_UNIT:1',
'METERING_GATE_UNIT:1','METERING_GATE_UNIT:1',#50672,#50695,
'METERING_GATE_UNIT:1') ;
#360 = NEXT_ASSEMBLY_USAGE_OCCURRENCE('SPOUT_UNIT:1','SPOUT_UNIT:1',
'SPOUT_UNIT:1',#50672,#50710,'SPOUT_UNIT:1') ;
#361 = NEXT_ASSEMBLY_USAGE_OCCURRENCE('FASTENERS:1','FASTENERS:1',
'FASTENERS:1',#50672,#50716,'FASTENERS:1') ;
#362 = ELLIPSE('',#29844,2.01265515316035,2.) ;
#363 = ELLIPSE('',#29845,2.01265515316035,2.) ;
#364 = ELLIPSE('',#29846,2.01265515316036,2.) ;
#365 = ELLIPSE('',#29847,2.01265515316036,2.) ;
#366 = ELLIPSE('',#29849,2.01265515316036,2.) ;
#367 = ELLIPSE('',#29850,2.01265515316036,2.) ;
#368 = ELLIPSE('',#29852,2.01265515316036,2.) ;
#369 = ELLIPSE('',#29853,2.01265515316036,2.) ;
#370 = ELLIPSE('',#29855,2.01265515316035,2.) ;
#371 = ELLIPSE('',#29856,2.01265515316035,2.) ;
#372 = ELLIPSE('',#29858,2.01265515316036,2.) ;
#373 = ELLIPSE('',#29859,2.01265515316036,2.) ;
#374 = ELLIPSE('',#29861,2.01265515316036,2.) ;
#375 = ELLIPSE('',#29862,2.01265515316036,2.) ;
#376 = ELLIPSE('',#29864,2.01265515316036,2.) ;
#377 = ELLIPSE('',#29865,2.01265515316036,2.) ;
#378 = ELLIPSE('',#29867,2.01265515316036,2.) ;
#379 = ELLIPSE('',#29869,2.01265515316036,2.) ;
#380 = ELLIPSE('',#29871,2.01265515316036,2.) ;
#381 = ELLIPSE('',#29873,2.01265515316035,2.) ;
#382 = ELLIPSE('',#29875,2.01265515316036,2.) ;
#383 = ELLIPSE('',#29877,2.01265515316036,2.) ;
#384 = ELLIPSE('',#29879,2.01265515316036,2.) ;
#385 = ELLIPSE('',#29881,2.01265515316036,2.) ;
#386 = ELLIPSE('',#29883,2.01265515316036,2.) ;
#387 = ELLIPSE('',#29885,2.01265515316036,2.) ;
#388 = ELLIPSE('',#29887,2.01265515316036,2.) ;
#389 = ELLIPSE('',#29889,2.01265515316036,2.) ;
#390 = ELLIPSE('',#29891,2.01265515316036,2.) ;
#391 = ELLIPSE('',#29893,2.01265515316036,2.) ;
#392 = ELLIPSE('',#29894,2.01265515316036,2.) ;
#393 = ELLIPSE('',#29896,2.01265515316036,2.) ;
#394 = ELLIPSE('',#29897,2.01265515316036,2.) ;
#395 = ELLIPSE('',#29899,2.01265515316035,2.) ;
#396 = ELLIPSE('',#29900,2.01265515316035,2.) ;
#397 = ELLIPSE('',#29902,2.01265515316036,2.) ;
#398 = ELLIPSE('',#29903,2.01265515316036,2.) ;
#399 = ELLIPSE('',#29905,2.01265515316036,2.) ;
#400 = ELLIPSE('',#29906,2.01265515316036,2.) ;
#401 = ELLIPSE('',#29908,2.01265515316036,2.) ;
#402 = ELLIPSE('',#29909,2.01265515316036,2.) ;
#403 = ELLIPSE('',#29911,2.01265515316036,2.) ;
#404 = ELLIPSE('',#29912,2.01265515316036,2.) ;
#405 = ELLIPSE('',#30976,0.400079928078316,0.4) ;
#406 = ELLIPSE('',#30978,0.400079928078316,0.4) ;
#407 = ELLIPSE('',#30982,0.400000809214436,0.4) ;
#408 = ELLIPSE('',#30983,0.400000809214436,0.4) ;
#409 = ELLIPSE('',#30986,0.563115453389195,0.4) ;
#410 = ELLIPSE('',#30989,0.505057490139689,0.4) ;
#411 = ELLIPSE('',#30992,0.565685424949243,0.4) ;
#412 = ELLIPSE('',#30993,0.565685424949243,0.4) ;
#413 = ELLIPSE('',#31038,0.176776695296637,0.125) ;
#414 = ELLIPSE('',#31039,0.176776695296637,0.125) ;
#415 = ELLIPSE('',#31041,0.176776695296637,0.125) ;
#416 = ELLIPSE('',#31042,0.176776695296637,0.125) ;
#417 = ELLIPSE('',#31090,8.74484398085574,0.8) ;
#418 = ELLIPSE('',#31097,1.63965824641058,0.15) ;
#419 = ELLIPSE('',#31099,1.63965824641055,0.15) ;
#420 = ELLIPSE('',#31101,1.63965824641045,0.15) ;
#421 = ELLIPSE('',#31675,0.162242389830004,0.15) ;
#422 = ELLIPSE('',#31677,0.162242389830007,0.15) ;
#423 = ELLIPSE('',#31679,0.162242389830008,0.15) ;
#424 = ELLIPSE('',#31680,0.162242389830008,0.15) ;
#425 = ELLIPSE('',#31682,0.16224238983001,0.15) ;
#426 = ELLIPSE('',#31683,0.16224238983001,0.15) ;
#427 = ELLIPSE('',#31685,0.162242389830005,0.15) ;
#428 = ELLIPSE('',#31686,0.162242389830005,0.15) ;
#429 = ELLIPSE('',#31688,0.162242389830007,0.15) ;
#430 = ELLIPSE('',#31689,0.162242389830007,0.15) ;
#431 = ELLIPSE('',#31691,0.162242389830009,0.15) ;
#432 = ELLIPSE('',#31692,0.162242389830009,0.15) ;
#433 = ELLIPSE('',#31694,0.162242389830009,0.15) ;
#434 = ELLIPSE('',#31695,0.162242389830009,0.15) ;
#435 = ELLIPSE('',#31697,0.162242389830006,0.15) ;
#436 = ELLIPSE('',#31698,0.162242389830006,0.15) ;
#437 = ELLIPSE('',#31700,0.16224238983001,0.15) ;
#438 = ELLIPSE('',#31701,0.16224238983001,0.15) ;
#439 = ELLIPSE('',#31703,0.162242389830006,0.15) ;
#440 = ELLIPSE('',#31704,0.162242389830006,0.15) ;
#441 = ELLIPSE('',#31706,0.162242389830011,0.15) ;
#442 = ELLIPSE('',#31707,0.162242389830011,0.15) ;
#443 = ELLIPSE('',#31709,0.162242389830005,0.15) ;
#444 = ELLIPSE('',#31710,0.162242389830005,0.15) ;
#445 = ELLIPSE('',#31712,0.162242389830007,0.15) ;
#446 = ELLIPSE('',#31713,0.162242389830007,0.15) ;
#447 = ELLIPSE('',#31715,0.162242389830006,0.15) ;
#448 = ELLIPSE('',#31716,0.162242389830006,0.15) ;
#449 = ELLIPSE('',#31718,0.162242389830011,0.15) ;
#450 = ELLIPSE('',#31719,0.162242389830011,0.15) ;
#451 = ELLIPSE('',#31721,0.162242389830004,0.15) ;
#452 = ELLIPSE('',#31722,0.162242389830004,0.15) ;
#453 = ELLIPSE('',#31724,0.162242389830007,0.15) ;
#454 = ELLIPSE('',#31725,0.162242389830007,0.15) ;
#455 = ELLIPSE('',#31727,0.162242389830008,0.15) ;
#456 = ELLIPSE('',#31728,0.162242389830008,0.15) ;
#457 = ELLIPSE('',#31730,0.162242389830011,0.15) ;
#458 = ELLIPSE('',#31731,0.162242389830011,0.15) ;
#459 = ELLIPSE('',#31733,0.162242389830005,0.15) ;
#460 = ELLIPSE('',#31734,0.162242389830005,0.15) ;
#461 = ELLIPSE('',#31736,0.162242389830007,0.15) ;
#462 = ELLIPSE('',#31737,0.162242389830007,0.15) ;
#463 = ELLIPSE('',#31739,0.162242389830008,0.15) ;
#464 = ELLIPSE('',#31740,0.162242389830008,0.15) ;
#465 = ELLIPSE('',#31742,0.162242389830008,0.15) ;
#466 = ELLIPSE('',#31743,0.162242389830008,0.15) ;
#467 = ELLIPSE('',#31745,0.162242389830006,0.15) ;
#468 = ELLIPSE('',#31746,0.162242389830006,0.15) ;
#469 = ELLIPSE('',#31748,0.16224238983001,0.15) ;
#470 = ELLIPSE('',#31749,0.16224238983001,0.15) ;
#471 = ELLIPSE('',#31751,0.162242389830006,0.15) ;
#472 = ELLIPSE('',#31752,0.162242389830006,0.15) ;
#473 = ELLIPSE('',#31754,0.16224238983001,0.15) ;
#474 = ELLIPSE('',#31755,0.16224238983001,0.15) ;
#475 = ELLIPSE('',#31757,0.162242389830005,0.15) ;
#476 = ELLIPSE('',#31758,0.162242389830005,0.15) ;
#477 = ELLIPSE('',#31760,0.16224238983001,0.15) ;
#478 = ELLIPSE('',#31761,0.16224238983001,0.15) ;
#479 = ELLIPSE('',#31763,0.162242389830006,0.15) ;
#480 = ELLIPSE('',#31764,0.162242389830006,0.15) ;
#481 = ELLIPSE('',#31766,0.162242389830011,0.15) ;
#482 = ELLIPSE('',#31767,0.162242389830011,0.15) ;
#483 = ELLIPSE('',#31769,0.162242389830004,0.15) ;
#484 = ELLIPSE('',#31770,0.162242389830004,0.15) ;
#485 = ELLIPSE('',#31772,0.162242389830007,0.15) ;
#486 = ELLIPSE('',#31773,0.162242389830007,0.15) ;
#487 = ELLIPSE('',#31775,0.162242389830008,0.15) ;
#488 = ELLIPSE('',#31776,0.162242389830008,0.15) ;
#489 = ELLIPSE('',#31778,0.16224238983001,0.15) ;
#490 = ELLIPSE('',#31779,0.16224238983001,0.15) ;
#491 = ELLIPSE('',#31781,0.162242389830005,0.15) ;
#492 = ELLIPSE('',#31782,0.162242389830005,0.15) ;
#493 = ELLIPSE('',#31784,0.162242389830007,0.15) ;
#494 = ELLIPSE('',#31785,0.162242389830007,0.15) ;
#495 = ELLIPSE('',#31787,0.162242389830009,0.15) ;
#496 = ELLIPSE('',#31788,0.162242389830009,0.15) ;
#497 = ELLIPSE('',#31790,0.162242389830008,0.15) ;
#498 = ELLIPSE('',#31791,0.162242389830008,0.15) ;
#499 = ELLIPSE('',#31793,0.162242389830006,0.15) ;
#500 = ELLIPSE('',#31794,0.162242389830006,0.15) ;
#501 = ELLIPSE('',#31796,0.16224238983001,0.15) ;
#502 = ELLIPSE('',#31797,0.16224238983001,0.15) ;
#503 = ELLIPSE('',#31799,0.162242389830006,0.15) ;
#504 = ELLIPSE('',#31800,0.162242389830006,0.15) ;
#505 = ELLIPSE('',#31802,0.16224238983001,0.15) ;
#506 = ELLIPSE('',#31803,0.16224238983001,0.15) ;
#507 = ELLIPSE('',#31805,0.162242389830005,0.15) ;
#508 = ELLIPSE('',#31806,0.162242389830005,0.15) ;
#509 = ELLIPSE('',#31808,0.16224238983001,0.15) ;
#510 = ELLIPSE('',#31809,0.16224238983001,0.15) ;
#511 = ELLIPSE('',#31811,0.162242389830006,0.15) ;
#512 = ELLIPSE('',#31812,0.162242389830006,0.15) ;
#513 = ELLIPSE('',#31814,0.162242389830011,0.15) ;
#514 = ELLIPSE('',#31815,0.162242389830011,0.15) ;
#515 = ELLIPSE('',#31817,0.162242389830006,0.15) ;
#516 = ELLIPSE('',#31818,0.162242389830006,0.15) ;
#517 = ELLIPSE('',#31820,0.16224238983001,0.15) ;
#518 = ELLIPSE('',#31821,0.16224238983001,0.15) ;
#519 = ELLIPSE('',#31823,0.162242389830006,0.15) ;
#520 = ELLIPSE('',#31824,0.162242389830006,0.15) ;
#521 = ELLIPSE('',#31826,0.162242389830011,0.15) ;
#522 = ELLIPSE('',#31827,0.162242389830011,0.15) ;
#523 = ELLIPSE('',#31829,0.162242389830005,0.15) ;
#524 = ELLIPSE('',#31830,0.162242389830005,0.15) ;
#525 = ELLIPSE('',#31832,0.162242389830007,0.15) ;
#526 = ELLIPSE('',#31833,0.162242389830007,0.15) ;
#527 = ELLIPSE('',#31835,0.162242389830006,0.15) ;
#528 = ELLIPSE('',#31836,0.162242389830006,0.15) ;
#529 = ELLIPSE('',#31838,0.162242389830011,0.15) ;
#530 = ELLIPSE('',#31839,0.162242389830011,0.15) ;
#531 = ELLIPSE('',#31841,0.162242389830006,0.15) ;
#532 = ELLIPSE('',#31842,0.162242389830006,0.15) ;
#533 = ELLIPSE('',#31844,0.16224238983001,0.15) ;
#534 = ELLIPSE('',#31845,0.16224238983001,0.15) ;
#535 = ELLIPSE('',#31847,0.162242389830006,0.15) ;
#536 = ELLIPSE('',#31848,0.162242389830006,0.15) ;
#537 = ELLIPSE('',#31850,0.162242389830011,0.15) ;
#538 = ELLIPSE('',#31851,0.162242389830011,0.15) ;
#539 = ELLIPSE('',#31853,0.162242389830005,0.15) ;
#540 = ELLIPSE('',#31854,0.162242389830005,0.15) ;
#541 = ELLIPSE('',#31856,0.162242389830007,0.15) ;
#542 = ELLIPSE('',#31857,0.162242389830007,0.15) ;
#543 = ELLIPSE('',#31859,0.162242389830006,0.15) ;
#544 = ELLIPSE('',#31860,0.162242389830006,0.15) ;
#545 = ELLIPSE('',#31862,0.162242389830011,0.15) ;
#546 = ELLIPSE('',#31863,0.162242389830011,0.15) ;
#547 = ELLIPSE('',#31865,0.162242389830006,0.15) ;
#548 = ELLIPSE('',#31866,0.162242389830006,0.15) ;
#549 = ELLIPSE('',#31868,0.16224238983001,0.15) ;
#550 = ELLIPSE('',#31869,0.16224238983001,0.15) ;
#551 = ELLIPSE('',#31871,0.162242389830006,0.15) ;
#552 = ELLIPSE('',#31872,0.162242389830006,0.15) ;
#553 = ELLIPSE('',#31874,0.162242389830011,0.15) ;
#554 = ELLIPSE('',#31875,0.162242389830011,0.15) ;
#555 = ELLIPSE('',#31877,0.162242389830005,0.15) ;
#556 = ELLIPSE('',#31878,0.162242389830005,0.15) ;
#557 = ELLIPSE('',#31880,0.162242389830007,0.15) ;
#558 = ELLIPSE('',#31881,0.162242389830007,0.15) ;
#559 = ELLIPSE('',#31883,0.162242389830006,0.15) ;
#560 = ELLIPSE('',#31884,0.162242389830006,0.15) ;
#561 = ELLIPSE('',#31886,0.162242389830011,0.15) ;
#562 = ELLIPSE('',#31887,0.162242389830011,0.15) ;
#563 = ELLIPSE('',#31889,0.162242389830004,0.15) ;
#564 = ELLIPSE('',#31890,0.162242389830004,0.15) ;
#565 = ELLIPSE('',#31892,0.162242389830007,0.15) ;
#566 = ELLIPSE('',#31893,0.162242389830007,0.15) ;
#567 = ELLIPSE('',#31895,0.162242389830006,0.15) ;
#568 = ELLIPSE('',#31896,0.162242389830006,0.15) ;
#569 = ELLIPSE('',#31898,0.16224238983001,0.15) ;
#570 = ELLIPSE('',#31899,0.16224238983001,0.15) ;
#571 = ELLIPSE('',#31901,0.162242389830005,0.15) ;
#572 = ELLIPSE('',#31902,0.162242389830005,0.15) ;
#573 = ELLIPSE('',#31904,0.162242389830007,0.15) ;
#574 = ELLIPSE('',#31905,0.162242389830007,0.15) ;
#575 = ELLIPSE('',#31907,0.162242389830006,0.15) ;
#576 = ELLIPSE('',#31908,0.162242389830006,0.15) ;
#577 = ELLIPSE('',#31910,0.162242389830011,0.15) ;
#578 = ELLIPSE('',#31911,0.162242389830011,0.15) ;
#579 = ELLIPSE('',#31913,0.162242389830004,0.15) ;
#580 = ELLIPSE('',#31914,0.162242389830004,0.15) ;
#581 = ELLIPSE('',#31916,0.162242389830007,0.15) ;
#582 = ELLIPSE('',#31917,0.162242389830007,0.15) ;
#583 = ELLIPSE('',#31919,0.162242389830006,0.15) ;
#584 = ELLIPSE('',#31920,0.162242389830006,0.15) ;
#585 = ELLIPSE('',#31922,0.16224238983001,0.15) ;
#586 = ELLIPSE('',#31923,0.16224238983001,0.15) ;
#587 = ELLIPSE('',#31925,0.162242389830005,0.15) ;
#588 = ELLIPSE('',#31926,0.162242389830005,0.15) ;
#589 = ELLIPSE('',#31928,0.162242389830007,0.15) ;
#590 = ELLIPSE('',#31929,0.162242389830007,0.15) ;
#591 = ELLIPSE('',#31931,0.162242389830006,0.15) ;
#592 = ELLIPSE('',#31932,0.162242389830006,0.15) ;
#593 = ELLIPSE('',#31934,0.162242389830011,0.15) ;
#594 = ELLIPSE('',#31935,0.162242389830011,0.15) ;
#595 = ELLIPSE('',#31937,0.162242389830004,0.15) ;
#596 = ELLIPSE('',#31938,0.162242389830004,0.15) ;
#597 = ELLIPSE('',#31940,0.162242389830007,0.15) ;
#598 = ELLIPSE('',#31941,0.162242389830007,0.15) ;
#599 = ELLIPSE('',#31943,0.162242389830006,0.15) ;
#600 = ELLIPSE('',#31944,0.162242389830006,0.15) ;
#601 = ELLIPSE('',#31946,0.162242389830011,0.15) ;
#602 = ELLIPSE('',#31947,0.162242389830011,0.15) ;
#603 = ELLIPSE('',#31949,0.162242389830005,0.15) ;
#604 = ELLIPSE('',#31950,0.162242389830005,0.15) ;
#605 = ELLIPSE('',#31952,0.162242389830007,0.15) ;
#606 = ELLIPSE('',#31953,0.162242389830007,0.15) ;
#607 = ELLIPSE('',#31955,0.162242389830008,0.15) ;
#608 = ELLIPSE('',#31956,0.162242389830008,0.15) ;
#609 = ELLIPSE('',#31958,0.162242389830011,0.15) ;
#610 = ELLIPSE('',#31959,0.162242389830011,0.15) ;
#611 = ELLIPSE('',#31961,0.162242389830004,0.15) ;
#612 = ELLIPSE('',#31962,0.162242389830004,0.15) ;
#613 = ELLIPSE('',#31964,0.162242389830007,0.15) ;
#614 = ELLIPSE('',#31965,0.162242389830007,0.15) ;
#615 = ELLIPSE('',#31967,0.162242389830006,0.15) ;
#616 = ELLIPSE('',#31968,0.162242389830006,0.15) ;
#617 = ELLIPSE('',#31970,0.16224238983001,0.15) ;
#618 = ELLIPSE('',#31971,0.16224238983001,0.15) ;
#619 = ELLIPSE('',#31973,0.162242389830005,0.15) ;
#620 = ELLIPSE('',#31974,0.162242389830005,0.15) ;
#621 = ELLIPSE('',#31976,0.162242389830007,0.15) ;
#622 = ELLIPSE('',#31977,0.162242389830007,0.15) ;
#623 = ELLIPSE('',#31979,0.162242389830008,0.15) ;
#624 = ELLIPSE('',#31980,0.162242389830008,0.15) ;
#625 = ELLIPSE('',#31982,0.162242389830011,0.15) ;
#626 = ELLIPSE('',#31983,0.162242389830011,0.15) ;
#627 = ELLIPSE('',#31985,0.162242389830004,0.15) ;
#628 = ELLIPSE('',#31986,0.162242389830004,0.15) ;
#629 = ELLIPSE('',#31988,0.162242389830007,0.15) ;
#630 = ELLIPSE('',#31989,0.162242389830007,0.15) ;
#631 = ELLIPSE('',#31991,0.162242389830006,0.15) ;
#632 = ELLIPSE('',#31992,0.162242389830006,0.15) ;
#633 = ELLIPSE('',#31994,0.162242389830011,0.15) ;
#634 = ELLIPSE('',#31995,0.162242389830011,0.15) ;
#635 = ELLIPSE('',#31997,0.162242389830005,0.15) ;
#636 = ELLIPSE('',#31998,0.162242389830005,0.15) ;
#637 = ELLIPSE('',#32000,0.162242389830007,0.15) ;
#638 = ELLIPSE('',#32001,0.162242389830007,0.15) ;
#639 = ELLIPSE('',#32003,0.162242389830008,0.15) ;
#640 = ELLIPSE('',#32004,0.162242389830008,0.15) ;
#641 = ELLIPSE('',#32006,0.162242389830011,0.15) ;
#642 = ELLIPSE('',#32007,0.162242389830011,0.15) ;
#643 = ELLIPSE('',#32009,0.162242389830004,0.15) ;
#644 = ELLIPSE('',#32010,0.162242389830004,0.15) ;
#645 = ELLIPSE('',#32012,0.162242389830007,0.15) ;
#646 = ELLIPSE('',#32013,0.162242389830007,0.15) ;
#647 = ELLIPSE('',#32015,0.162242389830006,0.15) ;
#648 = ELLIPSE('',#32016,0.162242389830006,0.15) ;
#649 = ELLIPSE('',#32018,0.16224238983001,0.15) ;
#650 = ELLIPSE('',#32019,0.16224238983001,0.15) ;
#651 = ELLIPSE('',#32021,0.162242389830005,0.15) ;
#652 = ELLIPSE('',#32022,0.162242389830005,0.15) ;
#653 = ELLIPSE('',#32024,0.162242389830007,0.15) ;
#654 = ELLIPSE('',#32025,0.162242389830007,0.15) ;
#655 = ELLIPSE('',#32027,0.162242389830008,0.15) ;
#656 = ELLIPSE('',#32028,0.162242389830008,0.15) ;
#657 = ELLIPSE('',#32030,0.162242389830012,0.15) ;
#658 = ELLIPSE('',#32031,0.162242389830012,0.15) ;
#659 = ELLIPSE('',#32033,0.162242389830004,0.15) ;
#660 = ELLIPSE('',#32034,0.162242389830004,0.15) ;
#661 = ELLIPSE('',#32036,0.162242389830007,0.15) ;
#662 = ELLIPSE('',#32037,0.162242389830007,0.15) ;
#663 = ELLIPSE('',#32039,0.162242389830006,0.15) ;
#664 = ELLIPSE('',#32040,0.162242389830006,0.15) ;
#665 = ELLIPSE('',#32042,0.162242389830011,0.15) ;
#666 = ELLIPSE('',#32043,0.162242389830011,0.15) ;
#667 = ELLIPSE('',#32045,0.162242389830005,0.15) ;
#668 = ELLIPSE('',#32046,0.162242389830005,0.15) ;
#669 = ELLIPSE('',#32048,0.162242389830007,0.15) ;
#670 = ELLIPSE('',#32049,0.162242389830007,0.15) ;
#671 = ELLIPSE('',#32051,0.162242389830008,0.15) ;
#672 = ELLIPSE('',#32052,0.162242389830008,0.15) ;
#673 = ELLIPSE('',#32089,4.52782199571862,3.3) ;
#674 = ELLIPSE('',#32097,4.80223545000459,3.5) ;
#675 = ELLIPSE('',#32186,3.80741464119683,3.8) ;
#676 = ELLIPSE('',#32279,0.965925826289068,0.25) ;
#677 = ELLIPSE('',#32280,0.965925826289068,0.25) ;
#678 = ELLIPSE('',#32281,0.258819045102521,0.25) ;
#679 = ELLIPSE('',#32282,0.258819045102521,0.25) ;
#680 = ELLIPSE('',#32284,0.258819045102521,0.25) ;
#681 = ELLIPSE('',#32285,0.258819045102521,0.25) ;
#682 = ELLIPSE('',#32331,0.258819045102521,0.25) ;
#683 = ELLIPSE('',#32332,0.258819045102521,0.25) ;
#684 = ELLIPSE('',#32333,0.258819045102521,0.25) ;
#685 = ELLIPSE('',#32334,0.258819045102521,0.25) ;
#686 = ELLIPSE('',#32336,0.258819045102521,0.25) ;
#687 = ELLIPSE('',#32337,0.258819045102521,0.25) ;
#688 = ELLIPSE('',#32339,0.258819045102521,0.25) ;
#689 = ELLIPSE('',#32340,0.258819045102521,0.25) ;
#690 = ELLIPSE('',#32342,0.258819045102521,0.25) ;
#691 = ELLIPSE('',#32344,0.258819045102521,0.25) ;
#692 = ELLIPSE('',#32346,0.258819045102521,0.25) ;
#693 = ELLIPSE('',#32348,0.258819045102521,0.25) ;
#694 = ELLIPSE('',#32350,0.258819045102521,0.25) ;
#695 = ELLIPSE('',#32352,0.965925826289069,0.25) ;
#696 = ELLIPSE('',#32353,0.965925826289069,0.25) ;
#697 = ELLIPSE('',#32355,0.258819045102521,0.25) ;
#698 = ELLIPSE('',#32356,0.258819045102521,0.25) ;
#699 = SPHERICAL_SURFACE('',#29731,2.) ;
#700 = SPHERICAL_SURFACE('',#29734,2.) ;
#701 = SPHERICAL_SURFACE('',#29737,2.) ;
#702 = SPHERICAL_SURFACE('',#29740,2.) ;
#703 = SPHERICAL_SURFACE('',#29743,2.) ;
#704 = SPHERICAL_SURFACE('',#29746,2.) ;
#705 = SPHERICAL_SURFACE('',#29749,2.) ;
#706 = SPHERICAL_SURFACE('',#29752,2.) ;
#707 = SPHERICAL_SURFACE('',#29756,2.) ;
#708 = SPHERICAL_SURFACE('',#29761,2.) ;
#709 = SPHERICAL_SURFACE('',#29766,2.) ;
#710 = SPHERICAL_SURFACE('',#29771,2.) ;
#711 = SPHERICAL_SURFACE('',#29776,2.) ;
#712 = SPHERICAL_SURFACE('',#29781,2.) ;
#713 = SPHERICAL_SURFACE('',#29786,2.) ;
#714 = SPHERICAL_SURFACE('',#29791,2.) ;
#715 = SPHERICAL_SURFACE('',#29796,2.) ;
#716 = SPHERICAL_SURFACE('',#29801,2.) ;
#717 = SPHERICAL_SURFACE('',#29806,2.) ;
#718 = SPHERICAL_SURFACE('',#29811,2.) ;
#719 = SPHERICAL_SURFACE('',#29816,2.) ;
#720 = SPHERICAL_SURFACE('',#29821,2.) ;
#721 = SPHERICAL_SURFACE('',#29825,2.) ;
#722 = SPHERICAL_SURFACE('',#29828,2.) ;
#723 = SPHERICAL_SURFACE('',#29831,2.) ;
#724 = SPHERICAL_SURFACE('',#29834,2.) ;
#725 = SPHERICAL_SURFACE('',#29837,2.) ;
#726 = SPHERICAL_SURFACE('',#29840,2.) ;
#727 = SPHERICAL_SURFACE('',#30930,1.6) ;
#728 = SPHERICAL_SURFACE('',#30943,0.15) ;
#729 = SPHERICAL_SURFACE('',#30945,0.15) ;
#730 = SPHERICAL_SURFACE('',#30947,0.15) ;
#731 = SPHERICAL_SURFACE('',#30949,0.4) ;
#732 = SPHERICAL_SURFACE('',#30953,0.4) ;
#733 = SPHERICAL_SURFACE('',#30954,0.4) ;
#734 = SPHERICAL_SURFACE('',#30957,0.4) ;
#735 = SPHERICAL_SURFACE('',#30962,0.4) ;
#736 = SPHERICAL_SURFACE('',#30965,0.4) ;
#737 = SPHERICAL_SURFACE('',#30998,0.4) ;
#738 = SPHERICAL_SURFACE('',#30999,0.4) ;
#739 = SPHERICAL_SURFACE('',#31000,0.4) ;
#740 = SPHERICAL_SURFACE('',#31001,0.4) ;
#741 = SPHERICAL_SURFACE('',#31003,0.4) ;
#742 = SPHERICAL_SURFACE('',#31009,0.15) ;
#743 = SPHERICAL_SURFACE('',#31011,0.4) ;
#744 = SPHERICAL_SURFACE('',#31021,0.4) ;
#745 = SPHERICAL_SURFACE('',#31022,0.4) ;
#746 = SPHERICAL_SURFACE('',#31033,0.4) ;
#747 = SPHERICAL_SURFACE('',#31034,0.15) ;
#748 = SPHERICAL_SURFACE('',#31105,0.15) ;
#749 = SPHERICAL_SURFACE('',#31108,0.15) ;
#750 = SPHERICAL_SURFACE('',#31112,0.15) ;
#751 = SPHERICAL_SURFACE('',#31116,0.15) ;
#752 = SPHERICAL_SURFACE('',#31122,0.15) ;
#753 = SPHERICAL_SURFACE('',#31126,0.15) ;
#754 = SPHERICAL_SURFACE('',#31130,0.15) ;
#755 = SPHERICAL_SURFACE('',#31134,0.15) ;
#756 = SPHERICAL_SURFACE('',#31140,0.15) ;
#757 = SPHERICAL_SURFACE('',#31144,0.15) ;
#758 = SPHERICAL_SURFACE('',#31148,0.15) ;
#759 = SPHERICAL_SURFACE('',#31152,0.15) ;
#760 = SPHERICAL_SURFACE('',#31158,0.15) ;
#761 = SPHERICAL_SURFACE('',#31162,0.15) ;
#762 = SPHERICAL_SURFACE('',#31166,0.15) ;
#763 = SPHERICAL_SURFACE('',#31170,0.15) ;
#764 = SPHERICAL_SURFACE('',#31176,0.15) ;
#765 = SPHERICAL_SURFACE('',#31180,0.15) ;
#766 = SPHERICAL_SURFACE('',#31184,0.15) ;
#767 = SPHERICAL_SURFACE('',#31188,0.15) ;
#768 = SPHERICAL_SURFACE('',#31194,0.15) ;
#769 = SPHERICAL_SURFACE('',#31198,0.15) ;
#770 = SPHERICAL_SURFACE('',#31202,0.15) ;
#771 = SPHERICAL_SURFACE('',#31206,0.15) ;
#772 = SPHERICAL_SURFACE('',#31212,0.15) ;
#773 = SPHERICAL_SURFACE('',#31216,0.15) ;
#774 = SPHERICAL_SURFACE('',#31220,0.15) ;
#775 = SPHERICAL_SURFACE('',#31224,0.15) ;
#776 = SPHERICAL_SURFACE('',#31230,0.15) ;
#777 = SPHERICAL_SURFACE('',#31234,0.15) ;
#778 = SPHERICAL_SURFACE('',#31238,0.15) ;
#779 = SPHERICAL_SURFACE('',#31242,0.15) ;
#780 = SPHERICAL_SURFACE('',#31248,0.15) ;
#781 = SPHERICAL_SURFACE('',#31252,0.15) ;
#782 = SPHERICAL_SURFACE('',#31256,0.15) ;
#783 = SPHERICAL_SURFACE('',#31260,0.15) ;
#784 = SPHERICAL_SURFACE('',#31266,0.15) ;
#785 = SPHERICAL_SURFACE('',#31270,0.15) ;
#786 = SPHERICAL_SURFACE('',#31274,0.15) ;
#787 = SPHERICAL_SURFACE('',#31278,0.15) ;
#788 = SPHERICAL_SURFACE('',#31284,0.15) ;
#789 = SPHERICAL_SURFACE('',#31288,0.15) ;
#790 = SPHERICAL_SURFACE('',#31292,0.15) ;
#791 = SPHERICAL_SURFACE('',#31296,0.15) ;
#792 = SPHERICAL_SURFACE('',#31302,0.15) ;
#793 = SPHERICAL_SURFACE('',#31306,0.15) ;
#794 = SPHERICAL_SURFACE('',#31310,0.15) ;
#795 = SPHERICAL_SURFACE('',#31314,0.15) ;
#796 = SPHERICAL_SURFACE('',#31320,0.15) ;
#797 = SPHERICAL_SURFACE('',#31324,0.15) ;
#798 = SPHERICAL_SURFACE('',#31328,0.15) ;
#799 = SPHERICAL_SURFACE('',#31332,0.15) ;
#800 = SPHERICAL_SURFACE('',#31338,0.15) ;
#801 = SPHERICAL_SURFACE('',#31342,0.15) ;
#802 = SPHERICAL_SURFACE('',#31346,0.15) ;
#803 = SPHERICAL_SURFACE('',#31350,0.15) ;
#804 = SPHERICAL_SURFACE('',#31356,0.15) ;
#805 = SPHERICAL_SURFACE('',#31360,0.15) ;
#806 = SPHERICAL_SURFACE('',#31364,0.15) ;
#807 = SPHERICAL_SURFACE('',#31368,0.15) ;
#808 = SPHERICAL_SURFACE('',#31374,0.15) ;
#809 = SPHERICAL_SURFACE('',#31378,0.15) ;
#810 = SPHERICAL_SURFACE('',#31382,0.15) ;
#811 = SPHERICAL_SURFACE('',#31386,0.15) ;
#812 = SPHERICAL_SURFACE('',#31392,0.15) ;
#813 = SPHERICAL_SURFACE('',#31396,0.15) ;
#814 = SPHERICAL_SURFACE('',#31400,0.15) ;
#815 = SPHERICAL_SURFACE('',#31404,0.15) ;
#816 = SPHERICAL_SURFACE('',#31410,0.15) ;
#817 = SPHERICAL_SURFACE('',#31414,0.15) ;
#818 = SPHERICAL_SURFACE('',#31418,0.15) ;
#819 = SPHERICAL_SURFACE('',#31422,0.15) ;
#820 = SPHERICAL_SURFACE('',#31428,0.15) ;
#821 = SPHERICAL_SURFACE('',#31432,0.15) ;
#822 = SPHERICAL_SURFACE('',#31436,0.15) ;
#823 = SPHERICAL_SURFACE('',#31440,0.15) ;
#824 = SPHERICAL_SURFACE('',#31446,0.15) ;
#825 = SPHERICAL_SURFACE('',#31450,0.15) ;
#826 = SPHERICAL_SURFACE('',#31454,0.15) ;
#827 = SPHERICAL_SURFACE('',#31458,0.15) ;
#828 = SPHERICAL_SURFACE('',#31464,0.15) ;
#829 = SPHERICAL_SURFACE('',#31468,0.15) ;
#830 = SPHERICAL_SURFACE('',#31472,0.15) ;
#831 = SPHERICAL_SURFACE('',#31476,0.15) ;
#832 = SPHERICAL_SURFACE('',#31482,0.15) ;
#833 = SPHERICAL_SURFACE('',#31486,0.15) ;
#834 = SPHERICAL_SURFACE('',#31490,0.15) ;
#835 = SPHERICAL_SURFACE('',#31494,0.15) ;
#836 = SPHERICAL_SURFACE('',#31500,0.15) ;
#837 = SPHERICAL_SURFACE('',#31504,0.15) ;
#838 = SPHERICAL_SURFACE('',#31508,0.15) ;
#839 = SPHERICAL_SURFACE('',#31512,0.15) ;
#840 = SPHERICAL_SURFACE('',#31518,0.15) ;
#841 = SPHERICAL_SURFACE('',#31522,0.15) ;
#842 = SPHERICAL_SURFACE('',#31526,0.15) ;
#843 = SPHERICAL_SURFACE('',#31530,0.15) ;
#844 = SPHERICAL_SURFACE('',#31536,0.15) ;
#845 = SPHERICAL_SURFACE('',#31540,0.15) ;
#846 = SPHERICAL_SURFACE('',#31544,0.15) ;
#847 = SPHERICAL_SURFACE('',#31548,0.15) ;
#848 = SPHERICAL_SURFACE('',#31554,0.15) ;
#849 = SPHERICAL_SURFACE('',#31558,0.15) ;
#850 = SPHERICAL_SURFACE('',#31562,0.15) ;
#851 = SPHERICAL_SURFACE('',#31566,0.15) ;
#852 = SPHERICAL_SURFACE('',#31572,0.15) ;
#853 = SPHERICAL_SURFACE('',#31576,0.15) ;
#854 = SPHERICAL_SURFACE('',#31580,0.15) ;
#855 = SPHERICAL_SURFACE('',#31584,0.15) ;
#856 = SPHERICAL_SURFACE('',#31590,0.15) ;
#857 = SPHERICAL_SURFACE('',#31594,0.15) ;
#858 = SPHERICAL_SURFACE('',#31598,0.15) ;
#859 = SPHERICAL_SURFACE('',#31602,0.15) ;
#860 = SPHERICAL_SURFACE('',#31608,0.15) ;
#861 = SPHERICAL_SURFACE('',#31612,0.15) ;
#862 = SPHERICAL_SURFACE('',#31616,0.15) ;
#863 = SPHERICAL_SURFACE('',#31620,0.15) ;
#864 = SPHERICAL_SURFACE('',#31626,0.15) ;
#865 = SPHERICAL_SURFACE('',#31630,0.15) ;
#866 = SPHERICAL_SURFACE('',#31634,0.15) ;
#867 = SPHERICAL_SURFACE('',#31638,0.15) ;
#868 = SPHERICAL_SURFACE('',#31644,0.15) ;
#869 = SPHERICAL_SURFACE('',#31648,0.15) ;
#870 = SPHERICAL_SURFACE('',#31652,0.15) ;
#871 = SPHERICAL_SURFACE('',#31656,0.15) ;
#872 = SPHERICAL_SURFACE('',#31662,0.15) ;
#873 = SPHERICAL_SURFACE('',#31666,0.15) ;
#874 = SPHERICAL_SURFACE('',#31670,0.15) ;
#875 = SPHERICAL_SURFACE('',#32083,3.3) ;
#876 = SPHERICAL_SURFACE('',#32085,3.5) ;
#877 = SPHERICAL_SURFACE('',#32114,3.5) ;
#878 = SPHERICAL_SURFACE('',#32115,3.5) ;
#879 = SPHERICAL_SURFACE('',#32116,3.5) ;
#880 = SPHERICAL_SURFACE('',#32286,0.25) ;
#881 = SPHERICAL_SURFACE('',#32289,0.25) ;
#882 = SPHERICAL_SURFACE('',#32292,0.25) ;
#883 = SPHERICAL_SURFACE('',#32295,0.25) ;
#884 = SPHERICAL_SURFACE('',#32300,0.25) ;
#885 = SPHERICAL_SURFACE('',#32305,0.25) ;
#886 = SPHERICAL_SURFACE('',#32310,0.25) ;
#887 = SPHERICAL_SURFACE('',#32315,0.25) ;
#888 = SPHERICAL_SURFACE('',#32320,0.25) ;
#889 = SPHERICAL_SURFACE('',#32325,0.25) ;
#890 = SPHERICAL_SURFACE('',#32327,0.25) ;
#891 = SHAPE_REPRESENTATION_RELATIONSHIP('SRR','None',#50621,#936) ;
#892 = SHAPE_REPRESENTATION_RELATIONSHIP('SRR','None',#50622,#937) ;
#893 = SHAPE_REPRESENTATION_RELATIONSHIP('SRR','None',#50623,#938) ;
#894 = SHAPE_REPRESENTATION_RELATIONSHIP('SRR','None',#50624,#939) ;
#895 = SHAPE_REPRESENTATION_RELATIONSHIP('SRR','None',#50625,#940) ;
#896 = SHAPE_REPRESENTATION_RELATIONSHIP('SRR','None',#50627,#941) ;
#897 = SHAPE_REPRESENTATION_RELATIONSHIP('SRR','None',#50628,#942) ;
#898 = SHAPE_REPRESENTATION_RELATIONSHIP('SRR','None',#50629,#943) ;
#899 = SHAPE_REPRESENTATION_RELATIONSHIP('SRR','None',#50630,#944) ;
#900 = SHAPE_REPRESENTATION_RELATIONSHIP('SRR','None',#50632,#945) ;
#901 = SHAPE_REPRESENTATION_RELATIONSHIP('SRR','None',#50633,#946) ;
#902 = SHAPE_REPRESENTATION_RELATIONSHIP('SRR','None',#50634,#947) ;
#903 = SHAPE_REPRESENTATION_RELATIONSHIP('SRR','None',#50635,#948) ;
#904 = SHAPE_REPRESENTATION_RELATIONSHIP('SRR','None',#50636,#949) ;
#905 = SHAPE_REPRESENTATION_RELATIONSHIP('SRR','None',#50637,#950) ;
#906 = SHAPE_REPRESENTATION_RELATIONSHIP('SRR','None',#50638,#951) ;
#907 = SHAPE_REPRESENTATION_RELATIONSHIP('SRR','None',#50639,#952) ;
#908 = SHAPE_REPRESENTATION_RELATIONSHIP('SRR','None',#50640,#953) ;
#909 = SHAPE_REPRESENTATION_RELATIONSHIP('SRR','None',#50641,#954) ;
#910 = SHAPE_REPRESENTATION_RELATIONSHIP('SRR','None',#50643,#955) ;
#911 = SHAPE_REPRESENTATION_RELATIONSHIP('SRR','None',#50644,#956) ;
#912 = SHAPE_REPRESENTATION_RELATIONSHIP('SRR','None',#50645,#957) ;
#913 = SHAPE_REPRESENTATION_RELATIONSHIP('SRR','None',#50646,#958) ;
#914 = SHAPE_REPRESENTATION_RELATIONSHIP('SRR','None',#50647,#959) ;
#915 = SHAPE_REPRESENTATION_RELATIONSHIP('SRR','None',#50648,#960) ;
#916 = SHAPE_REPRESENTATION_RELATIONSHIP('SRR','None',#50649,#961) ;
#917 = SHAPE_REPRESENTATION_RELATIONSHIP('SRR','None',#50650,#962) ;
#918 = SHAPE_REPRESENTATION_RELATIONSHIP('SRR','None',#50651,#963) ;
#919 = SHAPE_REPRESENTATION_RELATIONSHIP('SRR','None',#50652,#964) ;
#920 = SHAPE_REPRESENTATION_RELATIONSHIP('SRR','None',#50653,#965) ;
#921 = SHAPE_REPRESENTATION_RELATIONSHIP('SRR','None',#50654,#966) ;
#922 = SHAPE_REPRESENTATION_RELATIONSHIP('SRR','None',#50655,#967) ;
#923 = SHAPE_REPRESENTATION_RELATIONSHIP('SRR','None',#50656,#968) ;
#924 = SHAPE_REPRESENTATION_RELATIONSHIP('SRR','None',#50658,#969) ;
#925 = SHAPE_REPRESENTATION_RELATIONSHIP('SRR','None',#50659,#970) ;
#926 = SHAPE_REPRESENTATION_RELATIONSHIP('SRR','None',#50660,#971) ;
#927 = SHAPE_REPRESENTATION_RELATIONSHIP('SRR','None',#50661,#972) ;
#928 = SHAPE_REPRESENTATION_RELATIONSHIP('SRR','None',#50662,#973) ;
#929 = SHAPE_REPRESENTATION_RELATIONSHIP('SRR','None',#50664,#974) ;
#930 = SHAPE_REPRESENTATION_RELATIONSHIP('SRR','None',#50665,#975) ;
#931 = SHAPE_REPRESENTATION_RELATIONSHIP('SRR','None',#50666,#976) ;
#932 = SHAPE_REPRESENTATION_RELATIONSHIP('SRR','None',#50667,#977) ;
#933 = SHAPE_REPRESENTATION_RELATIONSHIP('SRR','None',#50668,#978) ;
#934 = SHAPE_REPRESENTATION_RELATIONSHIP('SRR','None',#50669,#979) ;
#935 = SHAPE_REPRESENTATION_RELATIONSHIP('SRR','None',#50670,#980) ;
#936 = ADVANCED_BREP_SHAPE_REPRESENTATION('',(#1037),#50390) ;
#937 = ADVANCED_BREP_SHAPE_REPRESENTATION('',(#1038),#50391) ;
#938 = ADVANCED_BREP_SHAPE_REPRESENTATION('',(#1039),#50392) ;
#939 = ADVANCED_BREP_SHAPE_REPRESENTATION('',(#1040),#50393) ;
#940 = ADVANCED_BREP_SHAPE_REPRESENTATION('',(#1041),#50394) ;
#941 = ADVANCED_BREP_SHAPE_REPRESENTATION('',(#79),#50396) ;
#942 = ADVANCED_BREP_SHAPE_REPRESENTATION('',(#1042),#50397) ;
#943 = ADVANCED_BREP_SHAPE_REPRESENTATION('',(#1043),#50398) ;
#944 = ADVANCED_BREP_SHAPE_REPRESENTATION('',(#1044),#50399) ;
#945 = ADVANCED_BREP_SHAPE_REPRESENTATION('',(#1045),#50401) ;
#946 = ADVANCED_BREP_SHAPE_REPRESENTATION('',(#1046),#50402) ;
#947 = ADVANCED_BREP_SHAPE_REPRESENTATION('',(#1047),#50403) ;
#948 = ADVANCED_BREP_SHAPE_REPRESENTATION('',(#1048),#50404) ;
#949 = ADVANCED_BREP_SHAPE_REPRESENTATION('',(#1049),#50405) ;
#950 = ADVANCED_BREP_SHAPE_REPRESENTATION('',(#1050),#50406) ;
#951 = ADVANCED_BREP_SHAPE_REPRESENTATION('',(#1051),#50407) ;
#952 = ADVANCED_BREP_SHAPE_REPRESENTATION('',(#1052,#1053,#1054),#50408) ;
#953 = ADVANCED_BREP_SHAPE_REPRESENTATION('',(#1055),#50409) ;
#954 = ADVANCED_BREP_SHAPE_REPRESENTATION('',(#1056),#50410) ;
#955 = ADVANCED_BREP_SHAPE_REPRESENTATION('',(#1057),#50412) ;
#956 = ADVANCED_BREP_SHAPE_REPRESENTATION('',(#1058),#50413) ;
#957 = ADVANCED_BREP_SHAPE_REPRESENTATION('',(#1059),#50414) ;
#958 = ADVANCED_BREP_SHAPE_REPRESENTATION('',(#1060),#50415) ;
#959 = ADVANCED_BREP_SHAPE_REPRESENTATION('',(#1061,#1062),#50416) ;
#960 = ADVANCED_BREP_SHAPE_REPRESENTATION('',(#1063),#50417) ;
#961 = ADVANCED_BREP_SHAPE_REPRESENTATION('',(#1064),#50418) ;
#962 = ADVANCED_BREP_SHAPE_REPRESENTATION('',(#1065),#50419) ;
#963 = ADVANCED_BREP_SHAPE_REPRESENTATION('',(#1066),#50420) ;
#964 = ADVANCED_BREP_SHAPE_REPRESENTATION('',(#80),#50421) ;
#965 = ADVANCED_BREP_SHAPE_REPRESENTATION('',(#1067,#1068),#50422) ;
#966 = ADVANCED_BREP_SHAPE_REPRESENTATION('',(#1069),#50423) ;
#967 = ADVANCED_BREP_SHAPE_REPRESENTATION('',(#1070),#50424) ;
#968 = ADVANCED_BREP_SHAPE_REPRESENTATION('',(#1071,#1072,#1073,#1074),#50425) ;
#969 = ADVANCED_BREP_SHAPE_REPRESENTATION('',(#81),#50427) ;
#970 = ADVANCED_BREP_SHAPE_REPRESENTATION('',(#1075,#1076,#1077,#1078),#50428) ;
#971 = ADVANCED_BREP_SHAPE_REPRESENTATION('',(#1079),#50429) ;
#972 = ADVANCED_BREP_SHAPE_REPRESENTATION('',(#1080,#1081),#50430) ;
#973 = ADVANCED_BREP_SHAPE_REPRESENTATION('',(#1082),#50431) ;
#974 = ADVANCED_BREP_SHAPE_REPRESENTATION('',(#1083),#50433) ;
#975 = ADVANCED_BREP_SHAPE_REPRESENTATION('',(#1084),#50434) ;
#976 = ADVANCED_BREP_SHAPE_REPRESENTATION('',(#1085),#50435) ;
#977 = ADVANCED_BREP_SHAPE_REPRESENTATION('',(#1086),#50436) ;
#978 = ADVANCED_BREP_SHAPE_REPRESENTATION('',(#1087),#50437) ;
#979 = ADVANCED_BREP_SHAPE_REPRESENTATION('',(#1088),#50438) ;
#980 = ADVANCED_BREP_SHAPE_REPRESENTATION('',(#1089),#50439) ;
#981 = STYLED_ITEM('',(#50884),#1037) ;
#982 = STYLED_ITEM('',(#50884),#1038) ;
#983 = STYLED_ITEM('',(#50885),#1039) ;
#984 = STYLED_ITEM('',(#50885),#1040) ;
#985 = STYLED_ITEM('',(#50883),#1041) ;
#986 = STYLED_ITEM('',(#50883),#79) ;
#987 = STYLED_ITEM('',(#50883),#1042) ;
#988 = STYLED_ITEM('',(#50883),#1043) ;
#989 = STYLED_ITEM('',(#50883),#1044) ;
#990 = STYLED_ITEM('',(#50886),#1045) ;
#991 = STYLED_ITEM('',(#50887),#1046) ;
#992 = STYLED_ITEM('',(#50883),#1047) ;
#993 = STYLED_ITEM('',(#50888),#1048) ;
#994 = STYLED_ITEM('',(#50884),#1049) ;
#995 = STYLED_ITEM('',(#50883),#1050) ;
#996 = STYLED_ITEM('',(#50883),#1051) ;
#997 = STYLED_ITEM('',(#50883),#1052) ;
#998 = STYLED_ITEM('',(#50883),#1053) ;
#999 = STYLED_ITEM('',(#50883),#1054) ;
#1000 = STYLED_ITEM('',(#50889),#1055) ;
#1001 = STYLED_ITEM('',(#50888),#1056) ;
#1002 = STYLED_ITEM('',(#50885),#1057) ;
#1003 = STYLED_ITEM('',(#50889),#1058) ;
#1004 = STYLED_ITEM('',(#50886),#1059) ;
#1005 = STYLED_ITEM('',(#50889),#1060) ;
#1006 = STYLED_ITEM('',(#50889),#1061) ;
#1007 = STYLED_ITEM('',(#50889),#1062) ;
#1008 = STYLED_ITEM('',(#50883),#1063) ;
#1009 = STYLED_ITEM('',(#50883),#1064) ;
#1010 = STYLED_ITEM('',(#50888),#1065) ;
#1011 = STYLED_ITEM('',(#50883),#1066) ;
#1012 = STYLED_ITEM('',(#50888),#80) ;
#1013 = STYLED_ITEM('',(#50883),#1067) ;
#1014 = STYLED_ITEM('',(#50883),#1068) ;
#1015 = STYLED_ITEM('',(#50887),#1069) ;
#1016 = STYLED_ITEM('',(#50887),#1070) ;
#1017 = STYLED_ITEM('',(#50883),#1071) ;
#1018 = STYLED_ITEM('',(#50883),#1072) ;
#1019 = STYLED_ITEM('',(#50883),#1073) ;
#1020 = STYLED_ITEM('',(#50883),#1074) ;
#1021 = STYLED_ITEM('',(#50889),#81) ;
#1022 = STYLED_ITEM('',(#50883),#1075) ;
#1023 = STYLED_ITEM('',(#50883),#1076) ;
#1024 = STYLED_ITEM('',(#50883),#1077) ;
#1025 = STYLED_ITEM('',(#50883),#1078) ;
#1026 = STYLED_ITEM('',(#50887),#1079) ;
#1027 = STYLED_ITEM('',(#50889),#1080) ;
#1028 = STYLED_ITEM('',(#50889),#1081) ;
#1029 = STYLED_ITEM('',(#50889),#1082) ;
#1030 = STYLED_ITEM('',(#50883),#1083) ;
#1031 = STYLED_ITEM('',(#50883),#1084) ;
#1032 = STYLED_ITEM('',(#50883),#1085) ;
#1033 = STYLED_ITEM('',(#50883),#1086) ;
#1034 = STYLED_ITEM('',(#50883),#1087) ;
#1035 = STYLED_ITEM('',(#50883),#1088) ;
#1036 = STYLED_ITEM('',(#50883),#1089) ;
#1037 = MANIFOLD_SOLID_BREP('CONICAL_POLYETHYLENE_HOPPER',#28629) ;
#1038 = MANIFOLD_SOLID_BREP('HOPPER_LID',#28630) ;
#1039 = MANIFOLD_SOLID_BREP('LID_HINGE_STRAP',#28631) ;
#1040 = MANIFOLD_SOLID_BREP('HOPPER_SIEVE_GRID',#28632) ;
#1041 = MANIFOLD_SOLID_BREP('HOPPER_SUPPORT_RING',#28633) ;
#1042 = MANIFOLD_SOLID_BREP('STAND_FOOT_PLATE',#28654) ;
#1043 = MANIFOLD_SOLID_BREP('LOWER_LINK_PIN_CAT2',#28655) ;
#1044 = MANIFOLD_SOLID_BREP('TOP_LINK_PIN_CAT2',#28656) ;
#1045 = MANIFOLD_SOLID_BREP('GEARBOX_OSCILLATION_HOUSING',#28657) ;
#1046 = MANIFOLD_SOLID_BREP('GEARBOX_OIL_PLUG',#28658) ;
#1047 = MANIFOLD_SOLID_BREP('PTO_INPUT_SHAFT_SPLINE',#28659) ;
#1048 = MANIFOLD_SOLID_BREP('PTO_SHAFT_SEAL',#28660) ;
#1049 = MANIFOLD_SOLID_BREP('PTO_SHIELD_GUARD',#28661) ;
#1050 = MANIFOLD_SOLID_BREP('OSCILLATION_OUTPUT_SHAFT',#28662) ;
#1051 = MANIFOLD_SOLID_BREP('OSCILLATION_CRANK_DISC',#28663) ;
#1052 = MANIFOLD_SOLID_BREP('CONNECTING_ROD',#28664) ;
#1053 = MANIFOLD_SOLID_BREP('CONNECTING_ROD',#28665) ;
#1054 = MANIFOLD_SOLID_BREP('CONNECTING_ROD',#28666) ;
#1055 = MANIFOLD_SOLID_BREP('AGITATOR_SHAFT_ASSEMBLY',#28667) ;
#1056 = MANIFOLD_SOLID_BREP('AGITATOR_SHAFT_SEAL',#28668) ;
#1057 = MANIFOLD_SOLID_BREP('GATE_HOUSING_PLATE',#28669) ;
#1058 = MANIFOLD_SOLID_BREP('METERING_GATE_ORIFICE_PLATE',#28670) ;
#1059 = MANIFOLD_SOLID_BREP('FLOW_RATE_SCALE_STRIP',#28671) ;
#1060 = MANIFOLD_SOLID_BREP('OUTLET_FUNNEL',#28672) ;
#1061 = MANIFOLD_SOLID_BREP('SPOUT_FEED_FUNNEL',#28673) ;
#1062 = MANIFOLD_SOLID_BREP('SPOUT_FEED_FUNNEL',#28674) ;
#1063 = MANIFOLD_SOLID_BREP('FLOW_CONTROL_QUADRANT',#28675) ;
#1064 = MANIFOLD_SOLID_BREP('CABLE_ACTUATED_FLOW_CONTROL_LEVER',#28676) ;
#1065 = MANIFOLD_SOLID_BREP('LEVER_KNOB',#28677) ;
#1066 = MANIFOLD_SOLID_BREP('LEVER_PIVOT_PIN',#28678) ;
#1067 = MANIFOLD_SOLID_BREP('CONTROL_CABLE_INNER_WIRE',#28689) ;
#1068 = MANIFOLD_SOLID_BREP('CONTROL_CABLE_INNER_WIRE',#28690) ;
#1069 = MANIFOLD_SOLID_BREP('CABLE_END_NIPPLE',#28691) ;
#1070 = MANIFOLD_SOLID_BREP('LEVER_END_NIPPLE',#28692) ;
#1071 = MANIFOLD_SOLID_BREP('RETURN_TENSION_SPRING_ASSEMBLY',#28693) ;
#1072 = MANIFOLD_SOLID_BREP('RETURN_TENSION_SPRING_ASSEMBLY',#28694) ;
#1073 = MANIFOLD_SOLID_BREP('RETURN_TENSION_SPRING_ASSEMBLY',#28695) ;
#1074 = MANIFOLD_SOLID_BREP('RETURN_TENSION_SPRING_ASSEMBLY',#28696) ;
#1075 = MANIFOLD_SOLID_BREP('PENDULUM_TRUNNION_YOKE',#28700) ;
#1076 = MANIFOLD_SOLID_BREP('PENDULUM_TRUNNION_YOKE',#28701) ;
#1077 = MANIFOLD_SOLID_BREP('PENDULUM_TRUNNION_YOKE',#28702) ;
#1078 = MANIFOLD_SOLID_BREP('PENDULUM_TRUNNION_YOKE',#28703) ;
#1079 = MANIFOLD_SOLID_BREP('TRUNNION_BUSHING',#28704) ;
#1080 = MANIFOLD_SOLID_BREP('SPOUT_DEFLECTOR_PLATE',#28705) ;
#1081 = MANIFOLD_SOLID_BREP('SPOUT_DEFLECTOR_PLATE',#28706) ;
#1082 = MANIFOLD_SOLID_BREP('SPOUT_CLAMP_BAND',#28707) ;
#1083 = MANIFOLD_SOLID_BREP('GEARBOX_MOUNT_BOLT_M12x65',#28708) ;
#1084 = MANIFOLD_SOLID_BREP('GEARBOX_MOUNT_NUT_M12',#28709) ;
#1085 = MANIFOLD_SOLID_BREP('GATE_HOUSING_BOLT_M8x30',#28710) ;
#1086 = MANIFOLD_SOLID_BREP('LEVER_PIVOT_NUT_M10',#28711) ;
#1087 = MANIFOLD_SOLID_BREP('SPRING_HOOK_PIN',#28712) ;
#1088 = MANIFOLD_SOLID_BREP('SPRING_ANCHOR_PIN',#28713) ;
#1089 = MANIFOLD_SOLID_BREP('LINCH_PIN',#28714) ;
#1090 = CONICAL_SURFACE('',#29307,32.15,0.600917014687121) ;
#1091 = CONICAL_SURFACE('',#29309,32.75,0.600917014687121) ;
#1092 = CONICAL_SURFACE('',#30829,9.,0.805803494083987) ;
#1093 = CONICAL_SURFACE('',#30838,8.7,0.805803494083986) ;
#1094 = CONICAL_SURFACE('',#30858,4.65,0.193959147259893) ;
#1095 = CONICAL_SURFACE('',#30859,4.45,0.193959147259893) ;
#1096 = (
BOUNDED_CURVE()
B_SPLINE_CURVE(2,(#41351,#41352,#41353),.UNSPECIFIED.,.F.,.F.)
B_SPLINE_CURVE_WITH_KNOTS((3,3),(0.,1.45668740131038),.UNSPECIFIED.)
CURVE()
GEOMETRIC_REPRESENTATION_ITEM()
RATIONAL_B_SPLINE_CURVE((1.,1.00010597947028,1.))
REPRESENTATION_ITEM('')
) ;
#1097 = (
BOUNDED_CURVE()
B_SPLINE_CURVE(2,(#41359,#41360,#41361),.UNSPECIFIED.,.F.,.F.)
B_SPLINE_CURVE_WITH_KNOTS((3,3),(0.,1.45668740131038),.UNSPECIFIED.)
CURVE()
GEOMETRIC_REPRESENTATION_ITEM()
RATIONAL_B_SPLINE_CURVE((1.,1.00010597945705,1.))
REPRESENTATION_ITEM('')
) ;
#1098 = (
BOUNDED_CURVE()
B_SPLINE_CURVE(2,(#41368,#41369,#41370),.UNSPECIFIED.,.F.,.F.)
B_SPLINE_CURVE_WITH_KNOTS((3,3),(0.,1.45676753689758),.UNSPECIFIED.)
CURVE()
GEOMETRIC_REPRESENTATION_ITEM()
RATIONAL_B_SPLINE_CURVE((1.,1.00011064855622,1.))
REPRESENTATION_ITEM('')
) ;
#1099 = (
BOUNDED_CURVE()
B_SPLINE_CURVE(2,(#41392,#41393,#41394),.UNSPECIFIED.,.F.,.F.)
B_SPLINE_CURVE_WITH_KNOTS((3,3),(0.,1.45676753689757),.UNSPECIFIED.)
CURVE()
GEOMETRIC_REPRESENTATION_ITEM()
RATIONAL_B_SPLINE_CURVE((1.,1.00011064897844,1.))
REPRESENTATION_ITEM('')
) ;
#1100 = (
BOUNDED_CURVE()
B_SPLINE_CURVE(2,(#41409,#41410,#41411),.UNSPECIFIED.,.F.,.F.)
B_SPLINE_CURVE_WITH_KNOTS((3,3),(0.,1.45668740131038),.UNSPECIFIED.)
CURVE()
GEOMETRIC_REPRESENTATION_ITEM()
RATIONAL_B_SPLINE_CURVE((1.,1.00010597929787,1.))
REPRESENTATION_ITEM('')
) ;
#1101 = (
BOUNDED_CURVE()
B_SPLINE_CURVE(2,(#41417,#41418,#41419),.UNSPECIFIED.,.F.,.F.)
B_SPLINE_CURVE_WITH_KNOTS((3,3),(0.,1.45668740131038),.UNSPECIFIED.)
CURVE()
GEOMETRIC_REPRESENTATION_ITEM()
RATIONAL_B_SPLINE_CURVE((1.,1.00010597985799,1.))
REPRESENTATION_ITEM('')
) ;
#1102 = (
BOUNDED_CURVE()
B_SPLINE_CURVE(2,(#41426,#41427,#41428),.UNSPECIFIED.,.F.,.F.)
B_SPLINE_CURVE_WITH_KNOTS((3,3),(0.,1.45676753689758),.UNSPECIFIED.)
CURVE()
GEOMETRIC_REPRESENTATION_ITEM()
RATIONAL_B_SPLINE_CURVE((1.,1.00011064842347,1.))
REPRESENTATION_ITEM('')
) ;
#1103 = (
BOUNDED_CURVE()
B_SPLINE_CURVE(2,(#41450,#41451,#41452),.UNSPECIFIED.,.F.,.F.)
B_SPLINE_CURVE_WITH_KNOTS((3,3),(0.,1.45676753689757),.UNSPECIFIED.)
CURVE()
GEOMETRIC_REPRESENTATION_ITEM()
RATIONAL_B_SPLINE_CURVE((1.,1.00011064825586,1.))
REPRESENTATION_ITEM('')
) ;
#1104 = (
BOUNDED_CURVE()
B_SPLINE_CURVE(2,(#41467,#41468,#41469),.UNSPECIFIED.,.F.,.F.)
B_SPLINE_CURVE_WITH_KNOTS((3,3),(0.,1.45668740131038),.UNSPECIFIED.)
CURVE()
GEOMETRIC_REPRESENTATION_ITEM()
RATIONAL_B_SPLINE_CURVE((1.,1.00010597960991,1.))
REPRESENTATION_ITEM('')
) ;
#1105 = (
BOUNDED_CURVE()
B_SPLINE_CURVE(2,(#41475,#41476,#41477),.UNSPECIFIED.,.F.,.F.)
B_SPLINE_CURVE_WITH_KNOTS((3,3),(0.,1.45668740131038),.UNSPECIFIED.)
CURVE()
GEOMETRIC_REPRESENTATION_ITEM()
RATIONAL_B_SPLINE_CURVE((1.,1.00010597917836,1.))
REPRESENTATION_ITEM('')
) ;
#1106 = (
BOUNDED_CURVE()
B_SPLINE_CURVE(2,(#41484,#41485,#41486),.UNSPECIFIED.,.F.,.F.)
B_SPLINE_CURVE_WITH_KNOTS((3,3),(0.,1.45676753689757),.UNSPECIFIED.)
CURVE()
GEOMETRIC_REPRESENTATION_ITEM()
RATIONAL_B_SPLINE_CURVE((1.,1.00011064860079,1.))
REPRESENTATION_ITEM('')
) ;
#1107 = (
BOUNDED_CURVE()
B_SPLINE_CURVE(2,(#41508,#41509,#41510),.UNSPECIFIED.,.F.,.F.)
B_SPLINE_CURVE_WITH_KNOTS((3,3),(0.,1.45676753689758),.UNSPECIFIED.)
CURVE()
GEOMETRIC_REPRESENTATION_ITEM()
RATIONAL_B_SPLINE_CURVE((1.,1.00011064816854,1.))
REPRESENTATION_ITEM('')
) ;
#1108 = (
BOUNDED_CURVE()
B_SPLINE_CURVE(2,(#41525,#41526,#41527),.UNSPECIFIED.,.F.,.F.)
B_SPLINE_CURVE_WITH_KNOTS((3,3),(0.,1.45668740131038),.UNSPECIFIED.)
CURVE()
GEOMETRIC_REPRESENTATION_ITEM()
RATIONAL_B_SPLINE_CURVE((1.,1.00010597960991,1.))
REPRESENTATION_ITEM('')
) ;
#1109 = (
BOUNDED_CURVE()
B_SPLINE_CURVE(2,(#41533,#41534,#41535),.UNSPECIFIED.,.F.,.F.)
B_SPLINE_CURVE_WITH_KNOTS((3,3),(0.,1.45668740131038),.UNSPECIFIED.)
CURVE()
GEOMETRIC_REPRESENTATION_ITEM()
RATIONAL_B_SPLINE_CURVE((1.,1.00010597917836,1.))
REPRESENTATION_ITEM('')
) ;
#1110 = (
BOUNDED_CURVE()
B_SPLINE_CURVE(2,(#41542,#41543,#41544),.UNSPECIFIED.,.F.,.F.)
B_SPLINE_CURVE_WITH_KNOTS((3,3),(0.,1.45676753689757),.UNSPECIFIED.)
CURVE()
GEOMETRIC_REPRESENTATION_ITEM()
RATIONAL_B_SPLINE_CURVE((1.,1.00011064860079,1.))
REPRESENTATION_ITEM('')
) ;
#1111 = (
BOUNDED_CURVE()
B_SPLINE_CURVE(2,(#41566,#41567,#41568),.UNSPECIFIED.,.F.,.F.)
B_SPLINE_CURVE_WITH_KNOTS((3,3),(0.,1.45676753689758),.UNSPECIFIED.)
CURVE()
GEOMETRIC_REPRESENTATION_ITEM()
RATIONAL_B_SPLINE_CURVE((1.,1.00011064816854,1.))
REPRESENTATION_ITEM('')
) ;
#1112 = FACE_BOUND('',#3896,.T.) ;
#1113 = FACE_BOUND('',#3903,.T.) ;
#1114 = FACE_BOUND('',#3908,.T.) ;
#1115 = FACE_BOUND('',#3915,.T.) ;
#1116 = FACE_BOUND('',#3960,.T.) ;
#1117 = FACE_BOUND('',#3962,.T.) ;
#1118 = FACE_BOUND('',#3964,.T.) ;
#1119 = FACE_BOUND('',#3965,.T.) ;
#1120 = FACE_BOUND('',#3966,.T.) ;
#1121 = FACE_BOUND('',#3967,.T.) ;
#1122 = FACE_BOUND('',#3969,.T.) ;
#1123 = FACE_BOUND('',#3970,.T.) ;
#1124 = FACE_BOUND('',#3971,.T.) ;
#1125 = FACE_BOUND('',#3972,.T.) ;
#1126 = FACE_BOUND('',#3974,.T.) ;
#1127 = FACE_BOUND('',#3985,.T.) ;
#1128 = FACE_BOUND('',#3989,.T.) ;
#1129 = FACE_BOUND('',#3990,.T.) ;
#1130 = FACE_BOUND('',#4023,.T.) ;
#1131 = FACE_BOUND('',#4024,.T.) ;
#1132 = FACE_BOUND('',#4025,.T.) ;
#1133 = FACE_BOUND('',#4026,.T.) ;
#1134 = FACE_BOUND('',#4027,.T.) ;
#1135 = FACE_BOUND('',#4028,.T.) ;
#1136 = FACE_BOUND('',#4029,.T.) ;
#1137 = FACE_BOUND('',#4030,.T.) ;
#1138 = FACE_BOUND('',#4031,.T.) ;
#1139 = FACE_BOUND('',#4032,.T.) ;
#1140 = FACE_BOUND('',#4033,.T.) ;
#1141 = FACE_BOUND('',#4034,.T.) ;
#1142 = FACE_BOUND('',#4035,.T.) ;
#1143 = FACE_BOUND('',#4036,.T.) ;
#1144 = FACE_BOUND('',#4037,.T.) ;
#1145 = FACE_BOUND('',#4038,.T.) ;
#1146 = FACE_BOUND('',#4039,.T.) ;
#1147 = FACE_BOUND('',#4040,.T.) ;
#1148 = FACE_BOUND('',#4041,.T.) ;
#1149 = FACE_BOUND('',#4042,.T.) ;
#1150 = FACE_BOUND('',#4043,.T.) ;
#1151 = FACE_BOUND('',#4044,.T.) ;
#1152 = FACE_BOUND('',#4045,.T.) ;
#1153 = FACE_BOUND('',#4046,.T.) ;
#1154 = FACE_BOUND('',#4047,.T.) ;
#1155 = FACE_BOUND('',#4048,.T.) ;
#1156 = FACE_BOUND('',#4049,.T.) ;
#1157 = FACE_BOUND('',#4050,.T.) ;
#1158 = FACE_BOUND('',#4051,.T.) ;
#1159 = FACE_BOUND('',#4052,.T.) ;
#1160 = FACE_BOUND('',#4053,.T.) ;
#1161 = FACE_BOUND('',#4054,.T.) ;
#1162 = FACE_BOUND('',#4055,.T.) ;
#1163 = FACE_BOUND('',#4056,.T.) ;
#1164 = FACE_BOUND('',#4057,.T.) ;
#1165 = FACE_BOUND('',#4058,.T.) ;
#1166 = FACE_BOUND('',#4059,.T.) ;
#1167 = FACE_BOUND('',#4060,.T.) ;
#1168 = FACE_BOUND('',#4061,.T.) ;
#1169 = FACE_BOUND('',#4062,.T.) ;
#1170 = FACE_BOUND('',#4063,.T.) ;
#1171 = FACE_BOUND('',#4064,.T.) ;
#1172 = FACE_BOUND('',#4065,.T.) ;
#1173 = FACE_BOUND('',#4066,.T.) ;
#1174 = FACE_BOUND('',#4067,.T.) ;
#1175 = FACE_BOUND('',#4068,.T.) ;
#1176 = FACE_BOUND('',#4069,.T.) ;
#1177 = FACE_BOUND('',#4070,.T.) ;
#1178 = FACE_BOUND('',#4071,.T.) ;
#1179 = FACE_BOUND('',#4072,.T.) ;
#1180 = FACE_BOUND('',#4073,.T.) ;
#1181 = FACE_BOUND('',#4074,.T.) ;
#1182 = FACE_BOUND('',#4077,.T.) ;
#1183 = FACE_BOUND('',#4078,.T.) ;
#1184 = FACE_BOUND('',#4079,.T.) ;
#1185 = FACE_BOUND('',#4080,.T.) ;
#1186 = FACE_BOUND('',#4081,.T.) ;
#1187 = FACE_BOUND('',#4082,.T.) ;
#1188 = FACE_BOUND('',#4083,.T.) ;
#1189 = FACE_BOUND('',#4084,.T.) ;
#1190 = FACE_BOUND('',#4085,.T.) ;
#1191 = FACE_BOUND('',#4086,.T.) ;
#1192 = FACE_BOUND('',#4087,.T.) ;
#1193 = FACE_BOUND('',#4088,.T.) ;
#1194 = FACE_BOUND('',#4089,.T.) ;
#1195 = FACE_BOUND('',#4090,.T.) ;
#1196 = FACE_BOUND('',#4091,.T.) ;
#1197 = FACE_BOUND('',#4092,.T.) ;
#1198 = FACE_BOUND('',#4093,.T.) ;
#1199 = FACE_BOUND('',#4094,.T.) ;
#1200 = FACE_BOUND('',#4095,.T.) ;
#1201 = FACE_BOUND('',#4096,.T.) ;
#1202 = FACE_BOUND('',#4097,.T.) ;
#1203 = FACE_BOUND('',#4098,.T.) ;
#1204 = FACE_BOUND('',#4099,.T.) ;
#1205 = FACE_BOUND('',#4100,.T.) ;
#1206 = FACE_BOUND('',#4101,.T.) ;
#1207 = FACE_BOUND('',#4102,.T.) ;
#1208 = FACE_BOUND('',#4103,.T.) ;
#1209 = FACE_BOUND('',#4104,.T.) ;
#1210 = FACE_BOUND('',#4105,.T.) ;
#1211 = FACE_BOUND('',#4106,.T.) ;
#1212 = FACE_BOUND('',#4107,.T.) ;
#1213 = FACE_BOUND('',#4108,.T.) ;
#1214 = FACE_BOUND('',#4109,.T.) ;
#1215 = FACE_BOUND('',#4110,.T.) ;
#1216 = FACE_BOUND('',#4111,.T.) ;
#1217 = FACE_BOUND('',#4112,.T.) ;
#1218 = FACE_BOUND('',#4113,.T.) ;
#1219 = FACE_BOUND('',#4114,.T.) ;
#1220 = FACE_BOUND('',#4115,.T.) ;
#1221 = FACE_BOUND('',#4116,.T.) ;
#1222 = FACE_BOUND('',#4117,.T.) ;
#1223 = FACE_BOUND('',#4118,.T.) ;
#1224 = FACE_BOUND('',#4119,.T.) ;
#1225 = FACE_BOUND('',#4120,.T.) ;
#1226 = FACE_BOUND('',#4121,.T.) ;
#1227 = FACE_BOUND('',#4122,.T.) ;
#1228 = FACE_BOUND('',#4123,.T.) ;
#1229 = FACE_BOUND('',#4124,.T.) ;
#1230 = FACE_BOUND('',#4125,.T.) ;
#1231 = FACE_BOUND('',#4126,.T.) ;
#1232 = FACE_BOUND('',#4127,.T.) ;
#1233 = FACE_BOUND('',#4128,.T.) ;
#1234 = FACE_BOUND('',#4462,.T.) ;
#1235 = FACE_BOUND('',#4463,.T.) ;
#1236 = FACE_BOUND('',#4465,.T.) ;
#1237 = FACE_BOUND('',#4466,.T.) ;
#1238 = FACE_BOUND('',#4476,.T.) ;
#1239 = FACE_BOUND('',#4477,.T.) ;
#1240 = FACE_BOUND('',#4479,.T.) ;
#1241 = FACE_BOUND('',#4480,.T.) ;
#1242 = FACE_BOUND('',#4488,.T.) ;
#1243 = FACE_BOUND('',#4490,.T.) ;
#1244 = FACE_BOUND('',#4491,.T.) ;
#1245 = FACE_BOUND('',#4492,.T.) ;
#1246 = FACE_BOUND('',#4493,.T.) ;
#1247 = FACE_BOUND('',#4497,.T.) ;
#1248 = FACE_BOUND('',#4504,.T.) ;
#1249 = FACE_BOUND('',#4508,.T.) ;
#1250 = FACE_BOUND('',#4509,.T.) ;
#1251 = FACE_BOUND('',#4527,.T.) ;
#1252 = FACE_BOUND('',#4536,.T.) ;
#1253 = FACE_BOUND('',#4541,.T.) ;
#1254 = FACE_BOUND('',#4550,.T.) ;
#1255 = FACE_BOUND('',#4552,.T.) ;
#1256 = FACE_BOUND('',#4564,.T.) ;
#1257 = FACE_BOUND('',#4566,.T.) ;
#1258 = FACE_BOUND('',#4569,.T.) ;
#1259 = FACE_BOUND('',#4570,.T.) ;
#1260 = FACE_BOUND('',#4574,.T.) ;
#1261 = FACE_BOUND('',#4581,.T.) ;
#1262 = FACE_BOUND('',#4585,.T.) ;
#1263 = FACE_BOUND('',#4586,.T.) ;
#1264 = FACE_BOUND('',#4587,.T.) ;
#1265 = FACE_BOUND('',#4588,.T.) ;
#1266 = FACE_BOUND('',#4590,.T.) ;
#1267 = FACE_BOUND('',#4605,.T.) ;
#1268 = FACE_BOUND('',#4609,.T.) ;
#1269 = FACE_BOUND('',#4613,.T.) ;
#1270 = FACE_BOUND('',#4727,.T.) ;
#1271 = FACE_BOUND('',#4731,.T.) ;
#1272 = FACE_BOUND('',#4732,.T.) ;
#1273 = FACE_BOUND('',#4736,.T.) ;
#1274 = FACE_BOUND('',#4740,.T.) ;
#1275 = FACE_BOUND('',#4741,.T.) ;
#1276 = FACE_BOUND('',#4753,.T.) ;
#1277 = FACE_BOUND('',#4757,.T.) ;
#1278 = FACE_BOUND('',#4764,.T.) ;
#1279 = FACE_BOUND('',#4785,.T.) ;
#1280 = FACE_BOUND('',#4790,.T.) ;
#1281 = FACE_BOUND('',#4795,.T.) ;
#1282 = FACE_BOUND('',#4797,.T.) ;
#1283 = FACE_BOUND('',#4799,.T.) ;
#1284 = FACE_BOUND('',#4803,.T.) ;
#1285 = FACE_BOUND('',#4805,.T.) ;
#1286 = FACE_BOUND('',#4807,.T.) ;
#1287 = FACE_BOUND('',#4811,.T.) ;
#1288 = FACE_BOUND('',#4813,.T.) ;
#1289 = FACE_BOUND('',#4817,.T.) ;
#1290 = FACE_BOUND('',#4819,.T.) ;
#1291 = FACE_BOUND('',#4824,.T.) ;
#1292 = FACE_BOUND('',#4825,.T.) ;
#1293 = FACE_BOUND('',#4826,.T.) ;
#1294 = FACE_BOUND('',#4832,.T.) ;
#1295 = FACE_BOUND('',#4895,.T.) ;
#1296 = FACE_BOUND('',#4898,.T.) ;
#1297 = FACE_BOUND('',#4902,.T.) ;
#1298 = FACE_BOUND('',#4904,.T.) ;
#1299 = FACE_BOUND('',#4927,.T.) ;
#1300 = FACE_BOUND('',#4928,.T.) ;
#1301 = FACE_BOUND('',#4930,.T.) ;
#1302 = FACE_BOUND('',#4934,.T.) ;
#1303 = FACE_BOUND('',#4936,.T.) ;
#1304 = FACE_BOUND('',#4940,.T.) ;
#1305 = FACE_BOUND('',#4942,.T.) ;
#1306 = FACE_BOUND('',#4947,.T.) ;
#1307 = FACE_BOUND('',#4949,.T.) ;
#1308 = FACE_BOUND('',#4952,.T.) ;
#1309 = FACE_BOUND('',#4953,.T.) ;
#1310 = FACE_BOUND('',#4954,.T.) ;
#1311 = FACE_BOUND('',#4955,.T.) ;
#1312 = FACE_BOUND('',#4956,.T.) ;
#1313 = FACE_BOUND('',#4957,.T.) ;
#1314 = FACE_BOUND('',#5004,.T.) ;
#1315 = FACE_BOUND('',#5006,.T.) ;
#1316 = FACE_BOUND('',#5009,.T.) ;
#1317 = FACE_BOUND('',#5014,.T.) ;
#1318 = FACE_BOUND('',#5021,.T.) ;
#1319 = FACE_BOUND('',#5024,.T.) ;
#1320 = FACE_BOUND('',#5031,.T.) ;
#1321 = FACE_BOUND('',#5032,.T.) ;
#1322 = FACE_BOUND('',#5035,.T.) ;
#1323 = FACE_BOUND('',#5036,.T.) ;
#1324 = FACE_BOUND('',#5042,.T.) ;
#1325 = FACE_BOUND('',#5043,.T.) ;
#1326 = FACE_BOUND('',#5049,.T.) ;
#1327 = FACE_BOUND('',#5050,.T.) ;
#1328 = FACE_BOUND('',#5051,.T.) ;
#1329 = FACE_BOUND('',#5052,.T.) ;
#1330 = FACE_BOUND('',#5053,.T.) ;
#1331 = FACE_BOUND('',#5054,.T.) ;
#1332 = FACE_BOUND('',#5081,.T.) ;
#1333 = FACE_BOUND('',#5082,.T.) ;
#1334 = FACE_BOUND('',#5083,.T.) ;
#1335 = FACE_BOUND('',#5085,.T.) ;
#1336 = FACE_BOUND('',#5086,.T.) ;
#1337 = FACE_BOUND('',#5087,.T.) ;
#1338 = FACE_BOUND('',#5137,.T.) ;
#1339 = FACE_BOUND('',#5139,.T.) ;
#1340 = FACE_BOUND('',#5140,.T.) ;
#1341 = FACE_BOUND('',#5141,.T.) ;
#1342 = FACE_BOUND('',#5142,.T.) ;
#1343 = FACE_BOUND('',#5143,.T.) ;
#1344 = FACE_BOUND('',#5147,.T.) ;
#1345 = FACE_BOUND('',#5148,.T.) ;
#1346 = FACE_BOUND('',#5149,.T.) ;
#1347 = FACE_BOUND('',#5150,.T.) ;
#1348 = FACE_BOUND('',#5151,.T.) ;
#1349 = FACE_BOUND('',#5158,.T.) ;
#1350 = FACE_BOUND('',#5163,.T.) ;
#1351 = FACE_BOUND('',#5165,.T.) ;
#1352 = FACE_BOUND('',#5167,.T.) ;
#1353 = FACE_BOUND('',#5169,.T.) ;
#1354 = FACE_BOUND('',#5182,.T.) ;
#1355 = FACE_BOUND('',#5183,.T.) ;
#1356 = FACE_BOUND('',#5184,.T.) ;
#1357 = FACE_BOUND('',#5185,.T.) ;
#1358 = FACE_BOUND('',#5186,.T.) ;
#1359 = FACE_BOUND('',#5187,.T.) ;
#1360 = FACE_BOUND('',#5188,.T.) ;
#1361 = FACE_BOUND('',#5189,.T.) ;
#1362 = FACE_BOUND('',#5191,.T.) ;
#1363 = FACE_BOUND('',#5192,.T.) ;
#1364 = FACE_BOUND('',#5193,.T.) ;
#1365 = FACE_BOUND('',#5194,.T.) ;
#1366 = FACE_BOUND('',#5195,.T.) ;
#1367 = FACE_BOUND('',#5196,.T.) ;
#1368 = FACE_BOUND('',#5197,.T.) ;
#1369 = FACE_BOUND('',#5198,.T.) ;
#1370 = FACE_BOUND('',#5206,.T.) ;
#1371 = FACE_BOUND('',#5211,.T.) ;
#1372 = FACE_BOUND('',#5213,.T.) ;
#1373 = FACE_BOUND('',#5215,.T.) ;
#1374 = FACE_BOUND('',#5218,.T.) ;
#1375 = FACE_BOUND('',#5229,.T.) ;
#1376 = FACE_BOUND('',#5234,.T.) ;
#1377 = FACE_BOUND('',#5253,.T.) ;
#1378 = FACE_BOUND('',#5261,.T.) ;
#1379 = FACE_BOUND('',#5297,.T.) ;
#1380 = FACE_BOUND('',#5300,.T.) ;
#1381 = FACE_BOUND('',#5302,.T.) ;
#1382 = FACE_BOUND('',#5308,.T.) ;
#1383 = FACE_BOUND('',#5310,.T.) ;
#1384 = FACE_BOUND('',#5314,.T.) ;
#1385 = FACE_BOUND('',#5316,.T.) ;
#1386 = FACE_BOUND('',#5577,.T.) ;
#1387 = FACE_BOUND('',#5579,.T.) ;
#1388 = FACE_BOUND('',#5587,.T.) ;
#1389 = FACE_BOUND('',#5591,.T.) ;
#1390 = FACE_BOUND('',#5605,.T.) ;
#1391 = FACE_BOUND('',#5612,.T.) ;
#1392 = FACE_BOUND('',#5618,.T.) ;
#1393 = FACE_BOUND('',#5622,.T.) ;
#1394 = FACE_BOUND('',#5624,.T.) ;
#1395 = FACE_BOUND('',#5626,.T.) ;
#1396 = FACE_BOUND('',#5632,.T.) ;
#1397 = FACE_BOUND('',#5634,.T.) ;
#1398 = FACE_BOUND('',#5656,.T.) ;
#1399 = FACE_BOUND('',#5660,.T.) ;
#1400 = FACE_BOUND('',#5671,.T.) ;
#1401 = FACE_BOUND('',#5676,.T.) ;
#1402 = FACE_BOUND('',#5682,.T.) ;
#1403 = FACE_BOUND('',#5693,.T.) ;
#1404 = FACE_BOUND('',#5698,.T.) ;
#1405 = FACE_BOUND('',#5704,.T.) ;
#1406 = FACE_BOUND('',#5706,.T.) ;
#1407 = FACE_BOUND('',#5712,.T.) ;
#1408 = PLANE('',#29217) ;
#1409 = PLANE('',#29218) ;
#1410 = PLANE('',#29219) ;
#1411 = PLANE('',#29220) ;
#1412 = PLANE('',#29221) ;
#1413 = PLANE('',#29223) ;
#1414 = PLANE('',#29224) ;
#1415 = PLANE('',#29225) ;
#1416 = PLANE('',#29235) ;
#1417 = PLANE('',#29236) ;
#1418 = PLANE('',#29237) ;
#1419 = PLANE('',#29238) ;
#1420 = PLANE('',#29239) ;
#1421 = PLANE('',#29240) ;
#1422 = PLANE('',#29241) ;
#1423 = PLANE('',#29242) ;
#1424 = PLANE('',#29243) ;
#1425 = PLANE('',#29245) ;
#1426 = PLANE('',#29246) ;
#1427 = PLANE('',#29247) ;
#1428 = PLANE('',#29248) ;
#1429 = PLANE('',#29250) ;
#1430 = PLANE('',#29252) ;
#1431 = PLANE('',#29254) ;
#1432 = PLANE('',#29255) ;
#1433 = PLANE('',#29256) ;
#1434 = PLANE('',#29257) ;
#1435 = PLANE('',#29259) ;
#1436 = PLANE('',#29260) ;
#1437 = PLANE('',#29261) ;
#1438 = PLANE('',#29262) ;
#1439 = PLANE('',#29264) ;
#1440 = PLANE('',#29266) ;
#1441 = PLANE('',#29268) ;
#1442 = PLANE('',#29269) ;
#1443 = PLANE('',#29270) ;
#1444 = PLANE('',#29271) ;
#1445 = PLANE('',#29273) ;
#1446 = PLANE('',#29274) ;
#1447 = PLANE('',#29275) ;
#1448 = PLANE('',#29276) ;
#1449 = PLANE('',#29278) ;
#1450 = PLANE('',#29280) ;
#1451 = PLANE('',#29282) ;
#1452 = PLANE('',#29283) ;
#1453 = PLANE('',#29284) ;
#1454 = PLANE('',#29285) ;
#1455 = PLANE('',#29287) ;
#1456 = PLANE('',#29288) ;
#1457 = PLANE('',#29289) ;
#1458 = PLANE('',#29290) ;
#1459 = PLANE('',#29292) ;
#1460 = PLANE('',#29294) ;
#1461 = PLANE('',#29296) ;
#1462 = PLANE('',#29297) ;
#1463 = PLANE('',#29298) ;
#1464 = PLANE('',#29305) ;
#1465 = PLANE('',#29306) ;
#1466 = PLANE('',#29311) ;
#1467 = PLANE('',#29313) ;
#1468 = PLANE('',#29314) ;
#1469 = PLANE('',#29315) ;
#1470 = PLANE('',#29316) ;
#1471 = PLANE('',#29317) ;
#1472 = PLANE('',#29318) ;
#1473 = PLANE('',#29319) ;
#1474 = PLANE('',#29320) ;
#1475 = PLANE('',#29324) ;
#1476 = PLANE('',#29328) ;
#1477 = PLANE('',#29329) ;
#1478 = PLANE('',#29331) ;
#1479 = PLANE('',#29332) ;
#1480 = PLANE('',#29333) ;
#1481 = PLANE('',#29334) ;
#1482 = PLANE('',#29338) ;
#1483 = PLANE('',#29340) ;
#1484 = PLANE('',#29341) ;
#1485 = PLANE('',#29342) ;
#1486 = PLANE('',#29343) ;
#1487 = PLANE('',#29344) ;
#1488 = PLANE('',#29345) ;
#1489 = PLANE('',#29346) ;
#1490 = PLANE('',#29347) ;
#1491 = PLANE('',#29348) ;
#1492 = PLANE('',#29349) ;
#1493 = PLANE('',#29350) ;
#1494 = PLANE('',#29351) ;
#1495 = PLANE('',#29352) ;
#1496 = PLANE('',#29353) ;
#1497 = PLANE('',#29363) ;
#1498 = PLANE('',#29364) ;
#1499 = PLANE('',#29365) ;
#1500 = PLANE('',#29366) ;
#1501 = PLANE('',#29367) ;
#1502 = PLANE('',#29368) ;
#1503 = PLANE('',#29369) ;
#1504 = PLANE('',#29370) ;
#1505 = PLANE('',#29371) ;
#1506 = PLANE('',#29419) ;
#1507 = PLANE('',#29466) ;
#1508 = PLANE('',#29467) ;
#1509 = PLANE('',#29468) ;
#1510 = PLANE('',#29469) ;
#1511 = PLANE('',#29470) ;
#1512 = PLANE('',#29471) ;
#1513 = PLANE('',#29472) ;
#1514 = PLANE('',#29473) ;
#1515 = PLANE('',#29474) ;
#1516 = PLANE('',#29475) ;
#1517 = PLANE('',#29476) ;
#1518 = PLANE('',#29477) ;
#1519 = PLANE('',#29478) ;
#1520 = PLANE('',#29479) ;
#1521 = PLANE('',#29480) ;
#1522 = PLANE('',#29481) ;
#1523 = PLANE('',#29482) ;
#1524 = PLANE('',#29485) ;
#1525 = PLANE('',#29486) ;
#1526 = PLANE('',#29487) ;
#1527 = PLANE('',#29488) ;
#1528 = PLANE('',#29489) ;
#1529 = PLANE('',#29493) ;
#1530 = PLANE('',#29494) ;
#1531 = PLANE('',#29495) ;
#1532 = PLANE('',#29496) ;
#1533 = PLANE('',#29497) ;
#1534 = PLANE('',#29498) ;
#1535 = PLANE('',#29499) ;
#1536 = PLANE('',#29500) ;
#1537 = PLANE('',#29501) ;
#1538 = PLANE('',#29502) ;
#1539 = PLANE('',#29503) ;
#1540 = PLANE('',#29504) ;
#1541 = PLANE('',#29505) ;
#1542 = PLANE('',#29506) ;
#1543 = PLANE('',#29507) ;
#1544 = PLANE('',#29508) ;
#1545 = PLANE('',#29509) ;
#1546 = PLANE('',#29511) ;
#1547 = PLANE('',#29512) ;
#1548 = PLANE('',#29513) ;
#1549 = PLANE('',#29514) ;
#1550 = PLANE('',#29515) ;
#1551 = PLANE('',#29516) ;
#1552 = PLANE('',#29517) ;
#1553 = PLANE('',#29518) ;
#1554 = PLANE('',#29520) ;
#1555 = PLANE('',#29521) ;
#1556 = PLANE('',#29522) ;
#1557 = PLANE('',#29523) ;
#1558 = PLANE('',#29524) ;
#1559 = PLANE('',#29525) ;
#1560 = PLANE('',#29526) ;
#1561 = PLANE('',#29527) ;
#1562 = PLANE('',#29528) ;
#1563 = PLANE('',#29529) ;
#1564 = PLANE('',#29530) ;
#1565 = PLANE('',#29531) ;
#1566 = PLANE('',#29532) ;
#1567 = PLANE('',#29533) ;
#1568 = PLANE('',#29534) ;
#1569 = PLANE('',#29535) ;
#1570 = PLANE('',#29536) ;
#1571 = PLANE('',#29537) ;
#1572 = PLANE('',#29538) ;
#1573 = PLANE('',#29541) ;
#1574 = PLANE('',#29544) ;
#1575 = PLANE('',#29545) ;
#1576 = PLANE('',#29546) ;
#1577 = PLANE('',#29547) ;
#1578 = PLANE('',#29548) ;
#1579 = PLANE('',#29549) ;
#1580 = PLANE('',#29550) ;
#1581 = PLANE('',#29551) ;
#1582 = PLANE('',#29552) ;
#1583 = PLANE('',#29553) ;
#1584 = PLANE('',#29554) ;
#1585 = PLANE('',#29555) ;
#1586 = PLANE('',#29556) ;
#1587 = PLANE('',#29557) ;
#1588 = PLANE('',#29558) ;
#1589 = PLANE('',#29559) ;
#1590 = PLANE('',#29560) ;
#1591 = PLANE('',#29561) ;
#1592 = PLANE('',#29562) ;
#1593 = PLANE('',#29563) ;
#1594 = PLANE('',#29564) ;
#1595 = PLANE('',#29565) ;
#1596 = PLANE('',#29570) ;
#1597 = PLANE('',#29571) ;
#1598 = PLANE('',#29572) ;
#1599 = PLANE('',#29573) ;
#1600 = PLANE('',#29574) ;
#1601 = PLANE('',#29575) ;
#1602 = PLANE('',#29576) ;
#1603 = PLANE('',#29577) ;
#1604 = PLANE('',#29578) ;
#1605 = PLANE('',#29579) ;
#1606 = PLANE('',#29580) ;
#1607 = PLANE('',#29581) ;
#1608 = PLANE('',#29582) ;
#1609 = PLANE('',#29583) ;
#1610 = PLANE('',#29584) ;
#1611 = PLANE('',#29585) ;
#1612 = PLANE('',#29586) ;
#1613 = PLANE('',#29587) ;
#1614 = PLANE('',#29588) ;
#1615 = PLANE('',#29589) ;
#1616 = PLANE('',#29590) ;
#1617 = PLANE('',#29591) ;
#1618 = PLANE('',#29592) ;
#1619 = PLANE('',#29593) ;
#1620 = PLANE('',#29597) ;
#1621 = PLANE('',#29598) ;
#1622 = PLANE('',#29599) ;
#1623 = PLANE('',#29600) ;
#1624 = PLANE('',#29601) ;
#1625 = PLANE('',#29602) ;
#1626 = PLANE('',#29605) ;
#1627 = PLANE('',#29606) ;
#1628 = PLANE('',#29607) ;
#1629 = PLANE('',#29608) ;
#1630 = PLANE('',#29609) ;
#1631 = PLANE('',#29610) ;
#1632 = PLANE('',#29611) ;
#1633 = PLANE('',#29612) ;
#1634 = PLANE('',#29613) ;
#1635 = PLANE('',#29614) ;
#1636 = PLANE('',#29615) ;
#1637 = PLANE('',#29616) ;
#1638 = PLANE('',#29617) ;
#1639 = PLANE('',#29618) ;
#1640 = PLANE('',#29619) ;
#1641 = PLANE('',#29620) ;
#1642 = PLANE('',#29621) ;
#1643 = PLANE('',#29622) ;
#1644 = PLANE('',#29625) ;
#1645 = PLANE('',#29626) ;
#1646 = PLANE('',#29630) ;
#1647 = PLANE('',#29631) ;
#1648 = PLANE('',#29632) ;
#1649 = PLANE('',#29633) ;
#1650 = PLANE('',#29634) ;
#1651 = PLANE('',#29635) ;
#1652 = PLANE('',#29636) ;
#1653 = PLANE('',#29637) ;
#1654 = PLANE('',#29638) ;
#1655 = PLANE('',#29639) ;
#1656 = PLANE('',#29640) ;
#1657 = PLANE('',#29641) ;
#1658 = PLANE('',#29642) ;
#1659 = PLANE('',#29643) ;
#1660 = PLANE('',#29644) ;
#1661 = PLANE('',#29645) ;
#1662 = PLANE('',#29646) ;
#1663 = PLANE('',#29647) ;
#1664 = PLANE('',#29648) ;
#1665 = PLANE('',#29649) ;
#1666 = PLANE('',#29650) ;
#1667 = PLANE('',#29651) ;
#1668 = PLANE('',#29653) ;
#1669 = PLANE('',#29654) ;
#1670 = PLANE('',#29658) ;
#1671 = PLANE('',#29659) ;
#1672 = PLANE('',#29660) ;
#1673 = PLANE('',#29661) ;
#1674 = PLANE('',#29662) ;
#1675 = PLANE('',#29663) ;
#1676 = PLANE('',#29664) ;
#1677 = PLANE('',#29665) ;
#1678 = PLANE('',#29666) ;
#1679 = PLANE('',#29667) ;
#1680 = PLANE('',#29668) ;
#1681 = PLANE('',#29669) ;
#1682 = PLANE('',#29670) ;
#1683 = PLANE('',#29671) ;
#1684 = PLANE('',#29672) ;
#1685 = PLANE('',#29673) ;
#1686 = PLANE('',#29675) ;
#1687 = PLANE('',#29676) ;
#1688 = PLANE('',#29679) ;
#1689 = PLANE('',#29680) ;
#1690 = PLANE('',#29681) ;
#1691 = PLANE('',#29682) ;
#1692 = PLANE('',#29683) ;
#1693 = PLANE('',#29684) ;
#1694 = PLANE('',#29685) ;
#1695 = PLANE('',#29686) ;
#1696 = PLANE('',#29687) ;
#1697 = PLANE('',#29688) ;
#1698 = PLANE('',#29689) ;
#1699 = PLANE('',#29693) ;
#1700 = PLANE('',#29694) ;
#1701 = PLANE('',#29697) ;
#1702 = PLANE('',#29698) ;
#1703 = PLANE('',#29699) ;
#1704 = PLANE('',#29700) ;
#1705 = PLANE('',#29701) ;
#1706 = PLANE('',#29702) ;
#1707 = PLANE('',#29703) ;
#1708 = PLANE('',#29704) ;
#1709 = PLANE('',#29705) ;
#1710 = PLANE('',#29707) ;
#1711 = PLANE('',#29709) ;
#1712 = PLANE('',#29710) ;
#1713 = PLANE('',#29711) ;
#1714 = PLANE('',#29712) ;
#1715 = PLANE('',#29713) ;
#1716 = PLANE('',#29714) ;
#1717 = PLANE('',#29715) ;
#1718 = PLANE('',#29717) ;
#1719 = PLANE('',#29718) ;
#1720 = PLANE('',#29719) ;
#1721 = PLANE('',#29720) ;
#1722 = PLANE('',#29721) ;
#1723 = PLANE('',#29724) ;
#1724 = PLANE('',#29725) ;
#1725 = PLANE('',#29726) ;
#1726 = PLANE('',#29727) ;
#1727 = PLANE('',#29728) ;
#1728 = PLANE('',#29729) ;
#1729 = PLANE('',#29943) ;
#1730 = PLANE('',#29944) ;
#1731 = PLANE('',#29945) ;
#1732 = PLANE('',#29946) ;
#1733 = PLANE('',#29947) ;
#1734 = PLANE('',#29948) ;
#1735 = PLANE('',#29949) ;
#1736 = PLANE('',#29959) ;
#1737 = PLANE('',#29960) ;
#1738 = PLANE('',#29961) ;
#1739 = PLANE('',#29962) ;
#1740 = PLANE('',#29963) ;
#1741 = PLANE('',#29964) ;
#1742 = PLANE('',#29965) ;
#1743 = PLANE('',#29978) ;
#1744 = PLANE('',#29979) ;
#1745 = PLANE('',#29986) ;
#1746 = PLANE('',#29987) ;
#1747 = PLANE('',#29988) ;
#1748 = PLANE('',#29989) ;
#1749 = PLANE('',#29990) ;
#1750 = PLANE('',#29991) ;
#1751 = PLANE('',#29992) ;
#1752 = PLANE('',#29993) ;
#1753 = PLANE('',#29994) ;
#1754 = PLANE('',#29995) ;
#1755 = PLANE('',#29996) ;
#1756 = PLANE('',#29997) ;
#1757 = PLANE('',#29998) ;
#1758 = PLANE('',#30000) ;
#1759 = PLANE('',#30001) ;
#1760 = PLANE('',#30003) ;
#1761 = PLANE('',#30004) ;
#1762 = PLANE('',#30005) ;
#1763 = PLANE('',#30007) ;
#1764 = PLANE('',#30009) ;
#1765 = PLANE('',#30010) ;
#1766 = PLANE('',#30011) ;
#1767 = PLANE('',#30012) ;
#1768 = PLANE('',#30013) ;
#1769 = PLANE('',#30014) ;
#1770 = PLANE('',#30016) ;
#1771 = PLANE('',#30018) ;
#1772 = PLANE('',#30019) ;
#1773 = PLANE('',#30021) ;
#1774 = PLANE('',#30022) ;
#1775 = PLANE('',#30023) ;
#1776 = PLANE('',#30024) ;
#1777 = PLANE('',#30025) ;
#1778 = PLANE('',#30026) ;
#1779 = PLANE('',#30027) ;
#1780 = PLANE('',#30028) ;
#1781 = PLANE('',#30029) ;
#1782 = PLANE('',#30031) ;
#1783 = PLANE('',#30033) ;
#1784 = PLANE('',#30034) ;
#1785 = PLANE('',#30035) ;
#1786 = PLANE('',#30036) ;
#1787 = PLANE('',#30038) ;
#1788 = PLANE('',#30039) ;
#1789 = PLANE('',#30040) ;
#1790 = PLANE('',#30041) ;
#1791 = PLANE('',#30042) ;
#1792 = PLANE('',#30045) ;
#1793 = PLANE('',#30052) ;
#1794 = PLANE('',#30053) ;
#1795 = PLANE('',#30054) ;
#1796 = PLANE('',#30055) ;
#1797 = PLANE('',#30056) ;
#1798 = PLANE('',#30057) ;
#1799 = PLANE('',#30058) ;
#1800 = PLANE('',#30059) ;
#1801 = PLANE('',#30060) ;
#1802 = PLANE('',#30061) ;
#1803 = PLANE('',#30062) ;
#1804 = PLANE('',#30063) ;
#1805 = PLANE('',#30064) ;
#1806 = PLANE('',#30065) ;
#1807 = PLANE('',#30066) ;
#1808 = PLANE('',#30067) ;
#1809 = PLANE('',#30068) ;
#1810 = PLANE('',#30069) ;
#1811 = PLANE('',#30071) ;
#1812 = PLANE('',#30077) ;
#1813 = PLANE('',#30079) ;
#1814 = PLANE('',#30088) ;
#1815 = PLANE('',#30089) ;
#1816 = PLANE('',#30090) ;
#1817 = PLANE('',#30091) ;
#1818 = PLANE('',#30092) ;
#1819 = PLANE('',#30093) ;
#1820 = PLANE('',#30094) ;
#1821 = PLANE('',#30095) ;
#1822 = PLANE('',#30096) ;
#1823 = PLANE('',#30097) ;
#1824 = PLANE('',#30098) ;
#1825 = PLANE('',#30099) ;
#1826 = PLANE('',#30100) ;
#1827 = PLANE('',#30101) ;
#1828 = PLANE('',#30102) ;
#1829 = PLANE('',#30103) ;
#1830 = PLANE('',#30104) ;
#1831 = PLANE('',#30105) ;
#1832 = PLANE('',#30109) ;
#1833 = PLANE('',#30110) ;
#1834 = PLANE('',#30111) ;
#1835 = PLANE('',#30112) ;
#1836 = PLANE('',#30113) ;
#1837 = PLANE('',#30114) ;
#1838 = PLANE('',#30115) ;
#1839 = PLANE('',#30117) ;
#1840 = PLANE('',#30118) ;
#1841 = PLANE('',#30120) ;
#1842 = PLANE('',#30122) ;
#1843 = PLANE('',#30124) ;
#1844 = PLANE('',#30126) ;
#1845 = PLANE('',#30128) ;
#1846 = PLANE('',#30129) ;
#1847 = PLANE('',#30130) ;
#1848 = PLANE('',#30132) ;
#1849 = PLANE('',#30135) ;
#1850 = PLANE('',#30137) ;
#1851 = PLANE('',#30138) ;
#1852 = PLANE('',#30141) ;
#1853 = PLANE('',#30142) ;
#1854 = PLANE('',#30143) ;
#1855 = PLANE('',#30144) ;
#1856 = PLANE('',#30146) ;
#1857 = PLANE('',#30149) ;
#1858 = PLANE('',#30151) ;
#1859 = PLANE('',#30154) ;
#1860 = PLANE('',#30155) ;
#1861 = PLANE('',#30156) ;
#1862 = PLANE('',#30160) ;
#1863 = PLANE('',#30161) ;
#1864 = PLANE('',#30162) ;
#1865 = PLANE('',#30163) ;
#1866 = PLANE('',#30165) ;
#1867 = PLANE('',#30168) ;
#1868 = PLANE('',#30169) ;
#1869 = PLANE('',#30170) ;
#1870 = PLANE('',#30171) ;
#1871 = PLANE('',#30173) ;
#1872 = PLANE('',#30179) ;
#1873 = PLANE('',#30180) ;
#1874 = PLANE('',#30181) ;
#1875 = PLANE('',#30182) ;
#1876 = PLANE('',#30183) ;
#1877 = PLANE('',#30185) ;
#1878 = PLANE('',#30191) ;
#1879 = PLANE('',#30192) ;
#1880 = PLANE('',#30193) ;
#1881 = PLANE('',#30194) ;
#1882 = PLANE('',#30195) ;
#1883 = PLANE('',#30199) ;
#1884 = PLANE('',#30200) ;
#1885 = PLANE('',#30201) ;
#1886 = PLANE('',#30202) ;
#1887 = PLANE('',#30203) ;
#1888 = PLANE('',#30204) ;
#1889 = PLANE('',#30205) ;
#1890 = PLANE('',#30206) ;
#1891 = PLANE('',#30207) ;
#1892 = PLANE('',#30208) ;
#1893 = PLANE('',#30209) ;
#1894 = PLANE('',#30210) ;
#1895 = PLANE('',#30211) ;
#1896 = PLANE('',#30212) ;
#1897 = PLANE('',#30213) ;
#1898 = PLANE('',#30214) ;
#1899 = PLANE('',#30215) ;
#1900 = PLANE('',#30216) ;
#1901 = PLANE('',#30217) ;
#1902 = PLANE('',#30218) ;
#1903 = PLANE('',#30219) ;
#1904 = PLANE('',#30220) ;
#1905 = PLANE('',#30221) ;
#1906 = PLANE('',#30222) ;
#1907 = PLANE('',#30223) ;
#1908 = PLANE('',#30224) ;
#1909 = PLANE('',#30225) ;
#1910 = PLANE('',#30229) ;
#1911 = PLANE('',#30230) ;
#1912 = PLANE('',#30231) ;
#1913 = PLANE('',#30232) ;
#1914 = PLANE('',#30234) ;
#1915 = PLANE('',#30241) ;
#1916 = PLANE('',#30242) ;
#1917 = PLANE('',#30243) ;
#1918 = PLANE('',#30244) ;
#1919 = PLANE('',#30245) ;
#1920 = PLANE('',#30247) ;
#1921 = PLANE('',#30248) ;
#1922 = PLANE('',#30249) ;
#1923 = PLANE('',#30250) ;
#1924 = PLANE('',#30251) ;
#1925 = PLANE('',#30252) ;
#1926 = PLANE('',#30255) ;
#1927 = PLANE('',#30260) ;
#1928 = PLANE('',#30263) ;
#1929 = PLANE('',#30266) ;
#1930 = PLANE('',#30271) ;
#1931 = PLANE('',#30274) ;
#1932 = PLANE('',#30300) ;
#1933 = PLANE('',#30301) ;
#1934 = PLANE('',#30310) ;
#1935 = PLANE('',#30313) ;
#1936 = PLANE('',#30315) ;
#1937 = PLANE('',#30318) ;
#1938 = PLANE('',#30320) ;
#1939 = PLANE('',#30326) ;
#1940 = PLANE('',#30329) ;
#1941 = PLANE('',#30336) ;
#1942 = PLANE('',#30337) ;
#1943 = PLANE('',#30338) ;
#1944 = PLANE('',#30339) ;
#1945 = PLANE('',#30340) ;
#1946 = PLANE('',#30341) ;
#1947 = PLANE('',#30342) ;
#1948 = PLANE('',#30343) ;
#1949 = PLANE('',#30344) ;
#1950 = PLANE('',#30345) ;
#1951 = PLANE('',#30346) ;
#1952 = PLANE('',#30347) ;
#1953 = PLANE('',#30348) ;
#1954 = PLANE('',#30358) ;
#1955 = PLANE('',#30359) ;
#1956 = PLANE('',#30363) ;
#1957 = PLANE('',#30367) ;
#1958 = PLANE('',#30371) ;
#1959 = PLANE('',#30374) ;
#1960 = PLANE('',#30375) ;
#1961 = PLANE('',#30376) ;
#1962 = PLANE('',#30377) ;
#1963 = PLANE('',#30378) ;
#1964 = PLANE('',#30379) ;
#1965 = PLANE('',#30380) ;
#1966 = PLANE('',#30381) ;
#1967 = PLANE('',#30382) ;
#1968 = PLANE('',#30383) ;
#1969 = PLANE('',#30384) ;
#1970 = PLANE('',#30385) ;
#1971 = PLANE('',#30386) ;
#1972 = PLANE('',#30387) ;
#1973 = PLANE('',#30388) ;
#1974 = PLANE('',#30389) ;
#1975 = PLANE('',#30390) ;
#1976 = PLANE('',#30391) ;
#1977 = PLANE('',#30392) ;
#1978 = PLANE('',#30393) ;
#1979 = PLANE('',#30398) ;
#1980 = PLANE('',#30399) ;
#1981 = PLANE('',#30400) ;
#1982 = PLANE('',#30401) ;
#1983 = PLANE('',#30402) ;
#1984 = PLANE('',#30403) ;
#1985 = PLANE('',#30404) ;
#1986 = PLANE('',#30405) ;
#1987 = PLANE('',#30406) ;
#1988 = PLANE('',#30408) ;
#1989 = PLANE('',#30411) ;
#1990 = PLANE('',#30414) ;
#1991 = PLANE('',#30417) ;
#1992 = PLANE('',#30420) ;
#1993 = PLANE('',#30423) ;
#1994 = PLANE('',#30438) ;
#1995 = PLANE('',#30440) ;
#1996 = PLANE('',#30443) ;
#1997 = PLANE('',#30445) ;
#1998 = PLANE('',#30447) ;
#1999 = PLANE('',#30449) ;
#2000 = PLANE('',#30451) ;
#2001 = PLANE('',#30452) ;
#2002 = PLANE('',#30453) ;
#2003 = PLANE('',#30454) ;
#2004 = PLANE('',#30455) ;
#2005 = PLANE('',#30456) ;
#2006 = PLANE('',#30457) ;
#2007 = PLANE('',#30458) ;
#2008 = PLANE('',#30459) ;
#2009 = PLANE('',#30460) ;
#2010 = PLANE('',#30461) ;
#2011 = PLANE('',#30462) ;
#2012 = PLANE('',#30475) ;
#2013 = PLANE('',#30477) ;
#2014 = PLANE('',#30478) ;
#2015 = PLANE('',#30479) ;
#2016 = PLANE('',#30480) ;
#2017 = PLANE('',#30481) ;
#2018 = PLANE('',#30483) ;
#2019 = PLANE('',#30485) ;
#2020 = PLANE('',#30491) ;
#2021 = PLANE('',#30492) ;
#2022 = PLANE('',#30493) ;
#2023 = PLANE('',#30494) ;
#2024 = PLANE('',#30495) ;
#2025 = PLANE('',#30496) ;
#2026 = PLANE('',#30497) ;
#2027 = PLANE('',#30498) ;
#2028 = PLANE('',#30499) ;
#2029 = PLANE('',#30503) ;
#2030 = PLANE('',#30504) ;
#2031 = PLANE('',#30508) ;
#2032 = PLANE('',#30516) ;
#2033 = PLANE('',#30517) ;
#2034 = PLANE('',#30519) ;
#2035 = PLANE('',#30522) ;
#2036 = PLANE('',#30523) ;
#2037 = PLANE('',#30524) ;
#2038 = PLANE('',#30531) ;
#2039 = PLANE('',#30532) ;
#2040 = PLANE('',#30533) ;
#2041 = PLANE('',#30534) ;
#2042 = PLANE('',#30535) ;
#2043 = PLANE('',#30536) ;
#2044 = PLANE('',#30537) ;
#2045 = PLANE('',#30538) ;
#2046 = PLANE('',#30543) ;
#2047 = PLANE('',#30544) ;
#2048 = PLANE('',#30549) ;
#2049 = PLANE('',#30556) ;
#2050 = PLANE('',#30557) ;
#2051 = PLANE('',#30565) ;
#2052 = PLANE('',#30566) ;
#2053 = PLANE('',#30573) ;
#2054 = PLANE('',#30574) ;
#2055 = PLANE('',#30578) ;
#2056 = PLANE('',#30579) ;
#2057 = PLANE('',#30581) ;
#2058 = PLANE('',#30584) ;
#2059 = PLANE('',#30610) ;
#2060 = PLANE('',#30611) ;
#2061 = PLANE('',#30612) ;
#2062 = PLANE('',#30613) ;
#2063 = PLANE('',#30614) ;
#2064 = PLANE('',#30615) ;
#2065 = PLANE('',#30616) ;
#2066 = PLANE('',#30617) ;
#2067 = PLANE('',#30618) ;
#2068 = PLANE('',#30619) ;
#2069 = PLANE('',#30620) ;
#2070 = PLANE('',#30621) ;
#2071 = PLANE('',#30622) ;
#2072 = PLANE('',#30623) ;
#2073 = PLANE('',#30624) ;
#2074 = PLANE('',#30625) ;
#2075 = PLANE('',#30626) ;
#2076 = PLANE('',#30627) ;
#2077 = PLANE('',#30628) ;
#2078 = PLANE('',#30629) ;
#2079 = PLANE('',#30630) ;
#2080 = PLANE('',#30631) ;
#2081 = PLANE('',#30632) ;
#2082 = PLANE('',#30633) ;
#2083 = PLANE('',#30634) ;
#2084 = PLANE('',#30635) ;
#2085 = PLANE('',#30636) ;
#2086 = PLANE('',#30637) ;
#2087 = PLANE('',#30638) ;
#2088 = PLANE('',#30639) ;
#2089 = PLANE('',#30640) ;
#2090 = PLANE('',#30641) ;
#2091 = PLANE('',#30642) ;
#2092 = PLANE('',#30643) ;
#2093 = PLANE('',#30644) ;
#2094 = PLANE('',#30645) ;
#2095 = PLANE('',#30646) ;
#2096 = PLANE('',#30647) ;
#2097 = PLANE('',#30648) ;
#2098 = PLANE('',#30649) ;
#2099 = PLANE('',#30652) ;
#2100 = PLANE('',#30653) ;
#2101 = PLANE('',#30661) ;
#2102 = PLANE('',#30662) ;
#2103 = PLANE('',#30678) ;
#2104 = PLANE('',#30679) ;
#2105 = PLANE('',#30680) ;
#2106 = PLANE('',#30681) ;
#2107 = PLANE('',#30682) ;
#2108 = PLANE('',#30683) ;
#2109 = PLANE('',#30684) ;
#2110 = PLANE('',#30688) ;
#2111 = PLANE('',#30689) ;
#2112 = PLANE('',#30690) ;
#2113 = PLANE('',#30691) ;
#2114 = PLANE('',#30692) ;
#2115 = PLANE('',#30710) ;
#2116 = PLANE('',#30714) ;
#2117 = PLANE('',#30715) ;
#2118 = PLANE('',#30717) ;
#2119 = PLANE('',#30718) ;
#2120 = PLANE('',#30719) ;
#2121 = PLANE('',#30720) ;
#2122 = PLANE('',#30721) ;
#2123 = PLANE('',#30722) ;
#2124 = PLANE('',#30723) ;
#2125 = PLANE('',#30724) ;
#2126 = PLANE('',#30727) ;
#2127 = PLANE('',#30730) ;
#2128 = PLANE('',#30731) ;
#2129 = PLANE('',#30732) ;
#2130 = PLANE('',#30733) ;
#2131 = PLANE('',#30735) ;
#2132 = PLANE('',#30736) ;
#2133 = PLANE('',#30737) ;
#2134 = PLANE('',#30738) ;
#2135 = PLANE('',#30739) ;
#2136 = PLANE('',#30740) ;
#2137 = PLANE('',#30741) ;
#2138 = PLANE('',#30745) ;
#2139 = PLANE('',#30746) ;
#2140 = PLANE('',#30747) ;
#2141 = PLANE('',#30748) ;
#2142 = PLANE('',#30749) ;
#2143 = PLANE('',#30753) ;
#2144 = PLANE('',#30754) ;
#2145 = PLANE('',#30755) ;
#2146 = PLANE('',#30756) ;
#2147 = PLANE('',#30757) ;
#2148 = PLANE('',#30761) ;
#2149 = PLANE('',#30762) ;
#2150 = PLANE('',#30763) ;
#2151 = PLANE('',#30764) ;
#2152 = PLANE('',#30766) ;
#2153 = PLANE('',#30767) ;
#2154 = PLANE('',#30768) ;
#2155 = PLANE('',#30769) ;
#2156 = PLANE('',#30770) ;
#2157 = PLANE('',#30771) ;
#2158 = PLANE('',#30772) ;
#2159 = PLANE('',#30773) ;
#2160 = PLANE('',#30774) ;
#2161 = PLANE('',#30775) ;
#2162 = PLANE('',#30776) ;
#2163 = PLANE('',#30777) ;
#2164 = PLANE('',#30778) ;
#2165 = PLANE('',#30779) ;
#2166 = PLANE('',#30780) ;
#2167 = PLANE('',#30781) ;
#2168 = PLANE('',#30782) ;
#2169 = PLANE('',#30783) ;
#2170 = PLANE('',#30784) ;
#2171 = PLANE('',#30785) ;
#2172 = PLANE('',#30786) ;
#2173 = PLANE('',#30787) ;
#2174 = PLANE('',#30788) ;
#2175 = PLANE('',#30789) ;
#2176 = PLANE('',#30790) ;
#2177 = PLANE('',#30791) ;
#2178 = PLANE('',#30792) ;
#2179 = PLANE('',#30793) ;
#2180 = PLANE('',#30794) ;
#2181 = PLANE('',#30795) ;
#2182 = PLANE('',#30796) ;
#2183 = PLANE('',#30797) ;
#2184 = PLANE('',#30798) ;
#2185 = PLANE('',#30799) ;
#2186 = PLANE('',#30800) ;
#2187 = PLANE('',#30801) ;
#2188 = PLANE('',#30802) ;
#2189 = PLANE('',#30803) ;
#2190 = PLANE('',#30804) ;
#2191 = PLANE('',#30805) ;
#2192 = PLANE('',#30806) ;
#2193 = PLANE('',#30807) ;
#2194 = PLANE('',#30824) ;
#2195 = PLANE('',#30833) ;
#2196 = PLANE('',#30834) ;
#2197 = PLANE('',#30835) ;
#2198 = PLANE('',#30836) ;
#2199 = PLANE('',#30837) ;
#2200 = PLANE('',#30840) ;
#2201 = PLANE('',#30850) ;
#2202 = PLANE('',#30851) ;
#2203 = PLANE('',#30852) ;
#2204 = PLANE('',#30855) ;
#2205 = PLANE('',#30885) ;
#2206 = PLANE('',#30886) ;
#2207 = PLANE('',#30888) ;
#2208 = PLANE('',#30896) ;
#2209 = PLANE('',#30897) ;
#2210 = PLANE('',#30898) ;
#2211 = PLANE('',#30902) ;
#2212 = PLANE('',#30904) ;
#2213 = PLANE('',#30910) ;
#2214 = PLANE('',#30911) ;
#2215 = PLANE('',#30912) ;
#2216 = PLANE('',#30913) ;
#2217 = PLANE('',#30914) ;
#2218 = PLANE('',#30915) ;
#2219 = PLANE('',#30916) ;
#2220 = PLANE('',#30917) ;
#2221 = PLANE('',#30918) ;
#2222 = PLANE('',#30919) ;
#2223 = PLANE('',#30920) ;
#2224 = PLANE('',#30921) ;
#2225 = PLANE('',#30922) ;
#2226 = PLANE('',#30923) ;
#2227 = PLANE('',#30924) ;
#2228 = PLANE('',#30929) ;
#2229 = PLANE('',#30933) ;
#2230 = PLANE('',#30938) ;
#2231 = PLANE('',#30941) ;
#2232 = PLANE('',#30979) ;
#2233 = PLANE('',#30997) ;
#2234 = PLANE('',#31044) ;
#2235 = PLANE('',#31045) ;
#2236 = PLANE('',#31046) ;
#2237 = PLANE('',#31051) ;
#2238 = PLANE('',#31055) ;
#2239 = PLANE('',#31056) ;
#2240 = PLANE('',#31061) ;
#2241 = PLANE('',#31062) ;
#2242 = PLANE('',#31067) ;
#2243 = PLANE('',#31068) ;
#2244 = PLANE('',#31076) ;
#2245 = PLANE('',#31077) ;
#2246 = PLANE('',#31080) ;
#2247 = PLANE('',#31087) ;
#2248 = PLANE('',#31088) ;
#2249 = PLANE('',#31096) ;
#2250 = PLANE('',#31102) ;
#2251 = PLANE('',#31103) ;
#2252 = PLANE('',#32055) ;
#2253 = PLANE('',#32062) ;
#2254 = PLANE('',#32063) ;
#2255 = PLANE('',#32066) ;
#2256 = PLANE('',#32091) ;
#2257 = PLANE('',#32100) ;
#2258 = PLANE('',#32122) ;
#2259 = PLANE('',#32123) ;
#2260 = PLANE('',#32124) ;
#2261 = PLANE('',#32125) ;
#2262 = PLANE('',#32126) ;
#2263 = PLANE('',#32127) ;
#2264 = PLANE('',#32128) ;
#2265 = PLANE('',#32129) ;
#2266 = PLANE('',#32130) ;
#2267 = PLANE('',#32132) ;
#2268 = PLANE('',#32136) ;
#2269 = PLANE('',#32139) ;
#2270 = PLANE('',#32144) ;
#2271 = PLANE('',#32145) ;
#2272 = PLANE('',#32149) ;
#2273 = PLANE('',#32152) ;
#2274 = PLANE('',#32164) ;
#2275 = PLANE('',#32165) ;
#2276 = PLANE('',#32170) ;
#2277 = PLANE('',#32171) ;
#2278 = PLANE('',#32172) ;
#2279 = PLANE('',#32173) ;
#2280 = PLANE('',#32174) ;
#2281 = PLANE('',#32175) ;
#2282 = PLANE('',#32176) ;
#2283 = PLANE('',#32177) ;
#2284 = PLANE('',#32178) ;
#2285 = PLANE('',#32179) ;
#2286 = PLANE('',#32180) ;
#2287 = PLANE('',#32181) ;
#2288 = PLANE('',#32182) ;
#2289 = PLANE('',#32184) ;
#2290 = PLANE('',#32185) ;
#2291 = PLANE('',#32187) ;
#2292 = PLANE('',#32188) ;
#2293 = PLANE('',#32189) ;
#2294 = PLANE('',#32190) ;
#2295 = PLANE('',#32191) ;
#2296 = PLANE('',#32199) ;
#2297 = PLANE('',#32211) ;
#2298 = PLANE('',#32212) ;
#2299 = PLANE('',#32213) ;
#2300 = PLANE('',#32214) ;
#2301 = PLANE('',#32215) ;
#2302 = PLANE('',#32216) ;
#2303 = PLANE('',#32217) ;
#2304 = PLANE('',#32218) ;
#2305 = PLANE('',#32219) ;
#2306 = PLANE('',#32224) ;
#2307 = PLANE('',#32225) ;
#2308 = PLANE('',#32226) ;
#2309 = PLANE('',#32227) ;
#2310 = PLANE('',#32228) ;
#2311 = PLANE('',#32229) ;
#2312 = PLANE('',#32230) ;
#2313 = PLANE('',#32231) ;
#2314 = PLANE('',#32236) ;
#2315 = PLANE('',#32237) ;
#2316 = PLANE('',#32238) ;
#2317 = PLANE('',#32239) ;
#2318 = PLANE('',#32240) ;
#2319 = PLANE('',#32241) ;
#2320 = PLANE('',#32242) ;
#2321 = PLANE('',#32243) ;
#2322 = PLANE('',#32244) ;
#2323 = PLANE('',#32249) ;
#2324 = PLANE('',#32250) ;
#2325 = PLANE('',#32251) ;
#2326 = PLANE('',#32252) ;
#2327 = PLANE('',#32253) ;
#2328 = PLANE('',#32254) ;
#2329 = PLANE('',#32255) ;
#2330 = PLANE('',#32256) ;
#2331 = PLANE('',#32258) ;
#2332 = PLANE('',#32263) ;
#2333 = PLANE('',#32266) ;
#2334 = PLANE('',#32268) ;
#2335 = PLANE('',#32273) ;
#2336 = PLANE('',#32276) ;
#2337 = PLANE('',#32358) ;
#2338 = PLANE('',#32363) ;
#2339 = PLANE('',#32364) ;
#2340 = FACE_OUTER_BOUND('',#3894,.T.) ;
#2341 = FACE_OUTER_BOUND('',#3895,.T.) ;
#2342 = FACE_OUTER_BOUND('',#3897,.T.) ;
#2343 = FACE_OUTER_BOUND('',#3898,.T.) ;
#2344 = FACE_OUTER_BOUND('',#3899,.T.) ;
#2345 = FACE_OUTER_BOUND('',#3900,.T.) ;
#2346 = FACE_OUTER_BOUND('',#3901,.T.) ;
#2347 = FACE_OUTER_BOUND('',#3902,.T.) ;
#2348 = FACE_OUTER_BOUND('',#3904,.T.) ;
#2349 = FACE_OUTER_BOUND('',#3905,.T.) ;
#2350 = FACE_OUTER_BOUND('',#3906,.T.) ;
#2351 = FACE_OUTER_BOUND('',#3907,.T.) ;
#2352 = FACE_OUTER_BOUND('',#3909,.T.) ;
#2353 = FACE_OUTER_BOUND('',#3910,.T.) ;
#2354 = FACE_OUTER_BOUND('',#3911,.T.) ;
#2355 = FACE_OUTER_BOUND('',#3912,.T.) ;
#2356 = FACE_OUTER_BOUND('',#3913,.T.) ;
#2357 = FACE_OUTER_BOUND('',#3914,.T.) ;
#2358 = FACE_OUTER_BOUND('',#3916,.T.) ;
#2359 = FACE_OUTER_BOUND('',#3917,.T.) ;
#2360 = FACE_OUTER_BOUND('',#3918,.T.) ;
#2361 = FACE_OUTER_BOUND('',#3919,.T.) ;
#2362 = FACE_OUTER_BOUND('',#3920,.T.) ;
#2363 = FACE_OUTER_BOUND('',#3921,.T.) ;
#2364 = FACE_OUTER_BOUND('',#3922,.T.) ;
#2365 = FACE_OUTER_BOUND('',#3923,.T.) ;
#2366 = FACE_OUTER_BOUND('',#3924,.T.) ;
#2367 = FACE_OUTER_BOUND('',#3925,.T.) ;
#2368 = FACE_OUTER_BOUND('',#3926,.T.) ;
#2369 = FACE_OUTER_BOUND('',#3927,.T.) ;
#2370 = FACE_OUTER_BOUND('',#3928,.T.) ;
#2371 = FACE_OUTER_BOUND('',#3929,.T.) ;
#2372 = FACE_OUTER_BOUND('',#3930,.T.) ;
#2373 = FACE_OUTER_BOUND('',#3931,.T.) ;
#2374 = FACE_OUTER_BOUND('',#3932,.T.) ;
#2375 = FACE_OUTER_BOUND('',#3933,.T.) ;
#2376 = FACE_OUTER_BOUND('',#3934,.T.) ;
#2377 = FACE_OUTER_BOUND('',#3935,.T.) ;
#2378 = FACE_OUTER_BOUND('',#3936,.T.) ;
#2379 = FACE_OUTER_BOUND('',#3937,.T.) ;
#2380 = FACE_OUTER_BOUND('',#3938,.T.) ;
#2381 = FACE_OUTER_BOUND('',#3939,.T.) ;
#2382 = FACE_OUTER_BOUND('',#3940,.T.) ;
#2383 = FACE_OUTER_BOUND('',#3941,.T.) ;
#2384 = FACE_OUTER_BOUND('',#3942,.T.) ;
#2385 = FACE_OUTER_BOUND('',#3943,.T.) ;
#2386 = FACE_OUTER_BOUND('',#3944,.T.) ;
#2387 = FACE_OUTER_BOUND('',#3945,.T.) ;
#2388 = FACE_OUTER_BOUND('',#3946,.T.) ;
#2389 = FACE_OUTER_BOUND('',#3947,.T.) ;
#2390 = FACE_OUTER_BOUND('',#3948,.T.) ;
#2391 = FACE_OUTER_BOUND('',#3949,.T.) ;
#2392 = FACE_OUTER_BOUND('',#3950,.T.) ;
#2393 = FACE_OUTER_BOUND('',#3951,.T.) ;
#2394 = FACE_OUTER_BOUND('',#3952,.T.) ;
#2395 = FACE_OUTER_BOUND('',#3953,.T.) ;
#2396 = FACE_OUTER_BOUND('',#3954,.T.) ;
#2397 = FACE_OUTER_BOUND('',#3955,.T.) ;
#2398 = FACE_OUTER_BOUND('',#3956,.T.) ;
#2399 = FACE_OUTER_BOUND('',#3957,.T.) ;
#2400 = FACE_OUTER_BOUND('',#3958,.T.) ;
#2401 = FACE_OUTER_BOUND('',#3959,.T.) ;
#2402 = FACE_OUTER_BOUND('',#3961,.T.) ;
#2403 = FACE_OUTER_BOUND('',#3963,.T.) ;
#2404 = FACE_OUTER_BOUND('',#3968,.T.) ;
#2405 = FACE_OUTER_BOUND('',#3973,.T.) ;
#2406 = FACE_OUTER_BOUND('',#3975,.T.) ;
#2407 = FACE_OUTER_BOUND('',#3976,.T.) ;
#2408 = FACE_OUTER_BOUND('',#3977,.T.) ;
#2409 = FACE_OUTER_BOUND('',#3978,.T.) ;
#2410 = FACE_OUTER_BOUND('',#3979,.T.) ;
#2411 = FACE_OUTER_BOUND('',#3980,.T.) ;
#2412 = FACE_OUTER_BOUND('',#3981,.T.) ;
#2413 = FACE_OUTER_BOUND('',#3982,.T.) ;
#2414 = FACE_OUTER_BOUND('',#3983,.T.) ;
#2415 = FACE_OUTER_BOUND('',#3984,.T.) ;
#2416 = FACE_OUTER_BOUND('',#3986,.T.) ;
#2417 = FACE_OUTER_BOUND('',#3987,.T.) ;
#2418 = FACE_OUTER_BOUND('',#3988,.T.) ;
#2419 = FACE_OUTER_BOUND('',#3991,.T.) ;
#2420 = FACE_OUTER_BOUND('',#3992,.T.) ;
#2421 = FACE_OUTER_BOUND('',#3993,.T.) ;
#2422 = FACE_OUTER_BOUND('',#3994,.T.) ;
#2423 = FACE_OUTER_BOUND('',#3995,.T.) ;
#2424 = FACE_OUTER_BOUND('',#3996,.T.) ;
#2425 = FACE_OUTER_BOUND('',#3997,.T.) ;
#2426 = FACE_OUTER_BOUND('',#3998,.T.) ;
#2427 = FACE_OUTER_BOUND('',#3999,.T.) ;
#2428 = FACE_OUTER_BOUND('',#4000,.T.) ;
#2429 = FACE_OUTER_BOUND('',#4001,.T.) ;
#2430 = FACE_OUTER_BOUND('',#4002,.T.) ;
#2431 = FACE_OUTER_BOUND('',#4003,.T.) ;
#2432 = FACE_OUTER_BOUND('',#4004,.T.) ;
#2433 = FACE_OUTER_BOUND('',#4005,.T.) ;
#2434 = FACE_OUTER_BOUND('',#4006,.T.) ;
#2435 = FACE_OUTER_BOUND('',#4007,.T.) ;
#2436 = FACE_OUTER_BOUND('',#4008,.T.) ;
#2437 = FACE_OUTER_BOUND('',#4009,.T.) ;
#2438 = FACE_OUTER_BOUND('',#4010,.T.) ;
#2439 = FACE_OUTER_BOUND('',#4011,.T.) ;
#2440 = FACE_OUTER_BOUND('',#4012,.T.) ;
#2441 = FACE_OUTER_BOUND('',#4013,.T.) ;
#2442 = FACE_OUTER_BOUND('',#4014,.T.) ;
#2443 = FACE_OUTER_BOUND('',#4015,.T.) ;
#2444 = FACE_OUTER_BOUND('',#4016,.T.) ;
#2445 = FACE_OUTER_BOUND('',#4017,.T.) ;
#2446 = FACE_OUTER_BOUND('',#4018,.T.) ;
#2447 = FACE_OUTER_BOUND('',#4019,.T.) ;
#2448 = FACE_OUTER_BOUND('',#4020,.T.) ;
#2449 = FACE_OUTER_BOUND('',#4021,.T.) ;
#2450 = FACE_OUTER_BOUND('',#4022,.T.) ;
#2451 = FACE_OUTER_BOUND('',#4075,.T.) ;
#2452 = FACE_OUTER_BOUND('',#4076,.T.) ;
#2453 = FACE_OUTER_BOUND('',#4129,.T.) ;
#2454 = FACE_OUTER_BOUND('',#4130,.T.) ;
#2455 = FACE_OUTER_BOUND('',#4131,.T.) ;
#2456 = FACE_OUTER_BOUND('',#4132,.T.) ;
#2457 = FACE_OUTER_BOUND('',#4133,.T.) ;
#2458 = FACE_OUTER_BOUND('',#4134,.T.) ;
#2459 = FACE_OUTER_BOUND('',#4135,.T.) ;
#2460 = FACE_OUTER_BOUND('',#4136,.T.) ;
#2461 = FACE_OUTER_BOUND('',#4137,.T.) ;
#2462 = FACE_OUTER_BOUND('',#4138,.T.) ;
#2463 = FACE_OUTER_BOUND('',#4139,.T.) ;
#2464 = FACE_OUTER_BOUND('',#4140,.T.) ;
#2465 = FACE_OUTER_BOUND('',#4141,.T.) ;
#2466 = FACE_OUTER_BOUND('',#4142,.T.) ;
#2467 = FACE_OUTER_BOUND('',#4143,.T.) ;
#2468 = FACE_OUTER_BOUND('',#4144,.T.) ;
#2469 = FACE_OUTER_BOUND('',#4145,.T.) ;
#2470 = FACE_OUTER_BOUND('',#4146,.T.) ;
#2471 = FACE_OUTER_BOUND('',#4147,.T.) ;
#2472 = FACE_OUTER_BOUND('',#4148,.T.) ;
#2473 = FACE_OUTER_BOUND('',#4149,.T.) ;
#2474 = FACE_OUTER_BOUND('',#4150,.T.) ;
#2475 = FACE_OUTER_BOUND('',#4151,.T.) ;
#2476 = FACE_OUTER_BOUND('',#4152,.T.) ;
#2477 = FACE_OUTER_BOUND('',#4153,.T.) ;
#2478 = FACE_OUTER_BOUND('',#4154,.T.) ;
#2479 = FACE_OUTER_BOUND('',#4155,.T.) ;
#2480 = FACE_OUTER_BOUND('',#4156,.T.) ;
#2481 = FACE_OUTER_BOUND('',#4157,.T.) ;
#2482 = FACE_OUTER_BOUND('',#4158,.T.) ;
#2483 = FACE_OUTER_BOUND('',#4159,.T.) ;
#2484 = FACE_OUTER_BOUND('',#4160,.T.) ;
#2485 = FACE_OUTER_BOUND('',#4161,.T.) ;
#2486 = FACE_OUTER_BOUND('',#4162,.T.) ;
#2487 = FACE_OUTER_BOUND('',#4163,.T.) ;
#2488 = FACE_OUTER_BOUND('',#4164,.T.) ;
#2489 = FACE_OUTER_BOUND('',#4165,.T.) ;
#2490 = FACE_OUTER_BOUND('',#4166,.T.) ;
#2491 = FACE_OUTER_BOUND('',#4167,.T.) ;
#2492 = FACE_OUTER_BOUND('',#4168,.T.) ;
#2493 = FACE_OUTER_BOUND('',#4169,.T.) ;
#2494 = FACE_OUTER_BOUND('',#4170,.T.) ;
#2495 = FACE_OUTER_BOUND('',#4171,.T.) ;
#2496 = FACE_OUTER_BOUND('',#4172,.T.) ;
#2497 = FACE_OUTER_BOUND('',#4173,.T.) ;
#2498 = FACE_OUTER_BOUND('',#4174,.T.) ;
#2499 = FACE_OUTER_BOUND('',#4175,.T.) ;
#2500 = FACE_OUTER_BOUND('',#4176,.T.) ;
#2501 = FACE_OUTER_BOUND('',#4177,.T.) ;
#2502 = FACE_OUTER_BOUND('',#4178,.T.) ;
#2503 = FACE_OUTER_BOUND('',#4179,.T.) ;
#2504 = FACE_OUTER_BOUND('',#4180,.T.) ;
#2505 = FACE_OUTER_BOUND('',#4181,.T.) ;
#2506 = FACE_OUTER_BOUND('',#4182,.T.) ;
#2507 = FACE_OUTER_BOUND('',#4183,.T.) ;
#2508 = FACE_OUTER_BOUND('',#4184,.T.) ;
#2509 = FACE_OUTER_BOUND('',#4185,.T.) ;
#2510 = FACE_OUTER_BOUND('',#4186,.T.) ;
#2511 = FACE_OUTER_BOUND('',#4187,.T.) ;
#2512 = FACE_OUTER_BOUND('',#4188,.T.) ;
#2513 = FACE_OUTER_BOUND('',#4189,.T.) ;
#2514 = FACE_OUTER_BOUND('',#4190,.T.) ;
#2515 = FACE_OUTER_BOUND('',#4191,.T.) ;
#2516 = FACE_OUTER_BOUND('',#4192,.T.) ;
#2517 = FACE_OUTER_BOUND('',#4193,.T.) ;
#2518 = FACE_OUTER_BOUND('',#4194,.T.) ;
#2519 = FACE_OUTER_BOUND('',#4195,.T.) ;
#2520 = FACE_OUTER_BOUND('',#4196,.T.) ;
#2521 = FACE_OUTER_BOUND('',#4197,.T.) ;
#2522 = FACE_OUTER_BOUND('',#4198,.T.) ;
#2523 = FACE_OUTER_BOUND('',#4199,.T.) ;
#2524 = FACE_OUTER_BOUND('',#4200,.T.) ;
#2525 = FACE_OUTER_BOUND('',#4201,.T.) ;
#2526 = FACE_OUTER_BOUND('',#4202,.T.) ;
#2527 = FACE_OUTER_BOUND('',#4203,.T.) ;
#2528 = FACE_OUTER_BOUND('',#4204,.T.) ;
#2529 = FACE_OUTER_BOUND('',#4205,.T.) ;
#2530 = FACE_OUTER_BOUND('',#4206,.T.) ;
#2531 = FACE_OUTER_BOUND('',#4207,.T.) ;
#2532 = FACE_OUTER_BOUND('',#4208,.T.) ;
#2533 = FACE_OUTER_BOUND('',#4209,.T.) ;
#2534 = FACE_OUTER_BOUND('',#4210,.T.) ;
#2535 = FACE_OUTER_BOUND('',#4211,.T.) ;
#2536 = FACE_OUTER_BOUND('',#4212,.T.) ;
#2537 = FACE_OUTER_BOUND('',#4213,.T.) ;
#2538 = FACE_OUTER_BOUND('',#4214,.T.) ;
#2539 = FACE_OUTER_BOUND('',#4215,.T.) ;
#2540 = FACE_OUTER_BOUND('',#4216,.T.) ;
#2541 = FACE_OUTER_BOUND('',#4217,.T.) ;
#2542 = FACE_OUTER_BOUND('',#4218,.T.) ;
#2543 = FACE_OUTER_BOUND('',#4219,.T.) ;
#2544 = FACE_OUTER_BOUND('',#4220,.T.) ;
#2545 = FACE_OUTER_BOUND('',#4221,.T.) ;
#2546 = FACE_OUTER_BOUND('',#4222,.T.) ;
#2547 = FACE_OUTER_BOUND('',#4223,.T.) ;
#2548 = FACE_OUTER_BOUND('',#4224,.T.) ;
#2549 = FACE_OUTER_BOUND('',#4225,.T.) ;
#2550 = FACE_OUTER_BOUND('',#4226,.T.) ;
#2551 = FACE_OUTER_BOUND('',#4227,.T.) ;
#2552 = FACE_OUTER_BOUND('',#4228,.T.) ;
#2553 = FACE_OUTER_BOUND('',#4229,.T.) ;
#2554 = FACE_OUTER_BOUND('',#4230,.T.) ;
#2555 = FACE_OUTER_BOUND('',#4231,.T.) ;
#2556 = FACE_OUTER_BOUND('',#4232,.T.) ;
#2557 = FACE_OUTER_BOUND('',#4233,.T.) ;
#2558 = FACE_OUTER_BOUND('',#4234,.T.) ;
#2559 = FACE_OUTER_BOUND('',#4235,.T.) ;
#2560 = FACE_OUTER_BOUND('',#4236,.T.) ;
#2561 = FACE_OUTER_BOUND('',#4237,.T.) ;
#2562 = FACE_OUTER_BOUND('',#4238,.T.) ;
#2563 = FACE_OUTER_BOUND('',#4239,.T.) ;
#2564 = FACE_OUTER_BOUND('',#4240,.T.) ;
#2565 = FACE_OUTER_BOUND('',#4241,.T.) ;
#2566 = FACE_OUTER_BOUND('',#4242,.T.) ;
#2567 = FACE_OUTER_BOUND('',#4243,.T.) ;
#2568 = FACE_OUTER_BOUND('',#4244,.T.) ;
#2569 = FACE_OUTER_BOUND('',#4245,.T.) ;
#2570 = FACE_OUTER_BOUND('',#4246,.T.) ;
#2571 = FACE_OUTER_BOUND('',#4247,.T.) ;
#2572 = FACE_OUTER_BOUND('',#4248,.T.) ;
#2573 = FACE_OUTER_BOUND('',#4249,.T.) ;
#2574 = FACE_OUTER_BOUND('',#4250,.T.) ;
#2575 = FACE_OUTER_BOUND('',#4251,.T.) ;
#2576 = FACE_OUTER_BOUND('',#4252,.T.) ;
#2577 = FACE_OUTER_BOUND('',#4253,.T.) ;
#2578 = FACE_OUTER_BOUND('',#4254,.T.) ;
#2579 = FACE_OUTER_BOUND('',#4255,.T.) ;
#2580 = FACE_OUTER_BOUND('',#4256,.T.) ;
#2581 = FACE_OUTER_BOUND('',#4257,.T.) ;
#2582 = FACE_OUTER_BOUND('',#4258,.T.) ;
#2583 = FACE_OUTER_BOUND('',#4259,.T.) ;
#2584 = FACE_OUTER_BOUND('',#4260,.T.) ;
#2585 = FACE_OUTER_BOUND('',#4261,.T.) ;
#2586 = FACE_OUTER_BOUND('',#4262,.T.) ;
#2587 = FACE_OUTER_BOUND('',#4263,.T.) ;
#2588 = FACE_OUTER_BOUND('',#4264,.T.) ;
#2589 = FACE_OUTER_BOUND('',#4265,.T.) ;
#2590 = FACE_OUTER_BOUND('',#4266,.T.) ;
#2591 = FACE_OUTER_BOUND('',#4267,.T.) ;
#2592 = FACE_OUTER_BOUND('',#4268,.T.) ;
#2593 = FACE_OUTER_BOUND('',#4269,.T.) ;
#2594 = FACE_OUTER_BOUND('',#4270,.T.) ;
#2595 = FACE_OUTER_BOUND('',#4271,.T.) ;
#2596 = FACE_OUTER_BOUND('',#4272,.T.) ;
#2597 = FACE_OUTER_BOUND('',#4273,.T.) ;
#2598 = FACE_OUTER_BOUND('',#4274,.T.) ;
#2599 = FACE_OUTER_BOUND('',#4275,.T.) ;
#2600 = FACE_OUTER_BOUND('',#4276,.T.) ;
#2601 = FACE_OUTER_BOUND('',#4277,.T.) ;
#2602 = FACE_OUTER_BOUND('',#4278,.T.) ;
#2603 = FACE_OUTER_BOUND('',#4279,.T.) ;
#2604 = FACE_OUTER_BOUND('',#4280,.T.) ;
#2605 = FACE_OUTER_BOUND('',#4281,.T.) ;
#2606 = FACE_OUTER_BOUND('',#4282,.T.) ;
#2607 = FACE_OUTER_BOUND('',#4283,.T.) ;
#2608 = FACE_OUTER_BOUND('',#4284,.T.) ;
#2609 = FACE_OUTER_BOUND('',#4285,.T.) ;
#2610 = FACE_OUTER_BOUND('',#4286,.T.) ;
#2611 = FACE_OUTER_BOUND('',#4287,.T.) ;
#2612 = FACE_OUTER_BOUND('',#4288,.T.) ;
#2613 = FACE_OUTER_BOUND('',#4289,.T.) ;
#2614 = FACE_OUTER_BOUND('',#4290,.T.) ;
#2615 = FACE_OUTER_BOUND('',#4291,.T.) ;
#2616 = FACE_OUTER_BOUND('',#4292,.T.) ;
#2617 = FACE_OUTER_BOUND('',#4293,.T.) ;
#2618 = FACE_OUTER_BOUND('',#4294,.T.) ;
#2619 = FACE_OUTER_BOUND('',#4295,.T.) ;
#2620 = FACE_OUTER_BOUND('',#4296,.T.) ;
#2621 = FACE_OUTER_BOUND('',#4297,.T.) ;
#2622 = FACE_OUTER_BOUND('',#4298,.T.) ;
#2623 = FACE_OUTER_BOUND('',#4299,.T.) ;
#2624 = FACE_OUTER_BOUND('',#4300,.T.) ;
#2625 = FACE_OUTER_BOUND('',#4301,.T.) ;
#2626 = FACE_OUTER_BOUND('',#4302,.T.) ;
#2627 = FACE_OUTER_BOUND('',#4303,.T.) ;
#2628 = FACE_OUTER_BOUND('',#4304,.T.) ;
#2629 = FACE_OUTER_BOUND('',#4305,.T.) ;
#2630 = FACE_OUTER_BOUND('',#4306,.T.) ;
#2631 = FACE_OUTER_BOUND('',#4307,.T.) ;
#2632 = FACE_OUTER_BOUND('',#4308,.T.) ;
#2633 = FACE_OUTER_BOUND('',#4309,.T.) ;
#2634 = FACE_OUTER_BOUND('',#4310,.T.) ;
#2635 = FACE_OUTER_BOUND('',#4311,.T.) ;
#2636 = FACE_OUTER_BOUND('',#4312,.T.) ;
#2637 = FACE_OUTER_BOUND('',#4313,.T.) ;
#2638 = FACE_OUTER_BOUND('',#4314,.T.) ;
#2639 = FACE_OUTER_BOUND('',#4315,.T.) ;
#2640 = FACE_OUTER_BOUND('',#4316,.T.) ;
#2641 = FACE_OUTER_BOUND('',#4317,.T.) ;
#2642 = FACE_OUTER_BOUND('',#4318,.T.) ;
#2643 = FACE_OUTER_BOUND('',#4319,.T.) ;
#2644 = FACE_OUTER_BOUND('',#4320,.T.) ;
#2645 = FACE_OUTER_BOUND('',#4321,.T.) ;
#2646 = FACE_OUTER_BOUND('',#4322,.T.) ;
#2647 = FACE_OUTER_BOUND('',#4323,.T.) ;
#2648 = FACE_OUTER_BOUND('',#4324,.T.) ;
#2649 = FACE_OUTER_BOUND('',#4325,.T.) ;
#2650 = FACE_OUTER_BOUND('',#4326,.T.) ;
#2651 = FACE_OUTER_BOUND('',#4327,.T.) ;
#2652 = FACE_OUTER_BOUND('',#4328,.T.) ;
#2653 = FACE_OUTER_BOUND('',#4329,.T.) ;
#2654 = FACE_OUTER_BOUND('',#4330,.T.) ;
#2655 = FACE_OUTER_BOUND('',#4331,.T.) ;
#2656 = FACE_OUTER_BOUND('',#4332,.T.) ;
#2657 = FACE_OUTER_BOUND('',#4333,.T.) ;
#2658 = FACE_OUTER_BOUND('',#4334,.T.) ;
#2659 = FACE_OUTER_BOUND('',#4335,.T.) ;
#2660 = FACE_OUTER_BOUND('',#4336,.T.) ;
#2661 = FACE_OUTER_BOUND('',#4337,.T.) ;
#2662 = FACE_OUTER_BOUND('',#4338,.T.) ;
#2663 = FACE_OUTER_BOUND('',#4339,.T.) ;
#2664 = FACE_OUTER_BOUND('',#4340,.T.) ;
#2665 = FACE_OUTER_BOUND('',#4341,.T.) ;
#2666 = FACE_OUTER_BOUND('',#4342,.T.) ;
#2667 = FACE_OUTER_BOUND('',#4343,.T.) ;
#2668 = FACE_OUTER_BOUND('',#4344,.T.) ;
#2669 = FACE_OUTER_BOUND('',#4345,.T.) ;
#2670 = FACE_OUTER_BOUND('',#4346,.T.) ;
#2671 = FACE_OUTER_BOUND('',#4347,.T.) ;
#2672 = FACE_OUTER_BOUND('',#4348,.T.) ;
#2673 = FACE_OUTER_BOUND('',#4349,.T.) ;
#2674 = FACE_OUTER_BOUND('',#4350,.T.) ;
#2675 = FACE_OUTER_BOUND('',#4351,.T.) ;
#2676 = FACE_OUTER_BOUND('',#4352,.T.) ;
#2677 = FACE_OUTER_BOUND('',#4353,.T.) ;
#2678 = FACE_OUTER_BOUND('',#4354,.T.) ;
#2679 = FACE_OUTER_BOUND('',#4355,.T.) ;
#2680 = FACE_OUTER_BOUND('',#4356,.T.) ;
#2681 = FACE_OUTER_BOUND('',#4357,.T.) ;
#2682 = FACE_OUTER_BOUND('',#4358,.T.) ;
#2683 = FACE_OUTER_BOUND('',#4359,.T.) ;
#2684 = FACE_OUTER_BOUND('',#4360,.T.) ;
#2685 = FACE_OUTER_BOUND('',#4361,.T.) ;
#2686 = FACE_OUTER_BOUND('',#4362,.T.) ;
#2687 = FACE_OUTER_BOUND('',#4363,.T.) ;
#2688 = FACE_OUTER_BOUND('',#4364,.T.) ;
#2689 = FACE_OUTER_BOUND('',#4365,.T.) ;
#2690 = FACE_OUTER_BOUND('',#4366,.T.) ;
#2691 = FACE_OUTER_BOUND('',#4367,.T.) ;
#2692 = FACE_OUTER_BOUND('',#4368,.T.) ;
#2693 = FACE_OUTER_BOUND('',#4369,.T.) ;
#2694 = FACE_OUTER_BOUND('',#4370,.T.) ;
#2695 = FACE_OUTER_BOUND('',#4371,.T.) ;
#2696 = FACE_OUTER_BOUND('',#4372,.T.) ;
#2697 = FACE_OUTER_BOUND('',#4373,.T.) ;
#2698 = FACE_OUTER_BOUND('',#4374,.T.) ;
#2699 = FACE_OUTER_BOUND('',#4375,.T.) ;
#2700 = FACE_OUTER_BOUND('',#4376,.T.) ;
#2701 = FACE_OUTER_BOUND('',#4377,.T.) ;
#2702 = FACE_OUTER_BOUND('',#4378,.T.) ;
#2703 = FACE_OUTER_BOUND('',#4379,.T.) ;
#2704 = FACE_OUTER_BOUND('',#4380,.T.) ;
#2705 = FACE_OUTER_BOUND('',#4381,.T.) ;
#2706 = FACE_OUTER_BOUND('',#4382,.T.) ;
#2707 = FACE_OUTER_BOUND('',#4383,.T.) ;
#2708 = FACE_OUTER_BOUND('',#4384,.T.) ;
#2709 = FACE_OUTER_BOUND('',#4385,.T.) ;
#2710 = FACE_OUTER_BOUND('',#4386,.T.) ;
#2711 = FACE_OUTER_BOUND('',#4387,.T.) ;
#2712 = FACE_OUTER_BOUND('',#4388,.T.) ;
#2713 = FACE_OUTER_BOUND('',#4389,.T.) ;
#2714 = FACE_OUTER_BOUND('',#4390,.T.) ;
#2715 = FACE_OUTER_BOUND('',#4391,.T.) ;
#2716 = FACE_OUTER_BOUND('',#4392,.T.) ;
#2717 = FACE_OUTER_BOUND('',#4393,.T.) ;
#2718 = FACE_OUTER_BOUND('',#4394,.T.) ;
#2719 = FACE_OUTER_BOUND('',#4395,.T.) ;
#2720 = FACE_OUTER_BOUND('',#4396,.T.) ;
#2721 = FACE_OUTER_BOUND('',#4397,.T.) ;
#2722 = FACE_OUTER_BOUND('',#4398,.T.) ;
#2723 = FACE_OUTER_BOUND('',#4399,.T.) ;
#2724 = FACE_OUTER_BOUND('',#4400,.T.) ;
#2725 = FACE_OUTER_BOUND('',#4401,.T.) ;
#2726 = FACE_OUTER_BOUND('',#4402,.T.) ;
#2727 = FACE_OUTER_BOUND('',#4403,.T.) ;
#2728 = FACE_OUTER_BOUND('',#4404,.T.) ;
#2729 = FACE_OUTER_BOUND('',#4405,.T.) ;
#2730 = FACE_OUTER_BOUND('',#4406,.T.) ;
#2731 = FACE_OUTER_BOUND('',#4407,.T.) ;
#2732 = FACE_OUTER_BOUND('',#4408,.T.) ;
#2733 = FACE_OUTER_BOUND('',#4409,.T.) ;
#2734 = FACE_OUTER_BOUND('',#4410,.T.) ;
#2735 = FACE_OUTER_BOUND('',#4411,.T.) ;
#2736 = FACE_OUTER_BOUND('',#4412,.T.) ;
#2737 = FACE_OUTER_BOUND('',#4413,.T.) ;
#2738 = FACE_OUTER_BOUND('',#4414,.T.) ;
#2739 = FACE_OUTER_BOUND('',#4415,.T.) ;
#2740 = FACE_OUTER_BOUND('',#4416,.T.) ;
#2741 = FACE_OUTER_BOUND('',#4417,.T.) ;
#2742 = FACE_OUTER_BOUND('',#4418,.T.) ;
#2743 = FACE_OUTER_BOUND('',#4419,.T.) ;
#2744 = FACE_OUTER_BOUND('',#4420,.T.) ;
#2745 = FACE_OUTER_BOUND('',#4421,.T.) ;
#2746 = FACE_OUTER_BOUND('',#4422,.T.) ;
#2747 = FACE_OUTER_BOUND('',#4423,.T.) ;
#2748 = FACE_OUTER_BOUND('',#4424,.T.) ;
#2749 = FACE_OUTER_BOUND('',#4425,.T.) ;
#2750 = FACE_OUTER_BOUND('',#4426,.T.) ;
#2751 = FACE_OUTER_BOUND('',#4427,.T.) ;
#2752 = FACE_OUTER_BOUND('',#4428,.T.) ;
#2753 = FACE_OUTER_BOUND('',#4429,.T.) ;
#2754 = FACE_OUTER_BOUND('',#4430,.T.) ;
#2755 = FACE_OUTER_BOUND('',#4431,.T.) ;
#2756 = FACE_OUTER_BOUND('',#4432,.T.) ;
#2757 = FACE_OUTER_BOUND('',#4433,.T.) ;
#2758 = FACE_OUTER_BOUND('',#4434,.T.) ;
#2759 = FACE_OUTER_BOUND('',#4435,.T.) ;
#2760 = FACE_OUTER_BOUND('',#4436,.T.) ;
#2761 = FACE_OUTER_BOUND('',#4437,.T.) ;
#2762 = FACE_OUTER_BOUND('',#4438,.T.) ;
#2763 = FACE_OUTER_BOUND('',#4439,.T.) ;
#2764 = FACE_OUTER_BOUND('',#4440,.T.) ;
#2765 = FACE_OUTER_BOUND('',#4441,.T.) ;
#2766 = FACE_OUTER_BOUND('',#4442,.T.) ;
#2767 = FACE_OUTER_BOUND('',#4443,.T.) ;
#2768 = FACE_OUTER_BOUND('',#4444,.T.) ;
#2769 = FACE_OUTER_BOUND('',#4445,.T.) ;
#2770 = FACE_OUTER_BOUND('',#4446,.T.) ;
#2771 = FACE_OUTER_BOUND('',#4447,.T.) ;
#2772 = FACE_OUTER_BOUND('',#4448,.T.) ;
#2773 = FACE_OUTER_BOUND('',#4449,.T.) ;
#2774 = FACE_OUTER_BOUND('',#4450,.T.) ;
#2775 = FACE_OUTER_BOUND('',#4451,.T.) ;
#2776 = FACE_OUTER_BOUND('',#4452,.T.) ;
#2777 = FACE_OUTER_BOUND('',#4453,.T.) ;
#2778 = FACE_OUTER_BOUND('',#4454,.T.) ;
#2779 = FACE_OUTER_BOUND('',#4455,.T.) ;
#2780 = FACE_OUTER_BOUND('',#4456,.T.) ;
#2781 = FACE_OUTER_BOUND('',#4457,.T.) ;
#2782 = FACE_OUTER_BOUND('',#4458,.T.) ;
#2783 = FACE_OUTER_BOUND('',#4459,.T.) ;
#2784 = FACE_OUTER_BOUND('',#4460,.T.) ;
#2785 = FACE_OUTER_BOUND('',#4461,.T.) ;
#2786 = FACE_OUTER_BOUND('',#4464,.T.) ;
#2787 = FACE_OUTER_BOUND('',#4467,.T.) ;
#2788 = FACE_OUTER_BOUND('',#4468,.T.) ;
#2789 = FACE_OUTER_BOUND('',#4469,.T.) ;
#2790 = FACE_OUTER_BOUND('',#4470,.T.) ;
#2791 = FACE_OUTER_BOUND('',#4471,.T.) ;
#2792 = FACE_OUTER_BOUND('',#4472,.T.) ;
#2793 = FACE_OUTER_BOUND('',#4473,.T.) ;
#2794 = FACE_OUTER_BOUND('',#4474,.T.) ;
#2795 = FACE_OUTER_BOUND('',#4475,.T.) ;
#2796 = FACE_OUTER_BOUND('',#4478,.T.) ;
#2797 = FACE_OUTER_BOUND('',#4481,.T.) ;
#2798 = FACE_OUTER_BOUND('',#4482,.T.) ;
#2799 = FACE_OUTER_BOUND('',#4483,.T.) ;
#2800 = FACE_OUTER_BOUND('',#4484,.T.) ;
#2801 = FACE_OUTER_BOUND('',#4485,.T.) ;
#2802 = FACE_OUTER_BOUND('',#4486,.T.) ;
#2803 = FACE_OUTER_BOUND('',#4487,.T.) ;
#2804 = FACE_OUTER_BOUND('',#4489,.T.) ;
#2805 = FACE_OUTER_BOUND('',#4494,.T.) ;
#2806 = FACE_OUTER_BOUND('',#4495,.T.) ;
#2807 = FACE_OUTER_BOUND('',#4496,.T.) ;
#2808 = FACE_OUTER_BOUND('',#4498,.T.) ;
#2809 = FACE_OUTER_BOUND('',#4499,.T.) ;
#2810 = FACE_OUTER_BOUND('',#4500,.T.) ;
#2811 = FACE_OUTER_BOUND('',#4501,.T.) ;
#2812 = FACE_OUTER_BOUND('',#4502,.T.) ;
#2813 = FACE_OUTER_BOUND('',#4503,.T.) ;
#2814 = FACE_OUTER_BOUND('',#4505,.T.) ;
#2815 = FACE_OUTER_BOUND('',#4506,.T.) ;
#2816 = FACE_OUTER_BOUND('',#4507,.T.) ;
#2817 = FACE_OUTER_BOUND('',#4510,.T.) ;
#2818 = FACE_OUTER_BOUND('',#4511,.T.) ;
#2819 = FACE_OUTER_BOUND('',#4512,.T.) ;
#2820 = FACE_OUTER_BOUND('',#4513,.T.) ;
#2821 = FACE_OUTER_BOUND('',#4514,.T.) ;
#2822 = FACE_OUTER_BOUND('',#4515,.T.) ;
#2823 = FACE_OUTER_BOUND('',#4516,.T.) ;
#2824 = FACE_OUTER_BOUND('',#4517,.T.) ;
#2825 = FACE_OUTER_BOUND('',#4518,.T.) ;
#2826 = FACE_OUTER_BOUND('',#4519,.T.) ;
#2827 = FACE_OUTER_BOUND('',#4520,.T.) ;
#2828 = FACE_OUTER_BOUND('',#4521,.T.) ;
#2829 = FACE_OUTER_BOUND('',#4522,.T.) ;
#2830 = FACE_OUTER_BOUND('',#4523,.T.) ;
#2831 = FACE_OUTER_BOUND('',#4524,.T.) ;
#2832 = FACE_OUTER_BOUND('',#4525,.T.) ;
#2833 = FACE_OUTER_BOUND('',#4526,.T.) ;
#2834 = FACE_OUTER_BOUND('',#4528,.T.) ;
#2835 = FACE_OUTER_BOUND('',#4529,.T.) ;
#2836 = FACE_OUTER_BOUND('',#4530,.T.) ;
#2837 = FACE_OUTER_BOUND('',#4531,.T.) ;
#2838 = FACE_OUTER_BOUND('',#4532,.T.) ;
#2839 = FACE_OUTER_BOUND('',#4533,.T.) ;
#2840 = FACE_OUTER_BOUND('',#4534,.T.) ;
#2841 = FACE_OUTER_BOUND('',#4535,.T.) ;
#2842 = FACE_OUTER_BOUND('',#4537,.T.) ;
#2843 = FACE_OUTER_BOUND('',#4538,.T.) ;
#2844 = FACE_OUTER_BOUND('',#4539,.T.) ;
#2845 = FACE_OUTER_BOUND('',#4540,.T.) ;
#2846 = FACE_OUTER_BOUND('',#4542,.T.) ;
#2847 = FACE_OUTER_BOUND('',#4543,.T.) ;
#2848 = FACE_OUTER_BOUND('',#4544,.T.) ;
#2849 = FACE_OUTER_BOUND('',#4545,.T.) ;
#2850 = FACE_OUTER_BOUND('',#4546,.T.) ;
#2851 = FACE_OUTER_BOUND('',#4547,.T.) ;
#2852 = FACE_OUTER_BOUND('',#4548,.T.) ;
#2853 = FACE_OUTER_BOUND('',#4549,.T.) ;
#2854 = FACE_OUTER_BOUND('',#4551,.T.) ;
#2855 = FACE_OUTER_BOUND('',#4553,.T.) ;
#2856 = FACE_OUTER_BOUND('',#4554,.T.) ;
#2857 = FACE_OUTER_BOUND('',#4555,.T.) ;
#2858 = FACE_OUTER_BOUND('',#4556,.T.) ;
#2859 = FACE_OUTER_BOUND('',#4557,.T.) ;
#2860 = FACE_OUTER_BOUND('',#4558,.T.) ;
#2861 = FACE_OUTER_BOUND('',#4559,.T.) ;
#2862 = FACE_OUTER_BOUND('',#4560,.T.) ;
#2863 = FACE_OUTER_BOUND('',#4561,.T.) ;
#2864 = FACE_OUTER_BOUND('',#4562,.T.) ;
#2865 = FACE_OUTER_BOUND('',#4563,.T.) ;
#2866 = FACE_OUTER_BOUND('',#4565,.T.) ;
#2867 = FACE_OUTER_BOUND('',#4567,.T.) ;
#2868 = FACE_OUTER_BOUND('',#4568,.T.) ;
#2869 = FACE_OUTER_BOUND('',#4571,.T.) ;
#2870 = FACE_OUTER_BOUND('',#4572,.T.) ;
#2871 = FACE_OUTER_BOUND('',#4573,.T.) ;
#2872 = FACE_OUTER_BOUND('',#4575,.T.) ;
#2873 = FACE_OUTER_BOUND('',#4576,.T.) ;
#2874 = FACE_OUTER_BOUND('',#4577,.T.) ;
#2875 = FACE_OUTER_BOUND('',#4578,.T.) ;
#2876 = FACE_OUTER_BOUND('',#4579,.T.) ;
#2877 = FACE_OUTER_BOUND('',#4580,.T.) ;
#2878 = FACE_OUTER_BOUND('',#4582,.T.) ;
#2879 = FACE_OUTER_BOUND('',#4583,.T.) ;
#2880 = FACE_OUTER_BOUND('',#4584,.T.) ;
#2881 = FACE_OUTER_BOUND('',#4589,.T.) ;
#2882 = FACE_OUTER_BOUND('',#4591,.T.) ;
#2883 = FACE_OUTER_BOUND('',#4592,.T.) ;
#2884 = FACE_OUTER_BOUND('',#4593,.T.) ;
#2885 = FACE_OUTER_BOUND('',#4594,.T.) ;
#2886 = FACE_OUTER_BOUND('',#4595,.T.) ;
#2887 = FACE_OUTER_BOUND('',#4596,.T.) ;
#2888 = FACE_OUTER_BOUND('',#4597,.T.) ;
#2889 = FACE_OUTER_BOUND('',#4598,.T.) ;
#2890 = FACE_OUTER_BOUND('',#4599,.T.) ;
#2891 = FACE_OUTER_BOUND('',#4600,.T.) ;
#2892 = FACE_OUTER_BOUND('',#4601,.T.) ;
#2893 = FACE_OUTER_BOUND('',#4602,.T.) ;
#2894 = FACE_OUTER_BOUND('',#4603,.T.) ;
#2895 = FACE_OUTER_BOUND('',#4604,.T.) ;
#2896 = FACE_OUTER_BOUND('',#4606,.T.) ;
#2897 = FACE_OUTER_BOUND('',#4607,.T.) ;
#2898 = FACE_OUTER_BOUND('',#4608,.T.) ;
#2899 = FACE_OUTER_BOUND('',#4610,.T.) ;
#2900 = FACE_OUTER_BOUND('',#4611,.T.) ;
#2901 = FACE_OUTER_BOUND('',#4612,.T.) ;
#2902 = FACE_OUTER_BOUND('',#4614,.T.) ;
#2903 = FACE_OUTER_BOUND('',#4615,.T.) ;
#2904 = FACE_OUTER_BOUND('',#4616,.T.) ;
#2905 = FACE_OUTER_BOUND('',#4617,.T.) ;
#2906 = FACE_OUTER_BOUND('',#4618,.T.) ;
#2907 = FACE_OUTER_BOUND('',#4619,.T.) ;
#2908 = FACE_OUTER_BOUND('',#4620,.T.) ;
#2909 = FACE_OUTER_BOUND('',#4621,.T.) ;
#2910 = FACE_OUTER_BOUND('',#4622,.T.) ;
#2911 = FACE_OUTER_BOUND('',#4623,.T.) ;
#2912 = FACE_OUTER_BOUND('',#4624,.T.) ;
#2913 = FACE_OUTER_BOUND('',#4625,.T.) ;
#2914 = FACE_OUTER_BOUND('',#4626,.T.) ;
#2915 = FACE_OUTER_BOUND('',#4627,.T.) ;
#2916 = FACE_OUTER_BOUND('',#4628,.T.) ;
#2917 = FACE_OUTER_BOUND('',#4629,.T.) ;
#2918 = FACE_OUTER_BOUND('',#4630,.T.) ;
#2919 = FACE_OUTER_BOUND('',#4631,.T.) ;
#2920 = FACE_OUTER_BOUND('',#4632,.T.) ;
#2921 = FACE_OUTER_BOUND('',#4633,.T.) ;
#2922 = FACE_OUTER_BOUND('',#4634,.T.) ;
#2923 = FACE_OUTER_BOUND('',#4635,.T.) ;
#2924 = FACE_OUTER_BOUND('',#4636,.T.) ;
#2925 = FACE_OUTER_BOUND('',#4637,.T.) ;
#2926 = FACE_OUTER_BOUND('',#4638,.T.) ;
#2927 = FACE_OUTER_BOUND('',#4639,.T.) ;
#2928 = FACE_OUTER_BOUND('',#4640,.T.) ;
#2929 = FACE_OUTER_BOUND('',#4641,.T.) ;
#2930 = FACE_OUTER_BOUND('',#4642,.T.) ;
#2931 = FACE_OUTER_BOUND('',#4643,.T.) ;
#2932 = FACE_OUTER_BOUND('',#4644,.T.) ;
#2933 = FACE_OUTER_BOUND('',#4645,.T.) ;
#2934 = FACE_OUTER_BOUND('',#4646,.T.) ;
#2935 = FACE_OUTER_BOUND('',#4647,.T.) ;
#2936 = FACE_OUTER_BOUND('',#4648,.T.) ;
#2937 = FACE_OUTER_BOUND('',#4649,.T.) ;
#2938 = FACE_OUTER_BOUND('',#4650,.T.) ;
#2939 = FACE_OUTER_BOUND('',#4651,.T.) ;
#2940 = FACE_OUTER_BOUND('',#4652,.T.) ;
#2941 = FACE_OUTER_BOUND('',#4653,.T.) ;
#2942 = FACE_OUTER_BOUND('',#4654,.T.) ;
#2943 = FACE_OUTER_BOUND('',#4655,.T.) ;
#2944 = FACE_OUTER_BOUND('',#4656,.T.) ;
#2945 = FACE_OUTER_BOUND('',#4657,.T.) ;
#2946 = FACE_OUTER_BOUND('',#4658,.T.) ;
#2947 = FACE_OUTER_BOUND('',#4659,.T.) ;
#2948 = FACE_OUTER_BOUND('',#4660,.T.) ;
#2949 = FACE_OUTER_BOUND('',#4661,.T.) ;
#2950 = FACE_OUTER_BOUND('',#4662,.T.) ;
#2951 = FACE_OUTER_BOUND('',#4663,.T.) ;
#2952 = FACE_OUTER_BOUND('',#4664,.T.) ;
#2953 = FACE_OUTER_BOUND('',#4665,.T.) ;
#2954 = FACE_OUTER_BOUND('',#4666,.T.) ;
#2955 = FACE_OUTER_BOUND('',#4667,.T.) ;
#2956 = FACE_OUTER_BOUND('',#4668,.T.) ;
#2957 = FACE_OUTER_BOUND('',#4669,.T.) ;
#2958 = FACE_OUTER_BOUND('',#4670,.T.) ;
#2959 = FACE_OUTER_BOUND('',#4671,.T.) ;
#2960 = FACE_OUTER_BOUND('',#4672,.T.) ;
#2961 = FACE_OUTER_BOUND('',#4673,.T.) ;
#2962 = FACE_OUTER_BOUND('',#4674,.T.) ;
#2963 = FACE_OUTER_BOUND('',#4675,.T.) ;
#2964 = FACE_OUTER_BOUND('',#4676,.T.) ;
#2965 = FACE_OUTER_BOUND('',#4677,.T.) ;
#2966 = FACE_OUTER_BOUND('',#4678,.T.) ;
#2967 = FACE_OUTER_BOUND('',#4679,.T.) ;
#2968 = FACE_OUTER_BOUND('',#4680,.T.) ;
#2969 = FACE_OUTER_BOUND('',#4681,.T.) ;
#2970 = FACE_OUTER_BOUND('',#4682,.T.) ;
#2971 = FACE_OUTER_BOUND('',#4683,.T.) ;
#2972 = FACE_OUTER_BOUND('',#4684,.T.) ;
#2973 = FACE_OUTER_BOUND('',#4685,.T.) ;
#2974 = FACE_OUTER_BOUND('',#4686,.T.) ;
#2975 = FACE_OUTER_BOUND('',#4687,.T.) ;
#2976 = FACE_OUTER_BOUND('',#4688,.T.) ;
#2977 = FACE_OUTER_BOUND('',#4689,.T.) ;
#2978 = FACE_OUTER_BOUND('',#4690,.T.) ;
#2979 = FACE_OUTER_BOUND('',#4691,.T.) ;
#2980 = FACE_OUTER_BOUND('',#4692,.T.) ;
#2981 = FACE_OUTER_BOUND('',#4693,.T.) ;
#2982 = FACE_OUTER_BOUND('',#4694,.T.) ;
#2983 = FACE_OUTER_BOUND('',#4695,.T.) ;
#2984 = FACE_OUTER_BOUND('',#4696,.T.) ;
#2985 = FACE_OUTER_BOUND('',#4697,.T.) ;
#2986 = FACE_OUTER_BOUND('',#4698,.T.) ;
#2987 = FACE_OUTER_BOUND('',#4699,.T.) ;
#2988 = FACE_OUTER_BOUND('',#4700,.T.) ;
#2989 = FACE_OUTER_BOUND('',#4701,.T.) ;
#2990 = FACE_OUTER_BOUND('',#4702,.T.) ;
#2991 = FACE_OUTER_BOUND('',#4703,.T.) ;
#2992 = FACE_OUTER_BOUND('',#4704,.T.) ;
#2993 = FACE_OUTER_BOUND('',#4705,.T.) ;
#2994 = FACE_OUTER_BOUND('',#4706,.T.) ;
#2995 = FACE_OUTER_BOUND('',#4707,.T.) ;
#2996 = FACE_OUTER_BOUND('',#4708,.T.) ;
#2997 = FACE_OUTER_BOUND('',#4709,.T.) ;
#2998 = FACE_OUTER_BOUND('',#4710,.T.) ;
#2999 = FACE_OUTER_BOUND('',#4711,.T.) ;
#3000 = FACE_OUTER_BOUND('',#4712,.T.) ;
#3001 = FACE_OUTER_BOUND('',#4713,.T.) ;
#3002 = FACE_OUTER_BOUND('',#4714,.T.) ;
#3003 = FACE_OUTER_BOUND('',#4715,.T.) ;
#3004 = FACE_OUTER_BOUND('',#4716,.T.) ;
#3005 = FACE_OUTER_BOUND('',#4717,.T.) ;
#3006 = FACE_OUTER_BOUND('',#4718,.T.) ;
#3007 = FACE_OUTER_BOUND('',#4719,.T.) ;
#3008 = FACE_OUTER_BOUND('',#4720,.T.) ;
#3009 = FACE_OUTER_BOUND('',#4721,.T.) ;
#3010 = FACE_OUTER_BOUND('',#4722,.T.) ;
#3011 = FACE_OUTER_BOUND('',#4723,.T.) ;
#3012 = FACE_OUTER_BOUND('',#4724,.T.) ;
#3013 = FACE_OUTER_BOUND('',#4725,.T.) ;
#3014 = FACE_OUTER_BOUND('',#4726,.T.) ;
#3015 = FACE_OUTER_BOUND('',#4728,.T.) ;
#3016 = FACE_OUTER_BOUND('',#4729,.T.) ;
#3017 = FACE_OUTER_BOUND('',#4730,.T.) ;
#3018 = FACE_OUTER_BOUND('',#4733,.T.) ;
#3019 = FACE_OUTER_BOUND('',#4734,.T.) ;
#3020 = FACE_OUTER_BOUND('',#4735,.T.) ;
#3021 = FACE_OUTER_BOUND('',#4737,.T.) ;
#3022 = FACE_OUTER_BOUND('',#4738,.T.) ;
#3023 = FACE_OUTER_BOUND('',#4739,.T.) ;
#3024 = FACE_OUTER_BOUND('',#4742,.T.) ;
#3025 = FACE_OUTER_BOUND('',#4743,.T.) ;
#3026 = FACE_OUTER_BOUND('',#4744,.T.) ;
#3027 = FACE_OUTER_BOUND('',#4745,.T.) ;
#3028 = FACE_OUTER_BOUND('',#4746,.T.) ;
#3029 = FACE_OUTER_BOUND('',#4747,.T.) ;
#3030 = FACE_OUTER_BOUND('',#4748,.T.) ;
#3031 = FACE_OUTER_BOUND('',#4749,.T.) ;
#3032 = FACE_OUTER_BOUND('',#4750,.T.) ;
#3033 = FACE_OUTER_BOUND('',#4751,.T.) ;
#3034 = FACE_OUTER_BOUND('',#4752,.T.) ;
#3035 = FACE_OUTER_BOUND('',#4754,.T.) ;
#3036 = FACE_OUTER_BOUND('',#4755,.T.) ;
#3037 = FACE_OUTER_BOUND('',#4756,.T.) ;
#3038 = FACE_OUTER_BOUND('',#4758,.T.) ;
#3039 = FACE_OUTER_BOUND('',#4759,.T.) ;
#3040 = FACE_OUTER_BOUND('',#4760,.T.) ;
#3041 = FACE_OUTER_BOUND('',#4761,.T.) ;
#3042 = FACE_OUTER_BOUND('',#4762,.T.) ;
#3043 = FACE_OUTER_BOUND('',#4763,.T.) ;
#3044 = FACE_OUTER_BOUND('',#4765,.T.) ;
#3045 = FACE_OUTER_BOUND('',#4766,.T.) ;
#3046 = FACE_OUTER_BOUND('',#4767,.T.) ;
#3047 = FACE_OUTER_BOUND('',#4768,.T.) ;
#3048 = FACE_OUTER_BOUND('',#4769,.T.) ;
#3049 = FACE_OUTER_BOUND('',#4770,.T.) ;
#3050 = FACE_OUTER_BOUND('',#4771,.T.) ;
#3051 = FACE_OUTER_BOUND('',#4772,.T.) ;
#3052 = FACE_OUTER_BOUND('',#4773,.T.) ;
#3053 = FACE_OUTER_BOUND('',#4774,.T.) ;
#3054 = FACE_OUTER_BOUND('',#4775,.T.) ;
#3055 = FACE_OUTER_BOUND('',#4776,.T.) ;
#3056 = FACE_OUTER_BOUND('',#4777,.T.) ;
#3057 = FACE_OUTER_BOUND('',#4778,.T.) ;
#3058 = FACE_OUTER_BOUND('',#4779,.T.) ;
#3059 = FACE_OUTER_BOUND('',#4780,.T.) ;
#3060 = FACE_OUTER_BOUND('',#4781,.T.) ;
#3061 = FACE_OUTER_BOUND('',#4782,.T.) ;
#3062 = FACE_OUTER_BOUND('',#4783,.T.) ;
#3063 = FACE_OUTER_BOUND('',#4784,.T.) ;
#3064 = FACE_OUTER_BOUND('',#4786,.T.) ;
#3065 = FACE_OUTER_BOUND('',#4787,.T.) ;
#3066 = FACE_OUTER_BOUND('',#4788,.T.) ;
#3067 = FACE_OUTER_BOUND('',#4789,.T.) ;
#3068 = FACE_OUTER_BOUND('',#4791,.T.) ;
#3069 = FACE_OUTER_BOUND('',#4792,.T.) ;
#3070 = FACE_OUTER_BOUND('',#4793,.T.) ;
#3071 = FACE_OUTER_BOUND('',#4794,.T.) ;
#3072 = FACE_OUTER_BOUND('',#4796,.T.) ;
#3073 = FACE_OUTER_BOUND('',#4798,.T.) ;
#3074 = FACE_OUTER_BOUND('',#4800,.T.) ;
#3075 = FACE_OUTER_BOUND('',#4801,.T.) ;
#3076 = FACE_OUTER_BOUND('',#4802,.T.) ;
#3077 = FACE_OUTER_BOUND('',#4804,.T.) ;
#3078 = FACE_OUTER_BOUND('',#4806,.T.) ;
#3079 = FACE_OUTER_BOUND('',#4808,.T.) ;
#3080 = FACE_OUTER_BOUND('',#4809,.T.) ;
#3081 = FACE_OUTER_BOUND('',#4810,.T.) ;
#3082 = FACE_OUTER_BOUND('',#4812,.T.) ;
#3083 = FACE_OUTER_BOUND('',#4814,.T.) ;
#3084 = FACE_OUTER_BOUND('',#4815,.T.) ;
#3085 = FACE_OUTER_BOUND('',#4816,.T.) ;
#3086 = FACE_OUTER_BOUND('',#4818,.T.) ;
#3087 = FACE_OUTER_BOUND('',#4820,.T.) ;
#3088 = FACE_OUTER_BOUND('',#4821,.T.) ;
#3089 = FACE_OUTER_BOUND('',#4822,.T.) ;
#3090 = FACE_OUTER_BOUND('',#4823,.T.) ;
#3091 = FACE_OUTER_BOUND('',#4827,.T.) ;
#3092 = FACE_OUTER_BOUND('',#4828,.T.) ;
#3093 = FACE_OUTER_BOUND('',#4829,.T.) ;
#3094 = FACE_OUTER_BOUND('',#4830,.T.) ;
#3095 = FACE_OUTER_BOUND('',#4831,.T.) ;
#3096 = FACE_OUTER_BOUND('',#4833,.T.) ;
#3097 = FACE_OUTER_BOUND('',#4834,.T.) ;
#3098 = FACE_OUTER_BOUND('',#4835,.T.) ;
#3099 = FACE_OUTER_BOUND('',#4836,.T.) ;
#3100 = FACE_OUTER_BOUND('',#4837,.T.) ;
#3101 = FACE_OUTER_BOUND('',#4838,.T.) ;
#3102 = FACE_OUTER_BOUND('',#4839,.T.) ;
#3103 = FACE_OUTER_BOUND('',#4840,.T.) ;
#3104 = FACE_OUTER_BOUND('',#4841,.T.) ;
#3105 = FACE_OUTER_BOUND('',#4842,.T.) ;
#3106 = FACE_OUTER_BOUND('',#4843,.T.) ;
#3107 = FACE_OUTER_BOUND('',#4844,.T.) ;
#3108 = FACE_OUTER_BOUND('',#4845,.T.) ;
#3109 = FACE_OUTER_BOUND('',#4846,.T.) ;
#3110 = FACE_OUTER_BOUND('',#4847,.T.) ;
#3111 = FACE_OUTER_BOUND('',#4848,.T.) ;
#3112 = FACE_OUTER_BOUND('',#4849,.T.) ;
#3113 = FACE_OUTER_BOUND('',#4850,.T.) ;
#3114 = FACE_OUTER_BOUND('',#4851,.T.) ;
#3115 = FACE_OUTER_BOUND('',#4852,.T.) ;
#3116 = FACE_OUTER_BOUND('',#4853,.T.) ;
#3117 = FACE_OUTER_BOUND('',#4854,.T.) ;
#3118 = FACE_OUTER_BOUND('',#4855,.T.) ;
#3119 = FACE_OUTER_BOUND('',#4856,.T.) ;
#3120 = FACE_OUTER_BOUND('',#4857,.T.) ;
#3121 = FACE_OUTER_BOUND('',#4858,.T.) ;
#3122 = FACE_OUTER_BOUND('',#4859,.T.) ;
#3123 = FACE_OUTER_BOUND('',#4860,.T.) ;
#3124 = FACE_OUTER_BOUND('',#4861,.T.) ;
#3125 = FACE_OUTER_BOUND('',#4862,.T.) ;
#3126 = FACE_OUTER_BOUND('',#4863,.T.) ;
#3127 = FACE_OUTER_BOUND('',#4864,.T.) ;
#3128 = FACE_OUTER_BOUND('',#4865,.T.) ;
#3129 = FACE_OUTER_BOUND('',#4866,.T.) ;
#3130 = FACE_OUTER_BOUND('',#4867,.T.) ;
#3131 = FACE_OUTER_BOUND('',#4868,.T.) ;
#3132 = FACE_OUTER_BOUND('',#4869,.T.) ;
#3133 = FACE_OUTER_BOUND('',#4870,.T.) ;
#3134 = FACE_OUTER_BOUND('',#4871,.T.) ;
#3135 = FACE_OUTER_BOUND('',#4872,.T.) ;
#3136 = FACE_OUTER_BOUND('',#4873,.T.) ;
#3137 = FACE_OUTER_BOUND('',#4874,.T.) ;
#3138 = FACE_OUTER_BOUND('',#4875,.T.) ;
#3139 = FACE_OUTER_BOUND('',#4876,.T.) ;
#3140 = FACE_OUTER_BOUND('',#4877,.T.) ;
#3141 = FACE_OUTER_BOUND('',#4878,.T.) ;
#3142 = FACE_OUTER_BOUND('',#4879,.T.) ;
#3143 = FACE_OUTER_BOUND('',#4880,.T.) ;
#3144 = FACE_OUTER_BOUND('',#4881,.T.) ;
#3145 = FACE_OUTER_BOUND('',#4882,.T.) ;
#3146 = FACE_OUTER_BOUND('',#4883,.T.) ;
#3147 = FACE_OUTER_BOUND('',#4884,.T.) ;
#3148 = FACE_OUTER_BOUND('',#4885,.T.) ;
#3149 = FACE_OUTER_BOUND('',#4886,.T.) ;
#3150 = FACE_OUTER_BOUND('',#4887,.T.) ;
#3151 = FACE_OUTER_BOUND('',#4888,.T.) ;
#3152 = FACE_OUTER_BOUND('',#4889,.T.) ;
#3153 = FACE_OUTER_BOUND('',#4890,.T.) ;
#3154 = FACE_OUTER_BOUND('',#4891,.T.) ;
#3155 = FACE_OUTER_BOUND('',#4892,.T.) ;
#3156 = FACE_OUTER_BOUND('',#4893,.T.) ;
#3157 = FACE_OUTER_BOUND('',#4894,.T.) ;
#3158 = FACE_OUTER_BOUND('',#4896,.T.) ;
#3159 = FACE_OUTER_BOUND('',#4897,.T.) ;
#3160 = FACE_OUTER_BOUND('',#4899,.T.) ;
#3161 = FACE_OUTER_BOUND('',#4900,.T.) ;
#3162 = FACE_OUTER_BOUND('',#4901,.T.) ;
#3163 = FACE_OUTER_BOUND('',#4903,.T.) ;
#3164 = FACE_OUTER_BOUND('',#4905,.T.) ;
#3165 = FACE_OUTER_BOUND('',#4906,.T.) ;
#3166 = FACE_OUTER_BOUND('',#4907,.T.) ;
#3167 = FACE_OUTER_BOUND('',#4908,.T.) ;
#3168 = FACE_OUTER_BOUND('',#4909,.T.) ;
#3169 = FACE_OUTER_BOUND('',#4910,.T.) ;
#3170 = FACE_OUTER_BOUND('',#4911,.T.) ;
#3171 = FACE_OUTER_BOUND('',#4912,.T.) ;
#3172 = FACE_OUTER_BOUND('',#4913,.T.) ;
#3173 = FACE_OUTER_BOUND('',#4914,.T.) ;
#3174 = FACE_OUTER_BOUND('',#4915,.T.) ;
#3175 = FACE_OUTER_BOUND('',#4916,.T.) ;
#3176 = FACE_OUTER_BOUND('',#4917,.T.) ;
#3177 = FACE_OUTER_BOUND('',#4918,.T.) ;
#3178 = FACE_OUTER_BOUND('',#4919,.T.) ;
#3179 = FACE_OUTER_BOUND('',#4920,.T.) ;
#3180 = FACE_OUTER_BOUND('',#4921,.T.) ;
#3181 = FACE_OUTER_BOUND('',#4922,.T.) ;
#3182 = FACE_OUTER_BOUND('',#4923,.T.) ;
#3183 = FACE_OUTER_BOUND('',#4924,.T.) ;
#3184 = FACE_OUTER_BOUND('',#4925,.T.) ;
#3185 = FACE_OUTER_BOUND('',#4926,.T.) ;
#3186 = FACE_OUTER_BOUND('',#4929,.T.) ;
#3187 = FACE_OUTER_BOUND('',#4931,.T.) ;
#3188 = FACE_OUTER_BOUND('',#4932,.T.) ;
#3189 = FACE_OUTER_BOUND('',#4933,.T.) ;
#3190 = FACE_OUTER_BOUND('',#4935,.T.) ;
#3191 = FACE_OUTER_BOUND('',#4937,.T.) ;
#3192 = FACE_OUTER_BOUND('',#4938,.T.) ;
#3193 = FACE_OUTER_BOUND('',#4939,.T.) ;
#3194 = FACE_OUTER_BOUND('',#4941,.T.) ;
#3195 = FACE_OUTER_BOUND('',#4943,.T.) ;
#3196 = FACE_OUTER_BOUND('',#4944,.T.) ;
#3197 = FACE_OUTER_BOUND('',#4945,.T.) ;
#3198 = FACE_OUTER_BOUND('',#4946,.T.) ;
#3199 = FACE_OUTER_BOUND('',#4948,.T.) ;
#3200 = FACE_OUTER_BOUND('',#4950,.T.) ;
#3201 = FACE_OUTER_BOUND('',#4951,.T.) ;
#3202 = FACE_OUTER_BOUND('',#4958,.T.) ;
#3203 = FACE_OUTER_BOUND('',#4959,.T.) ;
#3204 = FACE_OUTER_BOUND('',#4960,.T.) ;
#3205 = FACE_OUTER_BOUND('',#4961,.T.) ;
#3206 = FACE_OUTER_BOUND('',#4962,.T.) ;
#3207 = FACE_OUTER_BOUND('',#4963,.T.) ;
#3208 = FACE_OUTER_BOUND('',#4964,.T.) ;
#3209 = FACE_OUTER_BOUND('',#4965,.T.) ;
#3210 = FACE_OUTER_BOUND('',#4966,.T.) ;
#3211 = FACE_OUTER_BOUND('',#4967,.T.) ;
#3212 = FACE_OUTER_BOUND('',#4968,.T.) ;
#3213 = FACE_OUTER_BOUND('',#4969,.T.) ;
#3214 = FACE_OUTER_BOUND('',#4970,.T.) ;
#3215 = FACE_OUTER_BOUND('',#4971,.T.) ;
#3216 = FACE_OUTER_BOUND('',#4972,.T.) ;
#3217 = FACE_OUTER_BOUND('',#4973,.T.) ;
#3218 = FACE_OUTER_BOUND('',#4974,.T.) ;
#3219 = FACE_OUTER_BOUND('',#4975,.T.) ;
#3220 = FACE_OUTER_BOUND('',#4976,.T.) ;
#3221 = FACE_OUTER_BOUND('',#4977,.T.) ;
#3222 = FACE_OUTER_BOUND('',#4978,.T.) ;
#3223 = FACE_OUTER_BOUND('',#4979,.T.) ;
#3224 = FACE_OUTER_BOUND('',#4980,.T.) ;
#3225 = FACE_OUTER_BOUND('',#4981,.T.) ;
#3226 = FACE_OUTER_BOUND('',#4982,.T.) ;
#3227 = FACE_OUTER_BOUND('',#4983,.T.) ;
#3228 = FACE_OUTER_BOUND('',#4984,.T.) ;
#3229 = FACE_OUTER_BOUND('',#4985,.T.) ;
#3230 = FACE_OUTER_BOUND('',#4986,.T.) ;
#3231 = FACE_OUTER_BOUND('',#4987,.T.) ;
#3232 = FACE_OUTER_BOUND('',#4988,.T.) ;
#3233 = FACE_OUTER_BOUND('',#4989,.T.) ;
#3234 = FACE_OUTER_BOUND('',#4990,.T.) ;
#3235 = FACE_OUTER_BOUND('',#4991,.T.) ;
#3236 = FACE_OUTER_BOUND('',#4992,.T.) ;
#3237 = FACE_OUTER_BOUND('',#4993,.T.) ;
#3238 = FACE_OUTER_BOUND('',#4994,.T.) ;
#3239 = FACE_OUTER_BOUND('',#4995,.T.) ;
#3240 = FACE_OUTER_BOUND('',#4996,.T.) ;
#3241 = FACE_OUTER_BOUND('',#4997,.T.) ;
#3242 = FACE_OUTER_BOUND('',#4998,.T.) ;
#3243 = FACE_OUTER_BOUND('',#4999,.T.) ;
#3244 = FACE_OUTER_BOUND('',#5000,.T.) ;
#3245 = FACE_OUTER_BOUND('',#5001,.T.) ;
#3246 = FACE_OUTER_BOUND('',#5002,.T.) ;
#3247 = FACE_OUTER_BOUND('',#5003,.T.) ;
#3248 = FACE_OUTER_BOUND('',#5005,.T.) ;
#3249 = FACE_OUTER_BOUND('',#5007,.T.) ;
#3250 = FACE_OUTER_BOUND('',#5008,.T.) ;
#3251 = FACE_OUTER_BOUND('',#5010,.T.) ;
#3252 = FACE_OUTER_BOUND('',#5011,.T.) ;
#3253 = FACE_OUTER_BOUND('',#5012,.T.) ;
#3254 = FACE_OUTER_BOUND('',#5013,.T.) ;
#3255 = FACE_OUTER_BOUND('',#5015,.T.) ;
#3256 = FACE_OUTER_BOUND('',#5016,.T.) ;
#3257 = FACE_OUTER_BOUND('',#5017,.T.) ;
#3258 = FACE_OUTER_BOUND('',#5018,.T.) ;
#3259 = FACE_OUTER_BOUND('',#5019,.T.) ;
#3260 = FACE_OUTER_BOUND('',#5020,.T.) ;
#3261 = FACE_OUTER_BOUND('',#5022,.T.) ;
#3262 = FACE_OUTER_BOUND('',#5023,.T.) ;
#3263 = FACE_OUTER_BOUND('',#5025,.T.) ;
#3264 = FACE_OUTER_BOUND('',#5026,.T.) ;
#3265 = FACE_OUTER_BOUND('',#5027,.T.) ;
#3266 = FACE_OUTER_BOUND('',#5028,.T.) ;
#3267 = FACE_OUTER_BOUND('',#5029,.T.) ;
#3268 = FACE_OUTER_BOUND('',#5030,.T.) ;
#3269 = FACE_OUTER_BOUND('',#5033,.T.) ;
#3270 = FACE_OUTER_BOUND('',#5034,.T.) ;
#3271 = FACE_OUTER_BOUND('',#5037,.T.) ;
#3272 = FACE_OUTER_BOUND('',#5038,.T.) ;
#3273 = FACE_OUTER_BOUND('',#5039,.T.) ;
#3274 = FACE_OUTER_BOUND('',#5040,.T.) ;
#3275 = FACE_OUTER_BOUND('',#5041,.T.) ;
#3276 = FACE_OUTER_BOUND('',#5044,.T.) ;
#3277 = FACE_OUTER_BOUND('',#5045,.T.) ;
#3278 = FACE_OUTER_BOUND('',#5046,.T.) ;
#3279 = FACE_OUTER_BOUND('',#5047,.T.) ;
#3280 = FACE_OUTER_BOUND('',#5048,.T.) ;
#3281 = FACE_OUTER_BOUND('',#5055,.T.) ;
#3282 = FACE_OUTER_BOUND('',#5056,.T.) ;
#3283 = FACE_OUTER_BOUND('',#5057,.T.) ;
#3284 = FACE_OUTER_BOUND('',#5058,.T.) ;
#3285 = FACE_OUTER_BOUND('',#5059,.T.) ;
#3286 = FACE_OUTER_BOUND('',#5060,.T.) ;
#3287 = FACE_OUTER_BOUND('',#5061,.T.) ;
#3288 = FACE_OUTER_BOUND('',#5062,.T.) ;
#3289 = FACE_OUTER_BOUND('',#5063,.T.) ;
#3290 = FACE_OUTER_BOUND('',#5064,.T.) ;
#3291 = FACE_OUTER_BOUND('',#5065,.T.) ;
#3292 = FACE_OUTER_BOUND('',#5066,.T.) ;
#3293 = FACE_OUTER_BOUND('',#5067,.T.) ;
#3294 = FACE_OUTER_BOUND('',#5068,.T.) ;
#3295 = FACE_OUTER_BOUND('',#5069,.T.) ;
#3296 = FACE_OUTER_BOUND('',#5070,.T.) ;
#3297 = FACE_OUTER_BOUND('',#5071,.T.) ;
#3298 = FACE_OUTER_BOUND('',#5072,.T.) ;
#3299 = FACE_OUTER_BOUND('',#5073,.T.) ;
#3300 = FACE_OUTER_BOUND('',#5074,.T.) ;
#3301 = FACE_OUTER_BOUND('',#5075,.T.) ;
#3302 = FACE_OUTER_BOUND('',#5076,.T.) ;
#3303 = FACE_OUTER_BOUND('',#5077,.T.) ;
#3304 = FACE_OUTER_BOUND('',#5078,.T.) ;
#3305 = FACE_OUTER_BOUND('',#5079,.T.) ;
#3306 = FACE_OUTER_BOUND('',#5080,.T.) ;
#3307 = FACE_OUTER_BOUND('',#5084,.T.) ;
#3308 = FACE_OUTER_BOUND('',#5088,.T.) ;
#3309 = FACE_OUTER_BOUND('',#5089,.T.) ;
#3310 = FACE_OUTER_BOUND('',#5090,.T.) ;
#3311 = FACE_OUTER_BOUND('',#5091,.T.) ;
#3312 = FACE_OUTER_BOUND('',#5092,.T.) ;
#3313 = FACE_OUTER_BOUND('',#5093,.T.) ;
#3314 = FACE_OUTER_BOUND('',#5094,.T.) ;
#3315 = FACE_OUTER_BOUND('',#5095,.T.) ;
#3316 = FACE_OUTER_BOUND('',#5096,.T.) ;
#3317 = FACE_OUTER_BOUND('',#5097,.T.) ;
#3318 = FACE_OUTER_BOUND('',#5098,.T.) ;
#3319 = FACE_OUTER_BOUND('',#5099,.T.) ;
#3320 = FACE_OUTER_BOUND('',#5100,.T.) ;
#3321 = FACE_OUTER_BOUND('',#5101,.T.) ;
#3322 = FACE_OUTER_BOUND('',#5102,.T.) ;
#3323 = FACE_OUTER_BOUND('',#5103,.T.) ;
#3324 = FACE_OUTER_BOUND('',#5104,.T.) ;
#3325 = FACE_OUTER_BOUND('',#5105,.T.) ;
#3326 = FACE_OUTER_BOUND('',#5106,.T.) ;
#3327 = FACE_OUTER_BOUND('',#5107,.T.) ;
#3328 = FACE_OUTER_BOUND('',#5108,.T.) ;
#3329 = FACE_OUTER_BOUND('',#5109,.T.) ;
#3330 = FACE_OUTER_BOUND('',#5110,.T.) ;
#3331 = FACE_OUTER_BOUND('',#5111,.T.) ;
#3332 = FACE_OUTER_BOUND('',#5112,.T.) ;
#3333 = FACE_OUTER_BOUND('',#5113,.T.) ;
#3334 = FACE_OUTER_BOUND('',#5114,.T.) ;
#3335 = FACE_OUTER_BOUND('',#5115,.T.) ;
#3336 = FACE_OUTER_BOUND('',#5116,.T.) ;
#3337 = FACE_OUTER_BOUND('',#5117,.T.) ;
#3338 = FACE_OUTER_BOUND('',#5118,.T.) ;
#3339 = FACE_OUTER_BOUND('',#5119,.T.) ;
#3340 = FACE_OUTER_BOUND('',#5120,.T.) ;
#3341 = FACE_OUTER_BOUND('',#5121,.T.) ;
#3342 = FACE_OUTER_BOUND('',#5122,.T.) ;
#3343 = FACE_OUTER_BOUND('',#5123,.T.) ;
#3344 = FACE_OUTER_BOUND('',#5124,.T.) ;
#3345 = FACE_OUTER_BOUND('',#5125,.T.) ;
#3346 = FACE_OUTER_BOUND('',#5126,.T.) ;
#3347 = FACE_OUTER_BOUND('',#5127,.T.) ;
#3348 = FACE_OUTER_BOUND('',#5128,.T.) ;
#3349 = FACE_OUTER_BOUND('',#5129,.T.) ;
#3350 = FACE_OUTER_BOUND('',#5130,.T.) ;
#3351 = FACE_OUTER_BOUND('',#5131,.T.) ;
#3352 = FACE_OUTER_BOUND('',#5132,.T.) ;
#3353 = FACE_OUTER_BOUND('',#5133,.T.) ;
#3354 = FACE_OUTER_BOUND('',#5134,.T.) ;
#3355 = FACE_OUTER_BOUND('',#5135,.T.) ;
#3356 = FACE_OUTER_BOUND('',#5136,.T.) ;
#3357 = FACE_OUTER_BOUND('',#5138,.T.) ;
#3358 = FACE_OUTER_BOUND('',#5144,.T.) ;
#3359 = FACE_OUTER_BOUND('',#5145,.T.) ;
#3360 = FACE_OUTER_BOUND('',#5146,.T.) ;
#3361 = FACE_OUTER_BOUND('',#5152,.T.) ;
#3362 = FACE_OUTER_BOUND('',#5153,.T.) ;
#3363 = FACE_OUTER_BOUND('',#5154,.T.) ;
#3364 = FACE_OUTER_BOUND('',#5155,.T.) ;
#3365 = FACE_OUTER_BOUND('',#5156,.T.) ;
#3366 = FACE_OUTER_BOUND('',#5157,.T.) ;
#3367 = FACE_OUTER_BOUND('',#5159,.T.) ;
#3368 = FACE_OUTER_BOUND('',#5160,.T.) ;
#3369 = FACE_OUTER_BOUND('',#5161,.T.) ;
#3370 = FACE_OUTER_BOUND('',#5162,.T.) ;
#3371 = FACE_OUTER_BOUND('',#5164,.T.) ;
#3372 = FACE_OUTER_BOUND('',#5166,.T.) ;
#3373 = FACE_OUTER_BOUND('',#5168,.T.) ;
#3374 = FACE_OUTER_BOUND('',#5170,.T.) ;
#3375 = FACE_OUTER_BOUND('',#5171,.T.) ;
#3376 = FACE_OUTER_BOUND('',#5172,.T.) ;
#3377 = FACE_OUTER_BOUND('',#5173,.T.) ;
#3378 = FACE_OUTER_BOUND('',#5174,.T.) ;
#3379 = FACE_OUTER_BOUND('',#5175,.T.) ;
#3380 = FACE_OUTER_BOUND('',#5176,.T.) ;
#3381 = FACE_OUTER_BOUND('',#5177,.T.) ;
#3382 = FACE_OUTER_BOUND('',#5178,.T.) ;
#3383 = FACE_OUTER_BOUND('',#5179,.T.) ;
#3384 = FACE_OUTER_BOUND('',#5180,.T.) ;
#3385 = FACE_OUTER_BOUND('',#5181,.T.) ;
#3386 = FACE_OUTER_BOUND('',#5190,.T.) ;
#3387 = FACE_OUTER_BOUND('',#5199,.T.) ;
#3388 = FACE_OUTER_BOUND('',#5200,.T.) ;
#3389 = FACE_OUTER_BOUND('',#5201,.T.) ;
#3390 = FACE_OUTER_BOUND('',#5202,.T.) ;
#3391 = FACE_OUTER_BOUND('',#5203,.T.) ;
#3392 = FACE_OUTER_BOUND('',#5204,.T.) ;
#3393 = FACE_OUTER_BOUND('',#5205,.T.) ;
#3394 = FACE_OUTER_BOUND('',#5207,.T.) ;
#3395 = FACE_OUTER_BOUND('',#5208,.T.) ;
#3396 = FACE_OUTER_BOUND('',#5209,.T.) ;
#3397 = FACE_OUTER_BOUND('',#5210,.T.) ;
#3398 = FACE_OUTER_BOUND('',#5212,.T.) ;
#3399 = FACE_OUTER_BOUND('',#5214,.T.) ;
#3400 = FACE_OUTER_BOUND('',#5216,.T.) ;
#3401 = FACE_OUTER_BOUND('',#5217,.T.) ;
#3402 = FACE_OUTER_BOUND('',#5219,.T.) ;
#3403 = FACE_OUTER_BOUND('',#5220,.T.) ;
#3404 = FACE_OUTER_BOUND('',#5221,.T.) ;
#3405 = FACE_OUTER_BOUND('',#5222,.T.) ;
#3406 = FACE_OUTER_BOUND('',#5223,.T.) ;
#3407 = FACE_OUTER_BOUND('',#5224,.T.) ;
#3408 = FACE_OUTER_BOUND('',#5225,.T.) ;
#3409 = FACE_OUTER_BOUND('',#5226,.T.) ;
#3410 = FACE_OUTER_BOUND('',#5227,.T.) ;
#3411 = FACE_OUTER_BOUND('',#5228,.T.) ;
#3412 = FACE_OUTER_BOUND('',#5230,.T.) ;
#3413 = FACE_OUTER_BOUND('',#5231,.T.) ;
#3414 = FACE_OUTER_BOUND('',#5232,.T.) ;
#3415 = FACE_OUTER_BOUND('',#5233,.T.) ;
#3416 = FACE_OUTER_BOUND('',#5235,.T.) ;
#3417 = FACE_OUTER_BOUND('',#5236,.T.) ;
#3418 = FACE_OUTER_BOUND('',#5237,.T.) ;
#3419 = FACE_OUTER_BOUND('',#5238,.T.) ;
#3420 = FACE_OUTER_BOUND('',#5239,.T.) ;
#3421 = FACE_OUTER_BOUND('',#5240,.T.) ;
#3422 = FACE_OUTER_BOUND('',#5241,.T.) ;
#3423 = FACE_OUTER_BOUND('',#5242,.T.) ;
#3424 = FACE_OUTER_BOUND('',#5243,.T.) ;
#3425 = FACE_OUTER_BOUND('',#5244,.T.) ;
#3426 = FACE_OUTER_BOUND('',#5245,.T.) ;
#3427 = FACE_OUTER_BOUND('',#5246,.T.) ;
#3428 = FACE_OUTER_BOUND('',#5247,.T.) ;
#3429 = FACE_OUTER_BOUND('',#5248,.T.) ;
#3430 = FACE_OUTER_BOUND('',#5249,.T.) ;
#3431 = FACE_OUTER_BOUND('',#5250,.T.) ;
#3432 = FACE_OUTER_BOUND('',#5251,.T.) ;
#3433 = FACE_OUTER_BOUND('',#5252,.T.) ;
#3434 = FACE_OUTER_BOUND('',#5254,.T.) ;
#3435 = FACE_OUTER_BOUND('',#5255,.T.) ;
#3436 = FACE_OUTER_BOUND('',#5256,.T.) ;
#3437 = FACE_OUTER_BOUND('',#5257,.T.) ;
#3438 = FACE_OUTER_BOUND('',#5258,.T.) ;
#3439 = FACE_OUTER_BOUND('',#5259,.T.) ;
#3440 = FACE_OUTER_BOUND('',#5260,.T.) ;
#3441 = FACE_OUTER_BOUND('',#5262,.T.) ;
#3442 = FACE_OUTER_BOUND('',#5263,.T.) ;
#3443 = FACE_OUTER_BOUND('',#5264,.T.) ;
#3444 = FACE_OUTER_BOUND('',#5265,.T.) ;
#3445 = FACE_OUTER_BOUND('',#5266,.T.) ;
#3446 = FACE_OUTER_BOUND('',#5267,.T.) ;
#3447 = FACE_OUTER_BOUND('',#5268,.T.) ;
#3448 = FACE_OUTER_BOUND('',#5269,.T.) ;
#3449 = FACE_OUTER_BOUND('',#5270,.T.) ;
#3450 = FACE_OUTER_BOUND('',#5271,.T.) ;
#3451 = FACE_OUTER_BOUND('',#5272,.T.) ;
#3452 = FACE_OUTER_BOUND('',#5273,.T.) ;
#3453 = FACE_OUTER_BOUND('',#5274,.T.) ;
#3454 = FACE_OUTER_BOUND('',#5275,.T.) ;
#3455 = FACE_OUTER_BOUND('',#5276,.T.) ;
#3456 = FACE_OUTER_BOUND('',#5277,.T.) ;
#3457 = FACE_OUTER_BOUND('',#5278,.T.) ;
#3458 = FACE_OUTER_BOUND('',#5279,.T.) ;
#3459 = FACE_OUTER_BOUND('',#5280,.T.) ;
#3460 = FACE_OUTER_BOUND('',#5281,.T.) ;
#3461 = FACE_OUTER_BOUND('',#5282,.T.) ;
#3462 = FACE_OUTER_BOUND('',#5283,.T.) ;
#3463 = FACE_OUTER_BOUND('',#5284,.T.) ;
#3464 = FACE_OUTER_BOUND('',#5285,.T.) ;
#3465 = FACE_OUTER_BOUND('',#5286,.T.) ;
#3466 = FACE_OUTER_BOUND('',#5287,.T.) ;
#3467 = FACE_OUTER_BOUND('',#5288,.T.) ;
#3468 = FACE_OUTER_BOUND('',#5289,.T.) ;
#3469 = FACE_OUTER_BOUND('',#5290,.T.) ;
#3470 = FACE_OUTER_BOUND('',#5291,.T.) ;
#3471 = FACE_OUTER_BOUND('',#5292,.T.) ;
#3472 = FACE_OUTER_BOUND('',#5293,.T.) ;
#3473 = FACE_OUTER_BOUND('',#5294,.T.) ;
#3474 = FACE_OUTER_BOUND('',#5295,.T.) ;
#3475 = FACE_OUTER_BOUND('',#5296,.T.) ;
#3476 = FACE_OUTER_BOUND('',#5298,.T.) ;
#3477 = FACE_OUTER_BOUND('',#5299,.T.) ;
#3478 = FACE_OUTER_BOUND('',#5301,.T.) ;
#3479 = FACE_OUTER_BOUND('',#5303,.T.) ;
#3480 = FACE_OUTER_BOUND('',#5304,.T.) ;
#3481 = FACE_OUTER_BOUND('',#5305,.T.) ;
#3482 = FACE_OUTER_BOUND('',#5306,.T.) ;
#3483 = FACE_OUTER_BOUND('',#5307,.T.) ;
#3484 = FACE_OUTER_BOUND('',#5309,.T.) ;
#3485 = FACE_OUTER_BOUND('',#5311,.T.) ;
#3486 = FACE_OUTER_BOUND('',#5312,.T.) ;
#3487 = FACE_OUTER_BOUND('',#5313,.T.) ;
#3488 = FACE_OUTER_BOUND('',#5315,.T.) ;
#3489 = FACE_OUTER_BOUND('',#5317,.T.) ;
#3490 = FACE_OUTER_BOUND('',#5318,.T.) ;
#3491 = FACE_OUTER_BOUND('',#5319,.T.) ;
#3492 = FACE_OUTER_BOUND('',#5320,.T.) ;
#3493 = FACE_OUTER_BOUND('',#5321,.T.) ;
#3494 = FACE_OUTER_BOUND('',#5322,.T.) ;
#3495 = FACE_OUTER_BOUND('',#5323,.T.) ;
#3496 = FACE_OUTER_BOUND('',#5324,.T.) ;
#3497 = FACE_OUTER_BOUND('',#5325,.T.) ;
#3498 = FACE_OUTER_BOUND('',#5326,.T.) ;
#3499 = FACE_OUTER_BOUND('',#5327,.T.) ;
#3500 = FACE_OUTER_BOUND('',#5328,.T.) ;
#3501 = FACE_OUTER_BOUND('',#5329,.T.) ;
#3502 = FACE_OUTER_BOUND('',#5330,.T.) ;
#3503 = FACE_OUTER_BOUND('',#5331,.T.) ;
#3504 = FACE_OUTER_BOUND('',#5332,.T.) ;
#3505 = FACE_OUTER_BOUND('',#5333,.T.) ;
#3506 = FACE_OUTER_BOUND('',#5334,.T.) ;
#3507 = FACE_OUTER_BOUND('',#5335,.T.) ;
#3508 = FACE_OUTER_BOUND('',#5336,.T.) ;
#3509 = FACE_OUTER_BOUND('',#5337,.T.) ;
#3510 = FACE_OUTER_BOUND('',#5338,.T.) ;
#3511 = FACE_OUTER_BOUND('',#5339,.T.) ;
#3512 = FACE_OUTER_BOUND('',#5340,.T.) ;
#3513 = FACE_OUTER_BOUND('',#5341,.T.) ;
#3514 = FACE_OUTER_BOUND('',#5342,.T.) ;
#3515 = FACE_OUTER_BOUND('',#5343,.T.) ;
#3516 = FACE_OUTER_BOUND('',#5344,.T.) ;
#3517 = FACE_OUTER_BOUND('',#5345,.T.) ;
#3518 = FACE_OUTER_BOUND('',#5346,.T.) ;
#3519 = FACE_OUTER_BOUND('',#5347,.T.) ;
#3520 = FACE_OUTER_BOUND('',#5348,.T.) ;
#3521 = FACE_OUTER_BOUND('',#5349,.T.) ;
#3522 = FACE_OUTER_BOUND('',#5350,.T.) ;
#3523 = FACE_OUTER_BOUND('',#5351,.T.) ;
#3524 = FACE_OUTER_BOUND('',#5352,.T.) ;
#3525 = FACE_OUTER_BOUND('',#5353,.T.) ;
#3526 = FACE_OUTER_BOUND('',#5354,.T.) ;
#3527 = FACE_OUTER_BOUND('',#5355,.T.) ;
#3528 = FACE_OUTER_BOUND('',#5356,.T.) ;
#3529 = FACE_OUTER_BOUND('',#5357,.T.) ;
#3530 = FACE_OUTER_BOUND('',#5358,.T.) ;
#3531 = FACE_OUTER_BOUND('',#5359,.T.) ;
#3532 = FACE_OUTER_BOUND('',#5360,.T.) ;
#3533 = FACE_OUTER_BOUND('',#5361,.T.) ;
#3534 = FACE_OUTER_BOUND('',#5362,.T.) ;
#3535 = FACE_OUTER_BOUND('',#5363,.T.) ;
#3536 = FACE_OUTER_BOUND('',#5364,.T.) ;
#3537 = FACE_OUTER_BOUND('',#5365,.T.) ;
#3538 = FACE_OUTER_BOUND('',#5366,.T.) ;
#3539 = FACE_OUTER_BOUND('',#5367,.T.) ;
#3540 = FACE_OUTER_BOUND('',#5368,.T.) ;
#3541 = FACE_OUTER_BOUND('',#5369,.T.) ;
#3542 = FACE_OUTER_BOUND('',#5370,.T.) ;
#3543 = FACE_OUTER_BOUND('',#5371,.T.) ;
#3544 = FACE_OUTER_BOUND('',#5372,.T.) ;
#3545 = FACE_OUTER_BOUND('',#5373,.T.) ;
#3546 = FACE_OUTER_BOUND('',#5374,.T.) ;
#3547 = FACE_OUTER_BOUND('',#5375,.T.) ;
#3548 = FACE_OUTER_BOUND('',#5376,.T.) ;
#3549 = FACE_OUTER_BOUND('',#5377,.T.) ;
#3550 = FACE_OUTER_BOUND('',#5378,.T.) ;
#3551 = FACE_OUTER_BOUND('',#5379,.T.) ;
#3552 = FACE_OUTER_BOUND('',#5380,.T.) ;
#3553 = FACE_OUTER_BOUND('',#5381,.T.) ;
#3554 = FACE_OUTER_BOUND('',#5382,.T.) ;
#3555 = FACE_OUTER_BOUND('',#5383,.T.) ;
#3556 = FACE_OUTER_BOUND('',#5384,.T.) ;
#3557 = FACE_OUTER_BOUND('',#5385,.T.) ;
#3558 = FACE_OUTER_BOUND('',#5386,.T.) ;
#3559 = FACE_OUTER_BOUND('',#5387,.T.) ;
#3560 = FACE_OUTER_BOUND('',#5388,.T.) ;
#3561 = FACE_OUTER_BOUND('',#5389,.T.) ;
#3562 = FACE_OUTER_BOUND('',#5390,.T.) ;
#3563 = FACE_OUTER_BOUND('',#5391,.T.) ;
#3564 = FACE_OUTER_BOUND('',#5392,.T.) ;
#3565 = FACE_OUTER_BOUND('',#5393,.T.) ;
#3566 = FACE_OUTER_BOUND('',#5394,.T.) ;
#3567 = FACE_OUTER_BOUND('',#5395,.T.) ;
#3568 = FACE_OUTER_BOUND('',#5396,.T.) ;
#3569 = FACE_OUTER_BOUND('',#5397,.T.) ;
#3570 = FACE_OUTER_BOUND('',#5398,.T.) ;
#3571 = FACE_OUTER_BOUND('',#5399,.T.) ;
#3572 = FACE_OUTER_BOUND('',#5400,.T.) ;
#3573 = FACE_OUTER_BOUND('',#5401,.T.) ;
#3574 = FACE_OUTER_BOUND('',#5402,.T.) ;
#3575 = FACE_OUTER_BOUND('',#5403,.T.) ;
#3576 = FACE_OUTER_BOUND('',#5404,.T.) ;
#3577 = FACE_OUTER_BOUND('',#5405,.T.) ;
#3578 = FACE_OUTER_BOUND('',#5406,.T.) ;
#3579 = FACE_OUTER_BOUND('',#5407,.T.) ;
#3580 = FACE_OUTER_BOUND('',#5408,.T.) ;
#3581 = FACE_OUTER_BOUND('',#5409,.T.) ;
#3582 = FACE_OUTER_BOUND('',#5410,.T.) ;
#3583 = FACE_OUTER_BOUND('',#5411,.T.) ;
#3584 = FACE_OUTER_BOUND('',#5412,.T.) ;
#3585 = FACE_OUTER_BOUND('',#5413,.T.) ;
#3586 = FACE_OUTER_BOUND('',#5414,.T.) ;
#3587 = FACE_OUTER_BOUND('',#5415,.T.) ;
#3588 = FACE_OUTER_BOUND('',#5416,.T.) ;
#3589 = FACE_OUTER_BOUND('',#5417,.T.) ;
#3590 = FACE_OUTER_BOUND('',#5418,.T.) ;
#3591 = FACE_OUTER_BOUND('',#5419,.T.) ;
#3592 = FACE_OUTER_BOUND('',#5420,.T.) ;
#3593 = FACE_OUTER_BOUND('',#5421,.T.) ;
#3594 = FACE_OUTER_BOUND('',#5422,.T.) ;
#3595 = FACE_OUTER_BOUND('',#5423,.T.) ;
#3596 = FACE_OUTER_BOUND('',#5424,.T.) ;
#3597 = FACE_OUTER_BOUND('',#5425,.T.) ;
#3598 = FACE_OUTER_BOUND('',#5426,.T.) ;
#3599 = FACE_OUTER_BOUND('',#5427,.T.) ;
#3600 = FACE_OUTER_BOUND('',#5428,.T.) ;
#3601 = FACE_OUTER_BOUND('',#5429,.T.) ;
#3602 = FACE_OUTER_BOUND('',#5430,.T.) ;
#3603 = FACE_OUTER_BOUND('',#5431,.T.) ;
#3604 = FACE_OUTER_BOUND('',#5432,.T.) ;
#3605 = FACE_OUTER_BOUND('',#5433,.T.) ;
#3606 = FACE_OUTER_BOUND('',#5434,.T.) ;
#3607 = FACE_OUTER_BOUND('',#5435,.T.) ;
#3608 = FACE_OUTER_BOUND('',#5436,.T.) ;
#3609 = FACE_OUTER_BOUND('',#5437,.T.) ;
#3610 = FACE_OUTER_BOUND('',#5438,.T.) ;
#3611 = FACE_OUTER_BOUND('',#5439,.T.) ;
#3612 = FACE_OUTER_BOUND('',#5440,.T.) ;
#3613 = FACE_OUTER_BOUND('',#5441,.T.) ;
#3614 = FACE_OUTER_BOUND('',#5442,.T.) ;
#3615 = FACE_OUTER_BOUND('',#5443,.T.) ;
#3616 = FACE_OUTER_BOUND('',#5444,.T.) ;
#3617 = FACE_OUTER_BOUND('',#5445,.T.) ;
#3618 = FACE_OUTER_BOUND('',#5446,.T.) ;
#3619 = FACE_OUTER_BOUND('',#5447,.T.) ;
#3620 = FACE_OUTER_BOUND('',#5448,.T.) ;
#3621 = FACE_OUTER_BOUND('',#5449,.T.) ;
#3622 = FACE_OUTER_BOUND('',#5450,.T.) ;
#3623 = FACE_OUTER_BOUND('',#5451,.T.) ;
#3624 = FACE_OUTER_BOUND('',#5452,.T.) ;
#3625 = FACE_OUTER_BOUND('',#5453,.T.) ;
#3626 = FACE_OUTER_BOUND('',#5454,.T.) ;
#3627 = FACE_OUTER_BOUND('',#5455,.T.) ;
#3628 = FACE_OUTER_BOUND('',#5456,.T.) ;
#3629 = FACE_OUTER_BOUND('',#5457,.T.) ;
#3630 = FACE_OUTER_BOUND('',#5458,.T.) ;
#3631 = FACE_OUTER_BOUND('',#5459,.T.) ;
#3632 = FACE_OUTER_BOUND('',#5460,.T.) ;
#3633 = FACE_OUTER_BOUND('',#5461,.T.) ;
#3634 = FACE_OUTER_BOUND('',#5462,.T.) ;
#3635 = FACE_OUTER_BOUND('',#5463,.T.) ;
#3636 = FACE_OUTER_BOUND('',#5464,.T.) ;
#3637 = FACE_OUTER_BOUND('',#5465,.T.) ;
#3638 = FACE_OUTER_BOUND('',#5466,.T.) ;
#3639 = FACE_OUTER_BOUND('',#5467,.T.) ;
#3640 = FACE_OUTER_BOUND('',#5468,.T.) ;
#3641 = FACE_OUTER_BOUND('',#5469,.T.) ;
#3642 = FACE_OUTER_BOUND('',#5470,.T.) ;
#3643 = FACE_OUTER_BOUND('',#5471,.T.) ;
#3644 = FACE_OUTER_BOUND('',#5472,.T.) ;
#3645 = FACE_OUTER_BOUND('',#5473,.T.) ;
#3646 = FACE_OUTER_BOUND('',#5474,.T.) ;
#3647 = FACE_OUTER_BOUND('',#5475,.T.) ;
#3648 = FACE_OUTER_BOUND('',#5476,.T.) ;
#3649 = FACE_OUTER_BOUND('',#5477,.T.) ;
#3650 = FACE_OUTER_BOUND('',#5478,.T.) ;
#3651 = FACE_OUTER_BOUND('',#5479,.T.) ;
#3652 = FACE_OUTER_BOUND('',#5480,.T.) ;
#3653 = FACE_OUTER_BOUND('',#5481,.T.) ;
#3654 = FACE_OUTER_BOUND('',#5482,.T.) ;
#3655 = FACE_OUTER_BOUND('',#5483,.T.) ;
#3656 = FACE_OUTER_BOUND('',#5484,.T.) ;
#3657 = FACE_OUTER_BOUND('',#5485,.T.) ;
#3658 = FACE_OUTER_BOUND('',#5486,.T.) ;
#3659 = FACE_OUTER_BOUND('',#5487,.T.) ;
#3660 = FACE_OUTER_BOUND('',#5488,.T.) ;
#3661 = FACE_OUTER_BOUND('',#5489,.T.) ;
#3662 = FACE_OUTER_BOUND('',#5490,.T.) ;
#3663 = FACE_OUTER_BOUND('',#5491,.T.) ;
#3664 = FACE_OUTER_BOUND('',#5492,.T.) ;
#3665 = FACE_OUTER_BOUND('',#5493,.T.) ;
#3666 = FACE_OUTER_BOUND('',#5494,.T.) ;
#3667 = FACE_OUTER_BOUND('',#5495,.T.) ;
#3668 = FACE_OUTER_BOUND('',#5496,.T.) ;
#3669 = FACE_OUTER_BOUND('',#5497,.T.) ;
#3670 = FACE_OUTER_BOUND('',#5498,.T.) ;
#3671 = FACE_OUTER_BOUND('',#5499,.T.) ;
#3672 = FACE_OUTER_BOUND('',#5500,.T.) ;
#3673 = FACE_OUTER_BOUND('',#5501,.T.) ;
#3674 = FACE_OUTER_BOUND('',#5502,.T.) ;
#3675 = FACE_OUTER_BOUND('',#5503,.T.) ;
#3676 = FACE_OUTER_BOUND('',#5504,.T.) ;
#3677 = FACE_OUTER_BOUND('',#5505,.T.) ;
#3678 = FACE_OUTER_BOUND('',#5506,.T.) ;
#3679 = FACE_OUTER_BOUND('',#5507,.T.) ;
#3680 = FACE_OUTER_BOUND('',#5508,.T.) ;
#3681 = FACE_OUTER_BOUND('',#5509,.T.) ;
#3682 = FACE_OUTER_BOUND('',#5510,.T.) ;
#3683 = FACE_OUTER_BOUND('',#5511,.T.) ;
#3684 = FACE_OUTER_BOUND('',#5512,.T.) ;
#3685 = FACE_OUTER_BOUND('',#5513,.T.) ;
#3686 = FACE_OUTER_BOUND('',#5514,.T.) ;
#3687 = FACE_OUTER_BOUND('',#5515,.T.) ;
#3688 = FACE_OUTER_BOUND('',#5516,.T.) ;
#3689 = FACE_OUTER_BOUND('',#5517,.T.) ;
#3690 = FACE_OUTER_BOUND('',#5518,.T.) ;
#3691 = FACE_OUTER_BOUND('',#5519,.T.) ;
#3692 = FACE_OUTER_BOUND('',#5520,.T.) ;
#3693 = FACE_OUTER_BOUND('',#5521,.T.) ;
#3694 = FACE_OUTER_BOUND('',#5522,.T.) ;
#3695 = FACE_OUTER_BOUND('',#5523,.T.) ;
#3696 = FACE_OUTER_BOUND('',#5524,.T.) ;
#3697 = FACE_OUTER_BOUND('',#5525,.T.) ;
#3698 = FACE_OUTER_BOUND('',#5526,.T.) ;
#3699 = FACE_OUTER_BOUND('',#5527,.T.) ;
#3700 = FACE_OUTER_BOUND('',#5528,.T.) ;
#3701 = FACE_OUTER_BOUND('',#5529,.T.) ;
#3702 = FACE_OUTER_BOUND('',#5530,.T.) ;
#3703 = FACE_OUTER_BOUND('',#5531,.T.) ;
#3704 = FACE_OUTER_BOUND('',#5532,.T.) ;
#3705 = FACE_OUTER_BOUND('',#5533,.T.) ;
#3706 = FACE_OUTER_BOUND('',#5534,.T.) ;
#3707 = FACE_OUTER_BOUND('',#5535,.T.) ;
#3708 = FACE_OUTER_BOUND('',#5536,.T.) ;
#3709 = FACE_OUTER_BOUND('',#5537,.T.) ;
#3710 = FACE_OUTER_BOUND('',#5538,.T.) ;
#3711 = FACE_OUTER_BOUND('',#5539,.T.) ;
#3712 = FACE_OUTER_BOUND('',#5540,.T.) ;
#3713 = FACE_OUTER_BOUND('',#5541,.T.) ;
#3714 = FACE_OUTER_BOUND('',#5542,.T.) ;
#3715 = FACE_OUTER_BOUND('',#5543,.T.) ;
#3716 = FACE_OUTER_BOUND('',#5544,.T.) ;
#3717 = FACE_OUTER_BOUND('',#5545,.T.) ;
#3718 = FACE_OUTER_BOUND('',#5546,.T.) ;
#3719 = FACE_OUTER_BOUND('',#5547,.T.) ;
#3720 = FACE_OUTER_BOUND('',#5548,.T.) ;
#3721 = FACE_OUTER_BOUND('',#5549,.T.) ;
#3722 = FACE_OUTER_BOUND('',#5550,.T.) ;
#3723 = FACE_OUTER_BOUND('',#5551,.T.) ;
#3724 = FACE_OUTER_BOUND('',#5552,.T.) ;
#3725 = FACE_OUTER_BOUND('',#5553,.T.) ;
#3726 = FACE_OUTER_BOUND('',#5554,.T.) ;
#3727 = FACE_OUTER_BOUND('',#5555,.T.) ;
#3728 = FACE_OUTER_BOUND('',#5556,.T.) ;
#3729 = FACE_OUTER_BOUND('',#5557,.T.) ;
#3730 = FACE_OUTER_BOUND('',#5558,.T.) ;
#3731 = FACE_OUTER_BOUND('',#5559,.T.) ;
#3732 = FACE_OUTER_BOUND('',#5560,.T.) ;
#3733 = FACE_OUTER_BOUND('',#5561,.T.) ;
#3734 = FACE_OUTER_BOUND('',#5562,.T.) ;
#3735 = FACE_OUTER_BOUND('',#5563,.T.) ;
#3736 = FACE_OUTER_BOUND('',#5564,.T.) ;
#3737 = FACE_OUTER_BOUND('',#5565,.T.) ;
#3738 = FACE_OUTER_BOUND('',#5566,.T.) ;
#3739 = FACE_OUTER_BOUND('',#5567,.T.) ;
#3740 = FACE_OUTER_BOUND('',#5568,.T.) ;
#3741 = FACE_OUTER_BOUND('',#5569,.T.) ;
#3742 = FACE_OUTER_BOUND('',#5570,.T.) ;
#3743 = FACE_OUTER_BOUND('',#5571,.T.) ;
#3744 = FACE_OUTER_BOUND('',#5572,.T.) ;
#3745 = FACE_OUTER_BOUND('',#5573,.T.) ;
#3746 = FACE_OUTER_BOUND('',#5574,.T.) ;
#3747 = FACE_OUTER_BOUND('',#5575,.T.) ;
#3748 = FACE_OUTER_BOUND('',#5576,.T.) ;
#3749 = FACE_OUTER_BOUND('',#5578,.T.) ;
#3750 = FACE_OUTER_BOUND('',#5580,.T.) ;
#3751 = FACE_OUTER_BOUND('',#5581,.T.) ;
#3752 = FACE_OUTER_BOUND('',#5582,.T.) ;
#3753 = FACE_OUTER_BOUND('',#5583,.T.) ;
#3754 = FACE_OUTER_BOUND('',#5584,.T.) ;
#3755 = FACE_OUTER_BOUND('',#5585,.T.) ;
#3756 = FACE_OUTER_BOUND('',#5586,.T.) ;
#3757 = FACE_OUTER_BOUND('',#5588,.T.) ;
#3758 = FACE_OUTER_BOUND('',#5589,.T.) ;
#3759 = FACE_OUTER_BOUND('',#5590,.T.) ;
#3760 = FACE_OUTER_BOUND('',#5592,.T.) ;
#3761 = FACE_OUTER_BOUND('',#5593,.T.) ;
#3762 = FACE_OUTER_BOUND('',#5594,.T.) ;
#3763 = FACE_OUTER_BOUND('',#5595,.T.) ;
#3764 = FACE_OUTER_BOUND('',#5596,.T.) ;
#3765 = FACE_OUTER_BOUND('',#5597,.T.) ;
#3766 = FACE_OUTER_BOUND('',#5598,.T.) ;
#3767 = FACE_OUTER_BOUND('',#5599,.T.) ;
#3768 = FACE_OUTER_BOUND('',#5600,.T.) ;
#3769 = FACE_OUTER_BOUND('',#5601,.T.) ;
#3770 = FACE_OUTER_BOUND('',#5602,.T.) ;
#3771 = FACE_OUTER_BOUND('',#5603,.T.) ;
#3772 = FACE_OUTER_BOUND('',#5604,.T.) ;
#3773 = FACE_OUTER_BOUND('',#5606,.T.) ;
#3774 = FACE_OUTER_BOUND('',#5607,.T.) ;
#3775 = FACE_OUTER_BOUND('',#5608,.T.) ;
#3776 = FACE_OUTER_BOUND('',#5609,.T.) ;
#3777 = FACE_OUTER_BOUND('',#5610,.T.) ;
#3778 = FACE_OUTER_BOUND('',#5611,.T.) ;
#3779 = FACE_OUTER_BOUND('',#5613,.T.) ;
#3780 = FACE_OUTER_BOUND('',#5614,.T.) ;
#3781 = FACE_OUTER_BOUND('',#5615,.T.) ;
#3782 = FACE_OUTER_BOUND('',#5616,.T.) ;
#3783 = FACE_OUTER_BOUND('',#5617,.T.) ;
#3784 = FACE_OUTER_BOUND('',#5619,.T.) ;
#3785 = FACE_OUTER_BOUND('',#5620,.T.) ;
#3786 = FACE_OUTER_BOUND('',#5621,.T.) ;
#3787 = FACE_OUTER_BOUND('',#5623,.T.) ;
#3788 = FACE_OUTER_BOUND('',#5625,.T.) ;
#3789 = FACE_OUTER_BOUND('',#5627,.T.) ;
#3790 = FACE_OUTER_BOUND('',#5628,.T.) ;
#3791 = FACE_OUTER_BOUND('',#5629,.T.) ;
#3792 = FACE_OUTER_BOUND('',#5630,.T.) ;
#3793 = FACE_OUTER_BOUND('',#5631,.T.) ;
#3794 = FACE_OUTER_BOUND('',#5633,.T.) ;
#3795 = FACE_OUTER_BOUND('',#5635,.T.) ;
#3796 = FACE_OUTER_BOUND('',#5636,.T.) ;
#3797 = FACE_OUTER_BOUND('',#5637,.T.) ;
#3798 = FACE_OUTER_BOUND('',#5638,.T.) ;
#3799 = FACE_OUTER_BOUND('',#5639,.T.) ;
#3800 = FACE_OUTER_BOUND('',#5640,.T.) ;
#3801 = FACE_OUTER_BOUND('',#5641,.T.) ;
#3802 = FACE_OUTER_BOUND('',#5642,.T.) ;
#3803 = FACE_OUTER_BOUND('',#5643,.T.) ;
#3804 = FACE_OUTER_BOUND('',#5644,.T.) ;
#3805 = FACE_OUTER_BOUND('',#5645,.T.) ;
#3806 = FACE_OUTER_BOUND('',#5646,.T.) ;
#3807 = FACE_OUTER_BOUND('',#5647,.T.) ;
#3808 = FACE_OUTER_BOUND('',#5648,.T.) ;
#3809 = FACE_OUTER_BOUND('',#5649,.T.) ;
#3810 = FACE_OUTER_BOUND('',#5650,.T.) ;
#3811 = FACE_OUTER_BOUND('',#5651,.T.) ;
#3812 = FACE_OUTER_BOUND('',#5652,.T.) ;
#3813 = FACE_OUTER_BOUND('',#5653,.T.) ;
#3814 = FACE_OUTER_BOUND('',#5654,.T.) ;
#3815 = FACE_OUTER_BOUND('',#5655,.T.) ;
#3816 = FACE_OUTER_BOUND('',#5657,.T.) ;
#3817 = FACE_OUTER_BOUND('',#5658,.T.) ;
#3818 = FACE_OUTER_BOUND('',#5659,.T.) ;
#3819 = FACE_OUTER_BOUND('',#5661,.T.) ;
#3820 = FACE_OUTER_BOUND('',#5662,.T.) ;
#3821 = FACE_OUTER_BOUND('',#5663,.T.) ;
#3822 = FACE_OUTER_BOUND('',#5664,.T.) ;
#3823 = FACE_OUTER_BOUND('',#5665,.T.) ;
#3824 = FACE_OUTER_BOUND('',#5666,.T.) ;
#3825 = FACE_OUTER_BOUND('',#5667,.T.) ;
#3826 = FACE_OUTER_BOUND('',#5668,.T.) ;
#3827 = FACE_OUTER_BOUND('',#5669,.T.) ;
#3828 = FACE_OUTER_BOUND('',#5670,.T.) ;
#3829 = FACE_OUTER_BOUND('',#5672,.T.) ;
#3830 = FACE_OUTER_BOUND('',#5673,.T.) ;
#3831 = FACE_OUTER_BOUND('',#5674,.T.) ;
#3832 = FACE_OUTER_BOUND('',#5675,.T.) ;
#3833 = FACE_OUTER_BOUND('',#5677,.T.) ;
#3834 = FACE_OUTER_BOUND('',#5678,.T.) ;
#3835 = FACE_OUTER_BOUND('',#5679,.T.) ;
#3836 = FACE_OUTER_BOUND('',#5680,.T.) ;
#3837 = FACE_OUTER_BOUND('',#5681,.T.) ;
#3838 = FACE_OUTER_BOUND('',#5683,.T.) ;
#3839 = FACE_OUTER_BOUND('',#5684,.T.) ;
#3840 = FACE_OUTER_BOUND('',#5685,.T.) ;
#3841 = FACE_OUTER_BOUND('',#5686,.T.) ;
#3842 = FACE_OUTER_BOUND('',#5687,.T.) ;
#3843 = FACE_OUTER_BOUND('',#5688,.T.) ;
#3844 = FACE_OUTER_BOUND('',#5689,.T.) ;
#3845 = FACE_OUTER_BOUND('',#5690,.T.) ;
#3846 = FACE_OUTER_BOUND('',#5691,.T.) ;
#3847 = FACE_OUTER_BOUND('',#5692,.T.) ;
#3848 = FACE_OUTER_BOUND('',#5694,.T.) ;
#3849 = FACE_OUTER_BOUND('',#5695,.T.) ;
#3850 = FACE_OUTER_BOUND('',#5696,.T.) ;
#3851 = FACE_OUTER_BOUND('',#5697,.T.) ;
#3852 = FACE_OUTER_BOUND('',#5699,.T.) ;
#3853 = FACE_OUTER_BOUND('',#5700,.T.) ;
#3854 = FACE_OUTER_BOUND('',#5701,.T.) ;
#3855 = FACE_OUTER_BOUND('',#5702,.T.) ;
#3856 = FACE_OUTER_BOUND('',#5703,.T.) ;
#3857 = FACE_OUTER_BOUND('',#5705,.T.) ;
#3858 = FACE_OUTER_BOUND('',#5707,.T.) ;
#3859 = FACE_OUTER_BOUND('',#5708,.T.) ;
#3860 = FACE_OUTER_BOUND('',#5709,.T.) ;
#3861 = FACE_OUTER_BOUND('',#5710,.T.) ;
#3862 = FACE_OUTER_BOUND('',#5711,.T.) ;
#3863 = FACE_OUTER_BOUND('',#5713,.T.) ;
#3864 = FACE_OUTER_BOUND('',#5714,.T.) ;
#3865 = FACE_OUTER_BOUND('',#5715,.T.) ;
#3866 = FACE_OUTER_BOUND('',#5716,.T.) ;
#3867 = FACE_OUTER_BOUND('',#5717,.T.) ;
#3868 = FACE_OUTER_BOUND('',#5718,.T.) ;
#3869 = FACE_OUTER_BOUND('',#5719,.T.) ;
#3870 = FACE_OUTER_BOUND('',#5720,.T.) ;
#3871 = FACE_OUTER_BOUND('',#5721,.T.) ;
#3872 = FACE_OUTER_BOUND('',#5722,.T.) ;
#3873 = FACE_OUTER_BOUND('',#5723,.T.) ;
#3874 = FACE_OUTER_BOUND('',#5724,.T.) ;
#3875 = FACE_OUTER_BOUND('',#5725,.T.) ;
#3876 = FACE_OUTER_BOUND('',#5726,.T.) ;
#3877 = FACE_OUTER_BOUND('',#5727,.T.) ;
#3878 = FACE_OUTER_BOUND('',#5728,.T.) ;
#3879 = FACE_OUTER_BOUND('',#5729,.T.) ;
#3880 = FACE_OUTER_BOUND('',#5730,.T.) ;
#3881 = FACE_OUTER_BOUND('',#5731,.T.) ;
#3882 = FACE_OUTER_BOUND('',#5732,.T.) ;
#3883 = FACE_OUTER_BOUND('',#5733,.T.) ;
#3884 = FACE_OUTER_BOUND('',#5734,.T.) ;
#3885 = FACE_OUTER_BOUND('',#5735,.T.) ;
#3886 = FACE_OUTER_BOUND('',#5736,.T.) ;
#3887 = FACE_OUTER_BOUND('',#5737,.T.) ;
#3888 = FACE_OUTER_BOUND('',#5738,.T.) ;
#3889 = FACE_OUTER_BOUND('',#5739,.T.) ;
#3890 = FACE_OUTER_BOUND('',#5740,.T.) ;
#3891 = FACE_OUTER_BOUND('',#5741,.T.) ;
#3892 = FACE_OUTER_BOUND('',#5742,.T.) ;
#3893 = FACE_OUTER_BOUND('',#5743,.T.) ;
#3894 = EDGE_LOOP('',(#18591,#18592,#18593,#18594)) ;
#3895 = EDGE_LOOP('',(#18595,#18596,#18597,#18598,#18599,#18600,#18601,#18602)) ;
#3896 = EDGE_LOOP('',(#18603)) ;
#3897 = EDGE_LOOP('',(#18604,#18605,#18606,#18607)) ;
#3898 = EDGE_LOOP('',(#18608,#18609,#18610,#18611)) ;
#3899 = EDGE_LOOP('',(#18612,#18613,#18614,#18615)) ;
#3900 = EDGE_LOOP('',(#18616,#18617,#18618,#18619)) ;
#3901 = EDGE_LOOP('',(#18620,#18621,#18622,#18623)) ;
#3902 = EDGE_LOOP('',(#18624,#18625,#18626,#18627,#18628,#18629,#18630,#18631)) ;
#3903 = EDGE_LOOP('',(#18632)) ;
#3904 = EDGE_LOOP('',(#18633,#18634,#18635,#18636)) ;
#3905 = EDGE_LOOP('',(#18637,#18638,#18639,#18640,#18641,#18642,#18643,#18644,
#18645,#18646,#18647,#18648)) ;
#3906 = EDGE_LOOP('',(#18649,#18650,#18651,#18652)) ;
#3907 = EDGE_LOOP('',(#18653,#18654,#18655,#18656,#18657,#18658,#18659,#18660)) ;
#3908 = EDGE_LOOP('',(#18661)) ;
#3909 = EDGE_LOOP('',(#18662,#18663,#18664,#18665)) ;
#3910 = EDGE_LOOP('',(#18666,#18667,#18668,#18669)) ;
#3911 = EDGE_LOOP('',(#18670,#18671,#18672,#18673)) ;
#3912 = EDGE_LOOP('',(#18674,#18675,#18676,#18677)) ;
#3913 = EDGE_LOOP('',(#18678,#18679,#18680,#18681)) ;
#3914 = EDGE_LOOP('',(#18682,#18683,#18684,#18685,#18686,#18687,#18688,#18689)) ;
#3915 = EDGE_LOOP('',(#18690)) ;
#3916 = EDGE_LOOP('',(#18691,#18692,#18693,#18694)) ;
#3917 = EDGE_LOOP('',(#18695,#18696,#18697,#18698)) ;
#3918 = EDGE_LOOP('',(#18699,#18700,#18701,#18702)) ;
#3919 = EDGE_LOOP('',(#18703,#18704,#18705,#18706)) ;
#3920 = EDGE_LOOP('',(#18707,#18708,#18709,#18710)) ;
#3921 = EDGE_LOOP('',(#18711,#18712,#18713,#18714)) ;
#3922 = EDGE_LOOP('',(#18715,#18716,#18717,#18718)) ;
#3923 = EDGE_LOOP('',(#18719,#18720,#18721,#18722)) ;
#3924 = EDGE_LOOP('',(#18723,#18724,#18725,#18726)) ;
#3925 = EDGE_LOOP('',(#18727,#18728,#18729,#18730)) ;
#3926 = EDGE_LOOP('',(#18731,#18732,#18733,#18734)) ;
#3927 = EDGE_LOOP('',(#18735,#18736,#18737,#18738)) ;
#3928 = EDGE_LOOP('',(#18739,#18740,#18741,#18742)) ;
#3929 = EDGE_LOOP('',(#18743,#18744,#18745,#18746)) ;
#3930 = EDGE_LOOP('',(#18747,#18748,#18749,#18750)) ;
#3931 = EDGE_LOOP('',(#18751,#18752,#18753,#18754)) ;
#3932 = EDGE_LOOP('',(#18755,#18756,#18757,#18758)) ;
#3933 = EDGE_LOOP('',(#18759,#18760,#18761,#18762)) ;
#3934 = EDGE_LOOP('',(#18763,#18764,#18765,#18766)) ;
#3935 = EDGE_LOOP('',(#18767,#18768,#18769,#18770)) ;
#3936 = EDGE_LOOP('',(#18771,#18772,#18773,#18774)) ;
#3937 = EDGE_LOOP('',(#18775,#18776,#18777,#18778)) ;
#3938 = EDGE_LOOP('',(#18779,#18780,#18781,#18782)) ;
#3939 = EDGE_LOOP('',(#18783,#18784,#18785,#18786)) ;
#3940 = EDGE_LOOP('',(#18787,#18788,#18789,#18790)) ;
#3941 = EDGE_LOOP('',(#18791,#18792,#18793,#18794)) ;
#3942 = EDGE_LOOP('',(#18795,#18796,#18797,#18798)) ;
#3943 = EDGE_LOOP('',(#18799,#18800,#18801,#18802)) ;
#3944 = EDGE_LOOP('',(#18803,#18804,#18805,#18806)) ;
#3945 = EDGE_LOOP('',(#18807,#18808,#18809,#18810)) ;
#3946 = EDGE_LOOP('',(#18811,#18812,#18813,#18814)) ;
#3947 = EDGE_LOOP('',(#18815,#18816,#18817,#18818)) ;
#3948 = EDGE_LOOP('',(#18819,#18820,#18821,#18822)) ;
#3949 = EDGE_LOOP('',(#18823,#18824,#18825,#18826)) ;
#3950 = EDGE_LOOP('',(#18827,#18828,#18829,#18830)) ;
#3951 = EDGE_LOOP('',(#18831,#18832,#18833,#18834)) ;
#3952 = EDGE_LOOP('',(#18835,#18836,#18837,#18838)) ;
#3953 = EDGE_LOOP('',(#18839,#18840,#18841,#18842)) ;
#3954 = EDGE_LOOP('',(#18843,#18844,#18845,#18846)) ;
#3955 = EDGE_LOOP('',(#18847,#18848,#18849,#18850)) ;
#3956 = EDGE_LOOP('',(#18851,#18852,#18853,#18854)) ;
#3957 = EDGE_LOOP('',(#18855,#18856,#18857,#18858)) ;
#3958 = EDGE_LOOP('',(#18859,#18860,#18861,#18862)) ;
#3959 = EDGE_LOOP('',(#18863,#18864,#18865,#18866,#18867,#18868,#18869,#18870,
#18871)) ;
#3960 = EDGE_LOOP('',(#18872)) ;
#3961 = EDGE_LOOP('',(#18873)) ;
#3962 = EDGE_LOOP('',(#18874)) ;
#3963 = EDGE_LOOP('',(#18875,#18876,#18877,#18878)) ;
#3964 = EDGE_LOOP('',(#18879,#18880,#18881,#18882)) ;
#3965 = EDGE_LOOP('',(#18883,#18884,#18885,#18886)) ;
#3966 = EDGE_LOOP('',(#18887,#18888,#18889,#18890)) ;
#3967 = EDGE_LOOP('',(#18891,#18892,#18893,#18894)) ;
#3968 = EDGE_LOOP('',(#18895,#18896,#18897,#18898)) ;
#3969 = EDGE_LOOP('',(#18899,#18900,#18901,#18902)) ;
#3970 = EDGE_LOOP('',(#18903,#18904,#18905,#18906)) ;
#3971 = EDGE_LOOP('',(#18907,#18908,#18909,#18910)) ;
#3972 = EDGE_LOOP('',(#18911,#18912,#18913,#18914)) ;
#3973 = EDGE_LOOP('',(#18915)) ;
#3974 = EDGE_LOOP('',(#18916)) ;
#3975 = EDGE_LOOP('',(#18917,#18918,#18919,#18920)) ;
#3976 = EDGE_LOOP('',(#18921,#18922,#18923,#18924)) ;
#3977 = EDGE_LOOP('',(#18925,#18926,#18927,#18928)) ;
#3978 = EDGE_LOOP('',(#18929,#18930,#18931,#18932,#18933,#18934,#18935,#18936)) ;
#3979 = EDGE_LOOP('',(#18937,#18938,#18939,#18940,#18941,#18942,#18943,#18944)) ;
#3980 = EDGE_LOOP('',(#18945,#18946,#18947,#18948)) ;
#3981 = EDGE_LOOP('',(#18949,#18950,#18951,#18952)) ;
#3982 = EDGE_LOOP('',(#18953,#18954,#18955,#18956)) ;
#3983 = EDGE_LOOP('',(#18957,#18958,#18959,#18960)) ;
#3984 = EDGE_LOOP('',(#18961)) ;
#3985 = EDGE_LOOP('',(#18962)) ;
#3986 = EDGE_LOOP('',(#18963,#18964,#18965,#18966)) ;
#3987 = EDGE_LOOP('',(#18967)) ;
#3988 = EDGE_LOOP('',(#18968)) ;
#3989 = EDGE_LOOP('',(#18969,#18970,#18971,#18972)) ;
#3990 = EDGE_LOOP('',(#18973,#18974,#18975,#18976)) ;
#3991 = EDGE_LOOP('',(#18977,#18978,#18979,#18980)) ;
#3992 = EDGE_LOOP('',(#18981,#18982,#18983,#18984)) ;
#3993 = EDGE_LOOP('',(#18985,#18986,#18987,#18988)) ;
#3994 = EDGE_LOOP('',(#18989,#18990,#18991,#18992)) ;
#3995 = EDGE_LOOP('',(#18993,#18994,#18995,#18996)) ;
#3996 = EDGE_LOOP('',(#18997,#18998,#18999,#19000)) ;
#3997 = EDGE_LOOP('',(#19001,#19002,#19003,#19004)) ;
#3998 = EDGE_LOOP('',(#19005,#19006,#19007,#19008)) ;
#3999 = EDGE_LOOP('',(#19009,#19010,#19011,#19012)) ;
#4000 = EDGE_LOOP('',(#19013,#19014,#19015,#19016)) ;
#4001 = EDGE_LOOP('',(#19017,#19018,#19019,#19020)) ;
#4002 = EDGE_LOOP('',(#19021,#19022,#19023,#19024)) ;
#4003 = EDGE_LOOP('',(#19025,#19026,#19027,#19028)) ;
#4004 = EDGE_LOOP('',(#19029,#19030,#19031,#19032)) ;
#4005 = EDGE_LOOP('',(#19033,#19034,#19035,#19036)) ;
#4006 = EDGE_LOOP('',(#19037,#19038,#19039,#19040)) ;
#4007 = EDGE_LOOP('',(#19041,#19042,#19043,#19044)) ;
#4008 = EDGE_LOOP('',(#19045,#19046,#19047,#19048)) ;
#4009 = EDGE_LOOP('',(#19049,#19050,#19051,#19052)) ;
#4010 = EDGE_LOOP('',(#19053,#19054,#19055,#19056)) ;
#4011 = EDGE_LOOP('',(#19057,#19058,#19059,#19060)) ;
#4012 = EDGE_LOOP('',(#19061,#19062,#19063,#19064)) ;
#4013 = EDGE_LOOP('',(#19065,#19066,#19067,#19068)) ;
#4014 = EDGE_LOOP('',(#19069,#19070,#19071,#19072)) ;
#4015 = EDGE_LOOP('',(#19073,#19074,#19075,#19076)) ;
#4016 = EDGE_LOOP('',(#19077,#19078,#19079,#19080)) ;
#4017 = EDGE_LOOP('',(#19081,#19082,#19083,#19084)) ;
#4018 = EDGE_LOOP('',(#19085,#19086,#19087,#19088)) ;
#4019 = EDGE_LOOP('',(#19089,#19090,#19091,#19092)) ;
#4020 = EDGE_LOOP('',(#19093,#19094,#19095,#19096)) ;
#4021 = EDGE_LOOP('',(#19097,#19098,#19099,#19100)) ;
#4022 = EDGE_LOOP('',(#19101,#19102,#19103,#19104,#19105,#19106,#19107,#19108,
#19109,#19110,#19111,#19112,#19113,#19114,#19115,#19116,#19117,#19118,#19119,
#19120,#19121,#19122,#19123,#19124,#19125,#19126,#19127,#19128,#19129,#19130,
#19131,#19132,#19133,#19134,#19135,#19136,#19137,#19138,#19139,#19140,#19141,
#19142,#19143,#19144,#19145,#19146,#19147,#19148,#19149,#19150,#19151,#19152,
#19153,#19154,#19155,#19156,#19157,#19158,#19159,#19160,#19161,#19162,#19163,
#19164,#19165,#19166,#19167,#19168,#19169,#19170,#19171,#19172,#19173,#19174,
#19175,#19176,#19177,#19178,#19179,#19180,#19181,#19182,#19183,#19184,#19185,
#19186,#19187,#19188)) ;
#4023 = EDGE_LOOP('',(#19189,#19190,#19191)) ;
#4024 = EDGE_LOOP('',(#19192,#19193,#19194,#19195)) ;
#4025 = EDGE_LOOP('',(#19196,#19197,#19198,#19199)) ;
#4026 = EDGE_LOOP('',(#19200,#19201,#19202)) ;
#4027 = EDGE_LOOP('',(#19203,#19204,#19205,#19206)) ;
#4028 = EDGE_LOOP('',(#19207,#19208,#19209,#19210)) ;
#4029 = EDGE_LOOP('',(#19211,#19212,#19213,#19214)) ;
#4030 = EDGE_LOOP('',(#19215,#19216,#19217,#19218)) ;
#4031 = EDGE_LOOP('',(#19219,#19220,#19221,#19222,#19223)) ;
#4032 = EDGE_LOOP('',(#19224,#19225,#19226)) ;
#4033 = EDGE_LOOP('',(#19227,#19228,#19229,#19230)) ;
#4034 = EDGE_LOOP('',(#19231,#19232,#19233,#19234)) ;
#4035 = EDGE_LOOP('',(#19235,#19236,#19237,#19238)) ;
#4036 = EDGE_LOOP('',(#19239,#19240,#19241,#19242)) ;
#4037 = EDGE_LOOP('',(#19243,#19244,#19245,#19246)) ;
#4038 = EDGE_LOOP('',(#19247,#19248,#19249,#19250)) ;
#4039 = EDGE_LOOP('',(#19251,#19252,#19253,#19254,#19255)) ;
#4040 = EDGE_LOOP('',(#19256,#19257,#19258)) ;
#4041 = EDGE_LOOP('',(#19259,#19260,#19261,#19262)) ;
#4042 = EDGE_LOOP('',(#19263,#19264,#19265,#19266)) ;
#4043 = EDGE_LOOP('',(#19267,#19268,#19269,#19270)) ;
#4044 = EDGE_LOOP('',(#19271,#19272,#19273,#19274)) ;
#4045 = EDGE_LOOP('',(#19275,#19276,#19277,#19278)) ;
#4046 = EDGE_LOOP('',(#19279,#19280,#19281,#19282)) ;
#4047 = EDGE_LOOP('',(#19283,#19284,#19285,#19286)) ;
#4048 = EDGE_LOOP('',(#19287,#19288,#19289,#19290)) ;
#4049 = EDGE_LOOP('',(#19291,#19292,#19293,#19294)) ;
#4050 = EDGE_LOOP('',(#19295,#19296,#19297)) ;
#4051 = EDGE_LOOP('',(#19298,#19299,#19300,#19301,#19302)) ;
#4052 = EDGE_LOOP('',(#19303,#19304,#19305)) ;
#4053 = EDGE_LOOP('',(#19306,#19307,#19308,#19309)) ;
#4054 = EDGE_LOOP('',(#19310,#19311,#19312)) ;
#4055 = EDGE_LOOP('',(#19313,#19314,#19315,#19316)) ;
#4056 = EDGE_LOOP('',(#19317,#19318,#19319,#19320)) ;
#4057 = EDGE_LOOP('',(#19321,#19322,#19323,#19324)) ;
#4058 = EDGE_LOOP('',(#19325,#19326,#19327,#19328)) ;
#4059 = EDGE_LOOP('',(#19329,#19330,#19331,#19332)) ;
#4060 = EDGE_LOOP('',(#19333,#19334,#19335,#19336)) ;
#4061 = EDGE_LOOP('',(#19337,#19338,#19339,#19340)) ;
#4062 = EDGE_LOOP('',(#19341,#19342,#19343)) ;
#4063 = EDGE_LOOP('',(#19344,#19345,#19346,#19347)) ;
#4064 = EDGE_LOOP('',(#19348,#19349,#19350,#19351)) ;
#4065 = EDGE_LOOP('',(#19352,#19353,#19354,#19355)) ;
#4066 = EDGE_LOOP('',(#19356,#19357,#19358,#19359)) ;
#4067 = EDGE_LOOP('',(#19360,#19361,#19362,#19363)) ;
#4068 = EDGE_LOOP('',(#19364,#19365,#19366,#19367)) ;
#4069 = EDGE_LOOP('',(#19368,#19369,#19370,#19371)) ;
#4070 = EDGE_LOOP('',(#19372,#19373,#19374,#19375)) ;
#4071 = EDGE_LOOP('',(#19376,#19377,#19378,#19379)) ;
#4072 = EDGE_LOOP('',(#19380,#19381,#19382,#19383)) ;
#4073 = EDGE_LOOP('',(#19384,#19385,#19386,#19387)) ;
#4074 = EDGE_LOOP('',(#19388,#19389,#19390,#19391,#19392)) ;
#4075 = EDGE_LOOP('',(#19393,#19394,#19395,#19396)) ;
#4076 = EDGE_LOOP('',(#19397,#19398,#19399,#19400,#19401,#19402,#19403,#19404,
#19405,#19406,#19407,#19408,#19409,#19410,#19411,#19412,#19413,#19414,#19415,
#19416,#19417,#19418,#19419,#19420,#19421,#19422,#19423,#19424,#19425,#19426,
#19427,#19428,#19429,#19430,#19431,#19432,#19433,#19434,#19435,#19436,#19437,
#19438,#19439,#19440,#19441,#19442,#19443,#19444,#19445,#19446,#19447,#19448,
#19449,#19450,#19451,#19452,#19453,#19454,#19455,#19456,#19457,#19458,#19459,
#19460,#19461,#19462,#19463,#19464,#19465,#19466,#19467,#19468,#19469,#19470,
#19471,#19472,#19473,#19474,#19475,#19476,#19477,#19478,#19479,#19480,#19481,
#19482,#19483,#19484)) ;
#4077 = EDGE_LOOP('',(#19485,#19486,#19487,#19488)) ;
#4078 = EDGE_LOOP('',(#19489,#19490,#19491,#19492)) ;
#4079 = EDGE_LOOP('',(#19493,#19494,#19495,#19496)) ;
#4080 = EDGE_LOOP('',(#19497,#19498,#19499,#19500)) ;
#4081 = EDGE_LOOP('',(#19501,#19502,#19503,#19504,#19505)) ;
#4082 = EDGE_LOOP('',(#19506,#19507,#19508,#19509)) ;
#4083 = EDGE_LOOP('',(#19510,#19511,#19512,#19513)) ;
#4084 = EDGE_LOOP('',(#19514,#19515,#19516)) ;
#4085 = EDGE_LOOP('',(#19517,#19518,#19519,#19520,#19521)) ;
#4086 = EDGE_LOOP('',(#19522,#19523,#19524)) ;
#4087 = EDGE_LOOP('',(#19525,#19526,#19527,#19528,#19529)) ;
#4088 = EDGE_LOOP('',(#19530,#19531,#19532,#19533)) ;
#4089 = EDGE_LOOP('',(#19534,#19535,#19536,#19537)) ;
#4090 = EDGE_LOOP('',(#19538,#19539,#19540,#19541)) ;
#4091 = EDGE_LOOP('',(#19542,#19543,#19544,#19545)) ;
#4092 = EDGE_LOOP('',(#19546,#19547,#19548)) ;
#4093 = EDGE_LOOP('',(#19549,#19550,#19551,#19552)) ;
#4094 = EDGE_LOOP('',(#19553,#19554,#19555,#19556)) ;
#4095 = EDGE_LOOP('',(#19557,#19558,#19559,#19560)) ;
#4096 = EDGE_LOOP('',(#19561,#19562,#19563,#19564)) ;
#4097 = EDGE_LOOP('',(#19565,#19566,#19567,#19568)) ;
#4098 = EDGE_LOOP('',(#19569,#19570,#19571,#19572)) ;
#4099 = EDGE_LOOP('',(#19573,#19574,#19575,#19576)) ;
#4100 = EDGE_LOOP('',(#19577,#19578,#19579,#19580)) ;
#4101 = EDGE_LOOP('',(#19581,#19582,#19583,#19584,#19585)) ;
#4102 = EDGE_LOOP('',(#19586,#19587,#19588)) ;
#4103 = EDGE_LOOP('',(#19589,#19590,#19591,#19592)) ;
#4104 = EDGE_LOOP('',(#19593,#19594,#19595)) ;
#4105 = EDGE_LOOP('',(#19596,#19597,#19598,#19599)) ;
#4106 = EDGE_LOOP('',(#19600,#19601,#19602,#19603)) ;
#4107 = EDGE_LOOP('',(#19604,#19605,#19606,#19607)) ;
#4108 = EDGE_LOOP('',(#19608,#19609,#19610,#19611)) ;
#4109 = EDGE_LOOP('',(#19612,#19613,#19614,#19615)) ;
#4110 = EDGE_LOOP('',(#19616,#19617,#19618,#19619)) ;
#4111 = EDGE_LOOP('',(#19620,#19621,#19622,#19623)) ;
#4112 = EDGE_LOOP('',(#19624,#19625,#19626,#19627)) ;
#4113 = EDGE_LOOP('',(#19628,#19629,#19630,#19631)) ;
#4114 = EDGE_LOOP('',(#19632,#19633,#19634)) ;
#4115 = EDGE_LOOP('',(#19635,#19636,#19637,#19638)) ;
#4116 = EDGE_LOOP('',(#19639,#19640,#19641,#19642)) ;
#4117 = EDGE_LOOP('',(#19643,#19644,#19645,#19646)) ;
#4118 = EDGE_LOOP('',(#19647,#19648,#19649,#19650)) ;
#4119 = EDGE_LOOP('',(#19651,#19652,#19653,#19654)) ;
#4120 = EDGE_LOOP('',(#19655,#19656,#19657,#19658)) ;
#4121 = EDGE_LOOP('',(#19659,#19660,#19661,#19662)) ;
#4122 = EDGE_LOOP('',(#19663,#19664,#19665,#19666)) ;
#4123 = EDGE_LOOP('',(#19667,#19668,#19669,#19670)) ;
#4124 = EDGE_LOOP('',(#19671,#19672,#19673)) ;
#4125 = EDGE_LOOP('',(#19674,#19675,#19676)) ;
#4126 = EDGE_LOOP('',(#19677,#19678,#19679,#19680)) ;
#4127 = EDGE_LOOP('',(#19681,#19682,#19683,#19684)) ;
#4128 = EDGE_LOOP('',(#19685,#19686,#19687,#19688)) ;
#4129 = EDGE_LOOP('',(#19689,#19690,#19691,#19692)) ;
#4130 = EDGE_LOOP('',(#19693,#19694,#19695,#19696)) ;
#4131 = EDGE_LOOP('',(#19697,#19698,#19699,#19700)) ;
#4132 = EDGE_LOOP('',(#19701,#19702,#19703,#19704)) ;
#4133 = EDGE_LOOP('',(#19705,#19706,#19707,#19708)) ;
#4134 = EDGE_LOOP('',(#19709,#19710,#19711,#19712)) ;
#4135 = EDGE_LOOP('',(#19713,#19714,#19715,#19716)) ;
#4136 = EDGE_LOOP('',(#19717,#19718,#19719,#19720)) ;
#4137 = EDGE_LOOP('',(#19721,#19722,#19723,#19724)) ;
#4138 = EDGE_LOOP('',(#19725,#19726,#19727,#19728)) ;
#4139 = EDGE_LOOP('',(#19729,#19730,#19731,#19732)) ;
#4140 = EDGE_LOOP('',(#19733,#19734,#19735,#19736)) ;
#4141 = EDGE_LOOP('',(#19737,#19738,#19739,#19740)) ;
#4142 = EDGE_LOOP('',(#19741,#19742,#19743,#19744)) ;
#4143 = EDGE_LOOP('',(#19745,#19746,#19747,#19748)) ;
#4144 = EDGE_LOOP('',(#19749,#19750,#19751,#19752)) ;
#4145 = EDGE_LOOP('',(#19753,#19754,#19755,#19756)) ;
#4146 = EDGE_LOOP('',(#19757,#19758,#19759,#19760)) ;
#4147 = EDGE_LOOP('',(#19761,#19762,#19763,#19764)) ;
#4148 = EDGE_LOOP('',(#19765,#19766,#19767,#19768)) ;
#4149 = EDGE_LOOP('',(#19769,#19770,#19771,#19772)) ;
#4150 = EDGE_LOOP('',(#19773,#19774,#19775,#19776)) ;
#4151 = EDGE_LOOP('',(#19777,#19778,#19779,#19780)) ;
#4152 = EDGE_LOOP('',(#19781,#19782,#19783,#19784)) ;
#4153 = EDGE_LOOP('',(#19785,#19786,#19787,#19788)) ;
#4154 = EDGE_LOOP('',(#19789,#19790,#19791,#19792)) ;
#4155 = EDGE_LOOP('',(#19793,#19794,#19795,#19796)) ;
#4156 = EDGE_LOOP('',(#19797,#19798,#19799,#19800)) ;
#4157 = EDGE_LOOP('',(#19801,#19802,#19803,#19804)) ;
#4158 = EDGE_LOOP('',(#19805,#19806,#19807,#19808)) ;
#4159 = EDGE_LOOP('',(#19809,#19810,#19811,#19812)) ;
#4160 = EDGE_LOOP('',(#19813,#19814,#19815,#19816)) ;
#4161 = EDGE_LOOP('',(#19817,#19818,#19819,#19820)) ;
#4162 = EDGE_LOOP('',(#19821,#19822,#19823,#19824)) ;
#4163 = EDGE_LOOP('',(#19825,#19826,#19827,#19828)) ;
#4164 = EDGE_LOOP('',(#19829,#19830,#19831,#19832)) ;
#4165 = EDGE_LOOP('',(#19833,#19834,#19835,#19836)) ;
#4166 = EDGE_LOOP('',(#19837,#19838,#19839,#19840)) ;
#4167 = EDGE_LOOP('',(#19841,#19842,#19843,#19844)) ;
#4168 = EDGE_LOOP('',(#19845,#19846,#19847,#19848)) ;
#4169 = EDGE_LOOP('',(#19849,#19850,#19851,#19852)) ;
#4170 = EDGE_LOOP('',(#19853,#19854,#19855,#19856)) ;
#4171 = EDGE_LOOP('',(#19857,#19858,#19859,#19860)) ;
#4172 = EDGE_LOOP('',(#19861,#19862,#19863,#19864)) ;
#4173 = EDGE_LOOP('',(#19865,#19866,#19867,#19868)) ;
#4174 = EDGE_LOOP('',(#19869,#19870,#19871,#19872)) ;
#4175 = EDGE_LOOP('',(#19873,#19874,#19875,#19876)) ;
#4176 = EDGE_LOOP('',(#19877,#19878,#19879,#19880)) ;
#4177 = EDGE_LOOP('',(#19881,#19882,#19883,#19884)) ;
#4178 = EDGE_LOOP('',(#19885,#19886,#19887,#19888)) ;
#4179 = EDGE_LOOP('',(#19889,#19890,#19891,#19892)) ;
#4180 = EDGE_LOOP('',(#19893,#19894,#19895,#19896)) ;
#4181 = EDGE_LOOP('',(#19897,#19898,#19899,#19900)) ;
#4182 = EDGE_LOOP('',(#19901,#19902,#19903,#19904)) ;
#4183 = EDGE_LOOP('',(#19905,#19906,#19907,#19908)) ;
#4184 = EDGE_LOOP('',(#19909,#19910,#19911,#19912)) ;
#4185 = EDGE_LOOP('',(#19913,#19914,#19915,#19916)) ;
#4186 = EDGE_LOOP('',(#19917,#19918,#19919,#19920)) ;
#4187 = EDGE_LOOP('',(#19921,#19922,#19923,#19924)) ;
#4188 = EDGE_LOOP('',(#19925,#19926,#19927,#19928)) ;
#4189 = EDGE_LOOP('',(#19929,#19930,#19931,#19932)) ;
#4190 = EDGE_LOOP('',(#19933,#19934,#19935,#19936)) ;
#4191 = EDGE_LOOP('',(#19937,#19938,#19939,#19940)) ;
#4192 = EDGE_LOOP('',(#19941,#19942,#19943,#19944)) ;
#4193 = EDGE_LOOP('',(#19945,#19946,#19947,#19948)) ;
#4194 = EDGE_LOOP('',(#19949,#19950,#19951,#19952)) ;
#4195 = EDGE_LOOP('',(#19953,#19954,#19955,#19956)) ;
#4196 = EDGE_LOOP('',(#19957,#19958,#19959,#19960)) ;
#4197 = EDGE_LOOP('',(#19961,#19962,#19963,#19964)) ;
#4198 = EDGE_LOOP('',(#19965,#19966,#19967,#19968)) ;
#4199 = EDGE_LOOP('',(#19969,#19970,#19971,#19972)) ;
#4200 = EDGE_LOOP('',(#19973,#19974,#19975,#19976)) ;
#4201 = EDGE_LOOP('',(#19977,#19978,#19979,#19980)) ;
#4202 = EDGE_LOOP('',(#19981,#19982,#19983,#19984)) ;
#4203 = EDGE_LOOP('',(#19985,#19986,#19987,#19988)) ;
#4204 = EDGE_LOOP('',(#19989,#19990,#19991,#19992)) ;
#4205 = EDGE_LOOP('',(#19993,#19994,#19995,#19996)) ;
#4206 = EDGE_LOOP('',(#19997,#19998,#19999,#20000)) ;
#4207 = EDGE_LOOP('',(#20001,#20002,#20003,#20004)) ;
#4208 = EDGE_LOOP('',(#20005,#20006,#20007,#20008)) ;
#4209 = EDGE_LOOP('',(#20009,#20010,#20011,#20012)) ;
#4210 = EDGE_LOOP('',(#20013,#20014,#20015,#20016)) ;
#4211 = EDGE_LOOP('',(#20017,#20018,#20019,#20020)) ;
#4212 = EDGE_LOOP('',(#20021,#20022,#20023,#20024)) ;
#4213 = EDGE_LOOP('',(#20025,#20026,#20027,#20028)) ;
#4214 = EDGE_LOOP('',(#20029,#20030,#20031,#20032)) ;
#4215 = EDGE_LOOP('',(#20033,#20034,#20035,#20036)) ;
#4216 = EDGE_LOOP('',(#20037,#20038,#20039,#20040)) ;
#4217 = EDGE_LOOP('',(#20041,#20042,#20043,#20044)) ;
#4218 = EDGE_LOOP('',(#20045,#20046,#20047,#20048)) ;
#4219 = EDGE_LOOP('',(#20049,#20050,#20051,#20052)) ;
#4220 = EDGE_LOOP('',(#20053,#20054,#20055,#20056)) ;
#4221 = EDGE_LOOP('',(#20057,#20058,#20059,#20060)) ;
#4222 = EDGE_LOOP('',(#20061,#20062,#20063,#20064)) ;
#4223 = EDGE_LOOP('',(#20065,#20066,#20067,#20068)) ;
#4224 = EDGE_LOOP('',(#20069,#20070,#20071,#20072)) ;
#4225 = EDGE_LOOP('',(#20073,#20074,#20075,#20076)) ;
#4226 = EDGE_LOOP('',(#20077,#20078,#20079,#20080)) ;
#4227 = EDGE_LOOP('',(#20081,#20082,#20083,#20084)) ;
#4228 = EDGE_LOOP('',(#20085,#20086,#20087,#20088)) ;
#4229 = EDGE_LOOP('',(#20089,#20090,#20091,#20092)) ;
#4230 = EDGE_LOOP('',(#20093,#20094,#20095,#20096)) ;
#4231 = EDGE_LOOP('',(#20097,#20098,#20099,#20100)) ;
#4232 = EDGE_LOOP('',(#20101,#20102,#20103,#20104)) ;
#4233 = EDGE_LOOP('',(#20105,#20106,#20107,#20108)) ;
#4234 = EDGE_LOOP('',(#20109,#20110,#20111,#20112)) ;
#4235 = EDGE_LOOP('',(#20113,#20114,#20115,#20116)) ;
#4236 = EDGE_LOOP('',(#20117,#20118,#20119,#20120)) ;
#4237 = EDGE_LOOP('',(#20121,#20122,#20123,#20124)) ;
#4238 = EDGE_LOOP('',(#20125,#20126,#20127,#20128)) ;
#4239 = EDGE_LOOP('',(#20129,#20130,#20131,#20132)) ;
#4240 = EDGE_LOOP('',(#20133,#20134,#20135,#20136)) ;
#4241 = EDGE_LOOP('',(#20137,#20138,#20139,#20140)) ;
#4242 = EDGE_LOOP('',(#20141,#20142,#20143,#20144)) ;
#4243 = EDGE_LOOP('',(#20145,#20146,#20147,#20148)) ;
#4244 = EDGE_LOOP('',(#20149,#20150,#20151,#20152)) ;
#4245 = EDGE_LOOP('',(#20153,#20154,#20155,#20156)) ;
#4246 = EDGE_LOOP('',(#20157,#20158,#20159,#20160)) ;
#4247 = EDGE_LOOP('',(#20161,#20162,#20163,#20164)) ;
#4248 = EDGE_LOOP('',(#20165,#20166,#20167,#20168)) ;
#4249 = EDGE_LOOP('',(#20169,#20170,#20171,#20172)) ;
#4250 = EDGE_LOOP('',(#20173,#20174,#20175,#20176)) ;
#4251 = EDGE_LOOP('',(#20177,#20178,#20179,#20180)) ;
#4252 = EDGE_LOOP('',(#20181,#20182,#20183,#20184)) ;
#4253 = EDGE_LOOP('',(#20185,#20186,#20187,#20188)) ;
#4254 = EDGE_LOOP('',(#20189,#20190,#20191,#20192)) ;
#4255 = EDGE_LOOP('',(#20193,#20194,#20195,#20196)) ;
#4256 = EDGE_LOOP('',(#20197,#20198,#20199,#20200)) ;
#4257 = EDGE_LOOP('',(#20201,#20202,#20203,#20204)) ;
#4258 = EDGE_LOOP('',(#20205,#20206,#20207,#20208)) ;
#4259 = EDGE_LOOP('',(#20209,#20210,#20211,#20212)) ;
#4260 = EDGE_LOOP('',(#20213,#20214,#20215,#20216)) ;
#4261 = EDGE_LOOP('',(#20217,#20218,#20219,#20220)) ;
#4262 = EDGE_LOOP('',(#20221,#20222,#20223,#20224)) ;
#4263 = EDGE_LOOP('',(#20225,#20226,#20227,#20228)) ;
#4264 = EDGE_LOOP('',(#20229,#20230,#20231,#20232)) ;
#4265 = EDGE_LOOP('',(#20233,#20234,#20235,#20236)) ;
#4266 = EDGE_LOOP('',(#20237,#20238,#20239,#20240)) ;
#4267 = EDGE_LOOP('',(#20241,#20242,#20243,#20244)) ;
#4268 = EDGE_LOOP('',(#20245,#20246,#20247,#20248)) ;
#4269 = EDGE_LOOP('',(#20249,#20250,#20251,#20252)) ;
#4270 = EDGE_LOOP('',(#20253,#20254,#20255,#20256)) ;
#4271 = EDGE_LOOP('',(#20257,#20258,#20259,#20260)) ;
#4272 = EDGE_LOOP('',(#20261,#20262,#20263,#20264)) ;
#4273 = EDGE_LOOP('',(#20265,#20266,#20267,#20268)) ;
#4274 = EDGE_LOOP('',(#20269,#20270,#20271,#20272)) ;
#4275 = EDGE_LOOP('',(#20273,#20274,#20275,#20276)) ;
#4276 = EDGE_LOOP('',(#20277,#20278,#20279,#20280)) ;
#4277 = EDGE_LOOP('',(#20281,#20282,#20283,#20284)) ;
#4278 = EDGE_LOOP('',(#20285,#20286,#20287,#20288)) ;
#4279 = EDGE_LOOP('',(#20289,#20290,#20291,#20292)) ;
#4280 = EDGE_LOOP('',(#20293,#20294,#20295,#20296)) ;
#4281 = EDGE_LOOP('',(#20297,#20298,#20299,#20300)) ;
#4282 = EDGE_LOOP('',(#20301,#20302,#20303,#20304)) ;
#4283 = EDGE_LOOP('',(#20305,#20306,#20307,#20308)) ;
#4284 = EDGE_LOOP('',(#20309,#20310,#20311,#20312)) ;
#4285 = EDGE_LOOP('',(#20313,#20314,#20315,#20316)) ;
#4286 = EDGE_LOOP('',(#20317,#20318,#20319,#20320)) ;
#4287 = EDGE_LOOP('',(#20321,#20322,#20323,#20324)) ;
#4288 = EDGE_LOOP('',(#20325,#20326,#20327,#20328)) ;
#4289 = EDGE_LOOP('',(#20329,#20330,#20331,#20332)) ;
#4290 = EDGE_LOOP('',(#20333,#20334,#20335,#20336)) ;
#4291 = EDGE_LOOP('',(#20337,#20338,#20339,#20340)) ;
#4292 = EDGE_LOOP('',(#20341,#20342,#20343,#20344)) ;
#4293 = EDGE_LOOP('',(#20345,#20346,#20347,#20348)) ;
#4294 = EDGE_LOOP('',(#20349,#20350,#20351,#20352)) ;
#4295 = EDGE_LOOP('',(#20353,#20354,#20355,#20356)) ;
#4296 = EDGE_LOOP('',(#20357,#20358,#20359,#20360)) ;
#4297 = EDGE_LOOP('',(#20361,#20362,#20363,#20364)) ;
#4298 = EDGE_LOOP('',(#20365,#20366,#20367,#20368)) ;
#4299 = EDGE_LOOP('',(#20369,#20370,#20371,#20372)) ;
#4300 = EDGE_LOOP('',(#20373,#20374,#20375,#20376)) ;
#4301 = EDGE_LOOP('',(#20377,#20378,#20379,#20380)) ;
#4302 = EDGE_LOOP('',(#20381,#20382,#20383,#20384)) ;
#4303 = EDGE_LOOP('',(#20385,#20386,#20387,#20388)) ;
#4304 = EDGE_LOOP('',(#20389,#20390,#20391,#20392)) ;
#4305 = EDGE_LOOP('',(#20393,#20394,#20395,#20396)) ;
#4306 = EDGE_LOOP('',(#20397,#20398,#20399,#20400)) ;
#4307 = EDGE_LOOP('',(#20401,#20402,#20403,#20404)) ;
#4308 = EDGE_LOOP('',(#20405,#20406,#20407,#20408)) ;
#4309 = EDGE_LOOP('',(#20409,#20410,#20411,#20412)) ;
#4310 = EDGE_LOOP('',(#20413,#20414,#20415,#20416)) ;
#4311 = EDGE_LOOP('',(#20417,#20418,#20419,#20420)) ;
#4312 = EDGE_LOOP('',(#20421,#20422,#20423,#20424)) ;
#4313 = EDGE_LOOP('',(#20425,#20426,#20427,#20428)) ;
#4314 = EDGE_LOOP('',(#20429,#20430,#20431,#20432)) ;
#4315 = EDGE_LOOP('',(#20433,#20434,#20435,#20436)) ;
#4316 = EDGE_LOOP('',(#20437,#20438,#20439,#20440)) ;
#4317 = EDGE_LOOP('',(#20441,#20442,#20443,#20444)) ;
#4318 = EDGE_LOOP('',(#20445,#20446,#20447,#20448)) ;
#4319 = EDGE_LOOP('',(#20449,#20450,#20451,#20452)) ;
#4320 = EDGE_LOOP('',(#20453,#20454,#20455,#20456)) ;
#4321 = EDGE_LOOP('',(#20457,#20458,#20459,#20460)) ;
#4322 = EDGE_LOOP('',(#20461,#20462,#20463,#20464)) ;
#4323 = EDGE_LOOP('',(#20465,#20466,#20467,#20468)) ;
#4324 = EDGE_LOOP('',(#20469,#20470,#20471,#20472)) ;
#4325 = EDGE_LOOP('',(#20473,#20474,#20475,#20476)) ;
#4326 = EDGE_LOOP('',(#20477,#20478,#20479,#20480)) ;
#4327 = EDGE_LOOP('',(#20481,#20482,#20483,#20484)) ;
#4328 = EDGE_LOOP('',(#20485,#20486,#20487,#20488)) ;
#4329 = EDGE_LOOP('',(#20489,#20490,#20491,#20492)) ;
#4330 = EDGE_LOOP('',(#20493,#20494,#20495,#20496)) ;
#4331 = EDGE_LOOP('',(#20497,#20498,#20499,#20500)) ;
#4332 = EDGE_LOOP('',(#20501,#20502,#20503,#20504)) ;
#4333 = EDGE_LOOP('',(#20505,#20506,#20507,#20508)) ;
#4334 = EDGE_LOOP('',(#20509,#20510,#20511,#20512)) ;
#4335 = EDGE_LOOP('',(#20513,#20514,#20515,#20516)) ;
#4336 = EDGE_LOOP('',(#20517,#20518,#20519,#20520)) ;
#4337 = EDGE_LOOP('',(#20521,#20522,#20523,#20524)) ;
#4338 = EDGE_LOOP('',(#20525,#20526,#20527,#20528)) ;
#4339 = EDGE_LOOP('',(#20529,#20530,#20531,#20532)) ;
#4340 = EDGE_LOOP('',(#20533,#20534,#20535,#20536)) ;
#4341 = EDGE_LOOP('',(#20537,#20538,#20539,#20540)) ;
#4342 = EDGE_LOOP('',(#20541,#20542,#20543,#20544)) ;
#4343 = EDGE_LOOP('',(#20545,#20546,#20547,#20548)) ;
#4344 = EDGE_LOOP('',(#20549,#20550,#20551,#20552)) ;
#4345 = EDGE_LOOP('',(#20553,#20554,#20555,#20556)) ;
#4346 = EDGE_LOOP('',(#20557,#20558,#20559,#20560)) ;
#4347 = EDGE_LOOP('',(#20561,#20562,#20563,#20564)) ;
#4348 = EDGE_LOOP('',(#20565,#20566,#20567,#20568)) ;
#4349 = EDGE_LOOP('',(#20569,#20570,#20571,#20572)) ;
#4350 = EDGE_LOOP('',(#20573,#20574,#20575,#20576)) ;
#4351 = EDGE_LOOP('',(#20577,#20578,#20579,#20580)) ;
#4352 = EDGE_LOOP('',(#20581,#20582,#20583,#20584)) ;
#4353 = EDGE_LOOP('',(#20585,#20586,#20587,#20588)) ;
#4354 = EDGE_LOOP('',(#20589,#20590,#20591,#20592)) ;
#4355 = EDGE_LOOP('',(#20593,#20594,#20595,#20596)) ;
#4356 = EDGE_LOOP('',(#20597,#20598,#20599,#20600)) ;
#4357 = EDGE_LOOP('',(#20601,#20602,#20603,#20604)) ;
#4358 = EDGE_LOOP('',(#20605,#20606,#20607,#20608)) ;
#4359 = EDGE_LOOP('',(#20609,#20610,#20611,#20612)) ;
#4360 = EDGE_LOOP('',(#20613,#20614,#20615,#20616)) ;
#4361 = EDGE_LOOP('',(#20617,#20618,#20619,#20620)) ;
#4362 = EDGE_LOOP('',(#20621,#20622,#20623,#20624)) ;
#4363 = EDGE_LOOP('',(#20625,#20626,#20627,#20628)) ;
#4364 = EDGE_LOOP('',(#20629,#20630,#20631,#20632)) ;
#4365 = EDGE_LOOP('',(#20633,#20634,#20635,#20636)) ;
#4366 = EDGE_LOOP('',(#20637,#20638,#20639,#20640)) ;
#4367 = EDGE_LOOP('',(#20641,#20642,#20643,#20644)) ;
#4368 = EDGE_LOOP('',(#20645,#20646,#20647,#20648)) ;
#4369 = EDGE_LOOP('',(#20649,#20650,#20651,#20652)) ;
#4370 = EDGE_LOOP('',(#20653,#20654,#20655,#20656)) ;
#4371 = EDGE_LOOP('',(#20657,#20658,#20659,#20660)) ;
#4372 = EDGE_LOOP('',(#20661,#20662,#20663,#20664)) ;
#4373 = EDGE_LOOP('',(#20665,#20666,#20667,#20668)) ;
#4374 = EDGE_LOOP('',(#20669,#20670,#20671,#20672)) ;
#4375 = EDGE_LOOP('',(#20673,#20674,#20675,#20676)) ;
#4376 = EDGE_LOOP('',(#20677,#20678,#20679,#20680)) ;
#4377 = EDGE_LOOP('',(#20681,#20682,#20683,#20684)) ;
#4378 = EDGE_LOOP('',(#20685,#20686,#20687,#20688)) ;
#4379 = EDGE_LOOP('',(#20689,#20690,#20691,#20692)) ;
#4380 = EDGE_LOOP('',(#20693,#20694,#20695,#20696)) ;
#4381 = EDGE_LOOP('',(#20697,#20698,#20699,#20700)) ;
#4382 = EDGE_LOOP('',(#20701,#20702,#20703,#20704)) ;
#4383 = EDGE_LOOP('',(#20705,#20706,#20707,#20708)) ;
#4384 = EDGE_LOOP('',(#20709,#20710,#20711,#20712)) ;
#4385 = EDGE_LOOP('',(#20713,#20714,#20715,#20716)) ;
#4386 = EDGE_LOOP('',(#20717,#20718,#20719,#20720)) ;
#4387 = EDGE_LOOP('',(#20721,#20722,#20723,#20724)) ;
#4388 = EDGE_LOOP('',(#20725,#20726,#20727,#20728)) ;
#4389 = EDGE_LOOP('',(#20729,#20730,#20731,#20732)) ;
#4390 = EDGE_LOOP('',(#20733,#20734,#20735,#20736)) ;
#4391 = EDGE_LOOP('',(#20737,#20738,#20739,#20740)) ;
#4392 = EDGE_LOOP('',(#20741,#20742,#20743,#20744)) ;
#4393 = EDGE_LOOP('',(#20745,#20746,#20747,#20748)) ;
#4394 = EDGE_LOOP('',(#20749,#20750,#20751,#20752)) ;
#4395 = EDGE_LOOP('',(#20753,#20754)) ;
#4396 = EDGE_LOOP('',(#20755,#20756)) ;
#4397 = EDGE_LOOP('',(#20757,#20758)) ;
#4398 = EDGE_LOOP('',(#20759,#20760)) ;
#4399 = EDGE_LOOP('',(#20761,#20762)) ;
#4400 = EDGE_LOOP('',(#20763,#20764)) ;
#4401 = EDGE_LOOP('',(#20765,#20766)) ;
#4402 = EDGE_LOOP('',(#20767,#20768,#20769)) ;
#4403 = EDGE_LOOP('',(#20770,#20771,#20772,#20773)) ;
#4404 = EDGE_LOOP('',(#20774,#20775,#20776,#20777)) ;
#4405 = EDGE_LOOP('',(#20778,#20779,#20780,#20781)) ;
#4406 = EDGE_LOOP('',(#20782,#20783,#20784,#20785)) ;
#4407 = EDGE_LOOP('',(#20786,#20787,#20788,#20789)) ;
#4408 = EDGE_LOOP('',(#20790,#20791,#20792,#20793)) ;
#4409 = EDGE_LOOP('',(#20794,#20795,#20796,#20797)) ;
#4410 = EDGE_LOOP('',(#20798,#20799,#20800,#20801)) ;
#4411 = EDGE_LOOP('',(#20802,#20803,#20804,#20805)) ;
#4412 = EDGE_LOOP('',(#20806,#20807,#20808,#20809)) ;
#4413 = EDGE_LOOP('',(#20810,#20811,#20812,#20813)) ;
#4414 = EDGE_LOOP('',(#20814,#20815,#20816,#20817)) ;
#4415 = EDGE_LOOP('',(#20818,#20819,#20820,#20821)) ;
#4416 = EDGE_LOOP('',(#20822,#20823,#20824)) ;
#4417 = EDGE_LOOP('',(#20825,#20826)) ;
#4418 = EDGE_LOOP('',(#20827,#20828)) ;
#4419 = EDGE_LOOP('',(#20829,#20830)) ;
#4420 = EDGE_LOOP('',(#20831,#20832)) ;
#4421 = EDGE_LOOP('',(#20833,#20834)) ;
#4422 = EDGE_LOOP('',(#20835,#20836)) ;
#4423 = EDGE_LOOP('',(#20837,#20838,#20839,#20840,#20841,#20842,#20843,#20844)) ;
#4424 = EDGE_LOOP('',(#20845,#20846,#20847,#20848,#20849,#20850,#20851,#20852)) ;
#4425 = EDGE_LOOP('',(#20853,#20854,#20855,#20856,#20857,#20858,#20859,#20860)) ;
#4426 = EDGE_LOOP('',(#20861,#20862,#20863,#20864,#20865,#20866,#20867,#20868)) ;
#4427 = EDGE_LOOP('',(#20869,#20870,#20871,#20872,#20873,#20874,#20875,#20876)) ;
#4428 = EDGE_LOOP('',(#20877,#20878,#20879,#20880,#20881,#20882,#20883,#20884)) ;
#4429 = EDGE_LOOP('',(#20885,#20886,#20887,#20888,#20889,#20890,#20891,#20892)) ;
#4430 = EDGE_LOOP('',(#20893,#20894,#20895,#20896,#20897,#20898,#20899,#20900,
#20901)) ;
#4431 = EDGE_LOOP('',(#20902,#20903,#20904,#20905,#20906,#20907,#20908,#20909)) ;
#4432 = EDGE_LOOP('',(#20910,#20911,#20912,#20913,#20914,#20915,#20916,#20917)) ;
#4433 = EDGE_LOOP('',(#20918,#20919,#20920,#20921,#20922,#20923,#20924,#20925)) ;
#4434 = EDGE_LOOP('',(#20926,#20927,#20928,#20929,#20930,#20931,#20932,#20933)) ;
#4435 = EDGE_LOOP('',(#20934,#20935,#20936,#20937,#20938,#20939,#20940,#20941)) ;
#4436 = EDGE_LOOP('',(#20942,#20943,#20944,#20945,#20946,#20947,#20948,#20949)) ;
#4437 = EDGE_LOOP('',(#20950,#20951,#20952,#20953,#20954,#20955,#20956,#20957)) ;
#4438 = EDGE_LOOP('',(#20958,#20959,#20960,#20961,#20962,#20963,#20964,#20965)) ;
#4439 = EDGE_LOOP('',(#20966,#20967,#20968,#20969,#20970,#20971,#20972,#20973)) ;
#4440 = EDGE_LOOP('',(#20974,#20975,#20976,#20977,#20978,#20979,#20980,#20981)) ;
#4441 = EDGE_LOOP('',(#20982,#20983,#20984,#20985,#20986,#20987,#20988,#20989)) ;
#4442 = EDGE_LOOP('',(#20990,#20991,#20992,#20993,#20994,#20995,#20996,#20997)) ;
#4443 = EDGE_LOOP('',(#20998,#20999,#21000,#21001,#21002,#21003,#21004,#21005,
#21006)) ;
#4444 = EDGE_LOOP('',(#21007,#21008,#21009,#21010,#21011,#21012,#21013,#21014)) ;
#4445 = EDGE_LOOP('',(#21015,#21016,#21017,#21018,#21019,#21020,#21021,#21022)) ;
#4446 = EDGE_LOOP('',(#21023,#21024,#21025,#21026,#21027,#21028,#21029,#21030)) ;
#4447 = EDGE_LOOP('',(#21031,#21032,#21033,#21034,#21035,#21036,#21037,#21038)) ;
#4448 = EDGE_LOOP('',(#21039,#21040,#21041,#21042,#21043,#21044,#21045,#21046)) ;
#4449 = EDGE_LOOP('',(#21047,#21048,#21049,#21050,#21051,#21052,#21053,#21054)) ;
#4450 = EDGE_LOOP('',(#21055,#21056,#21057,#21058,#21059,#21060,#21061,#21062)) ;
#4451 = EDGE_LOOP('',(#21063,#21064,#21065,#21066)) ;
#4452 = EDGE_LOOP('',(#21067,#21068,#21069,#21070)) ;
#4453 = EDGE_LOOP('',(#21071,#21072,#21073,#21074)) ;
#4454 = EDGE_LOOP('',(#21075,#21076,#21077,#21078)) ;
#4455 = EDGE_LOOP('',(#21079,#21080,#21081,#21082)) ;
#4456 = EDGE_LOOP('',(#21083,#21084,#21085,#21086)) ;
#4457 = EDGE_LOOP('',(#21087,#21088,#21089,#21090)) ;
#4458 = EDGE_LOOP('',(#21091,#21092,#21093,#21094)) ;
#4459 = EDGE_LOOP('',(#21095,#21096,#21097,#21098,#21099,#21100)) ;
#4460 = EDGE_LOOP('',(#21101,#21102,#21103,#21104)) ;
#4461 = EDGE_LOOP('',(#21105,#21106,#21107,#21108)) ;
#4462 = EDGE_LOOP('',(#21109)) ;
#4463 = EDGE_LOOP('',(#21110)) ;
#4464 = EDGE_LOOP('',(#21111,#21112,#21113,#21114)) ;
#4465 = EDGE_LOOP('',(#21115)) ;
#4466 = EDGE_LOOP('',(#21116)) ;
#4467 = EDGE_LOOP('',(#21117,#21118,#21119,#21120)) ;
#4468 = EDGE_LOOP('',(#21121,#21122,#21123,#21124,#21125,#21126)) ;
#4469 = EDGE_LOOP('',(#21127,#21128,#21129,#21130)) ;
#4470 = EDGE_LOOP('',(#21131,#21132,#21133,#21134)) ;
#4471 = EDGE_LOOP('',(#21135,#21136,#21137,#21138)) ;
#4472 = EDGE_LOOP('',(#21139,#21140,#21141,#21142)) ;
#4473 = EDGE_LOOP('',(#21143,#21144,#21145,#21146,#21147,#21148)) ;
#4474 = EDGE_LOOP('',(#21149,#21150,#21151,#21152)) ;
#4475 = EDGE_LOOP('',(#21153,#21154,#21155,#21156)) ;
#4476 = EDGE_LOOP('',(#21157)) ;
#4477 = EDGE_LOOP('',(#21158)) ;
#4478 = EDGE_LOOP('',(#21159,#21160,#21161,#21162)) ;
#4479 = EDGE_LOOP('',(#21163)) ;
#4480 = EDGE_LOOP('',(#21164)) ;
#4481 = EDGE_LOOP('',(#21165,#21166,#21167,#21168)) ;
#4482 = EDGE_LOOP('',(#21169,#21170,#21171,#21172,#21173,#21174)) ;
#4483 = EDGE_LOOP('',(#21175,#21176,#21177,#21178)) ;
#4484 = EDGE_LOOP('',(#21179,#21180,#21181,#21182)) ;
#4485 = EDGE_LOOP('',(#21183,#21184,#21185,#21186)) ;
#4486 = EDGE_LOOP('',(#21187,#21188,#21189,#21190)) ;
#4487 = EDGE_LOOP('',(#21191)) ;
#4488 = EDGE_LOOP('',(#21192)) ;
#4489 = EDGE_LOOP('',(#21193,#21194,#21195,#21196,#21197)) ;
#4490 = EDGE_LOOP('',(#21198)) ;
#4491 = EDGE_LOOP('',(#21199)) ;
#4492 = EDGE_LOOP('',(#21200)) ;
#4493 = EDGE_LOOP('',(#21201)) ;
#4494 = EDGE_LOOP('',(#21202,#21203,#21204,#21205)) ;
#4495 = EDGE_LOOP('',(#21206,#21207,#21208,#21209)) ;
#4496 = EDGE_LOOP('',(#21210)) ;
#4497 = EDGE_LOOP('',(#21211)) ;
#4498 = EDGE_LOOP('',(#21212)) ;
#4499 = EDGE_LOOP('',(#21213,#21214,#21215,#21216)) ;
#4500 = EDGE_LOOP('',(#21217,#21218,#21219,#21220)) ;
#4501 = EDGE_LOOP('',(#21221,#21222,#21223,#21224)) ;
#4502 = EDGE_LOOP('',(#21225,#21226,#21227,#21228)) ;
#4503 = EDGE_LOOP('',(#21229,#21230,#21231,#21232)) ;
#4504 = EDGE_LOOP('',(#21233,#21234,#21235,#21236)) ;
#4505 = EDGE_LOOP('',(#21237,#21238,#21239,#21240)) ;
#4506 = EDGE_LOOP('',(#21241,#21242,#21243,#21244)) ;
#4507 = EDGE_LOOP('',(#21245,#21246,#21247,#21248,#21249)) ;
#4508 = EDGE_LOOP('',(#21250)) ;
#4509 = EDGE_LOOP('',(#21251)) ;
#4510 = EDGE_LOOP('',(#21252,#21253,#21254,#21255)) ;
#4511 = EDGE_LOOP('',(#21256,#21257,#21258,#21259)) ;
#4512 = EDGE_LOOP('',(#21260)) ;
#4513 = EDGE_LOOP('',(#21261,#21262,#21263,#21264)) ;
#4514 = EDGE_LOOP('',(#21265,#21266,#21267,#21268,#21269,#21270,#21271,#21272,
#21273,#21274)) ;
#4515 = EDGE_LOOP('',(#21275,#21276,#21277,#21278,#21279,#21280,#21281,#21282)) ;
#4516 = EDGE_LOOP('',(#21283,#21284,#21285,#21286)) ;
#4517 = EDGE_LOOP('',(#21287,#21288,#21289,#21290)) ;
#4518 = EDGE_LOOP('',(#21291,#21292,#21293,#21294)) ;
#4519 = EDGE_LOOP('',(#21295,#21296,#21297,#21298)) ;
#4520 = EDGE_LOOP('',(#21299,#21300,#21301,#21302)) ;
#4521 = EDGE_LOOP('',(#21303,#21304,#21305,#21306)) ;
#4522 = EDGE_LOOP('',(#21307,#21308,#21309,#21310)) ;
#4523 = EDGE_LOOP('',(#21311,#21312,#21313,#21314)) ;
#4524 = EDGE_LOOP('',(#21315,#21316,#21317,#21318)) ;
#4525 = EDGE_LOOP('',(#21319,#21320,#21321,#21322)) ;
#4526 = EDGE_LOOP('',(#21323,#21324,#21325,#21326,#21327,#21328,#21329,#21330,
#21331,#21332,#21333,#21334,#21335,#21336,#21337,#21338,#21339,#21340)) ;
#4527 = EDGE_LOOP('',(#21341,#21342,#21343,#21344,#21345,#21346,#21347,#21348,
#21349,#21350,#21351,#21352)) ;
#4528 = EDGE_LOOP('',(#21353,#21354,#21355,#21356)) ;
#4529 = EDGE_LOOP('',(#21357,#21358,#21359,#21360)) ;
#4530 = EDGE_LOOP('',(#21361,#21362,#21363,#21364)) ;
#4531 = EDGE_LOOP('',(#21365,#21366,#21367,#21368)) ;
#4532 = EDGE_LOOP('',(#21369,#21370,#21371,#21372)) ;
#4533 = EDGE_LOOP('',(#21373,#21374,#21375,#21376)) ;
#4534 = EDGE_LOOP('',(#21377,#21378,#21379,#21380)) ;
#4535 = EDGE_LOOP('',(#21381,#21382,#21383,#21384)) ;
#4536 = EDGE_LOOP('',(#21385,#21386,#21387,#21388)) ;
#4537 = EDGE_LOOP('',(#21389,#21390,#21391,#21392)) ;
#4538 = EDGE_LOOP('',(#21393)) ;
#4539 = EDGE_LOOP('',(#21394)) ;
#4540 = EDGE_LOOP('',(#21395,#21396,#21397,#21398)) ;
#4541 = EDGE_LOOP('',(#21399,#21400,#21401,#21402)) ;
#4542 = EDGE_LOOP('',(#21403,#21404,#21405,#21406)) ;
#4543 = EDGE_LOOP('',(#21407,#21408,#21409,#21410)) ;
#4544 = EDGE_LOOP('',(#21411,#21412,#21413,#21414)) ;
#4545 = EDGE_LOOP('',(#21415,#21416,#21417,#21418)) ;
#4546 = EDGE_LOOP('',(#21419,#21420,#21421,#21422)) ;
#4547 = EDGE_LOOP('',(#21423,#21424,#21425,#21426)) ;
#4548 = EDGE_LOOP('',(#21427,#21428,#21429,#21430)) ;
#4549 = EDGE_LOOP('',(#21431)) ;
#4550 = EDGE_LOOP('',(#21432)) ;
#4551 = EDGE_LOOP('',(#21433)) ;
#4552 = EDGE_LOOP('',(#21434)) ;
#4553 = EDGE_LOOP('',(#21435,#21436,#21437,#21438,#21439)) ;
#4554 = EDGE_LOOP('',(#21440,#21441,#21442,#21443,#21444)) ;
#4555 = EDGE_LOOP('',(#21445,#21446,#21447,#21448)) ;
#4556 = EDGE_LOOP('',(#21449,#21450,#21451,#21452)) ;
#4557 = EDGE_LOOP('',(#21453,#21454,#21455,#21456)) ;
#4558 = EDGE_LOOP('',(#21457,#21458,#21459,#21460)) ;
#4559 = EDGE_LOOP('',(#21461,#21462,#21463,#21464)) ;
#4560 = EDGE_LOOP('',(#21465,#21466,#21467,#21468)) ;
#4561 = EDGE_LOOP('',(#21469,#21470,#21471,#21472)) ;
#4562 = EDGE_LOOP('',(#21473,#21474,#21475,#21476)) ;
#4563 = EDGE_LOOP('',(#21477,#21478,#21479,#21480,#21481,#21482,#21483,#21484)) ;
#4564 = EDGE_LOOP('',(#21485)) ;
#4565 = EDGE_LOOP('',(#21486,#21487,#21488,#21489,#21490,#21491,#21492,#21493)) ;
#4566 = EDGE_LOOP('',(#21494)) ;
#4567 = EDGE_LOOP('',(#21495,#21496,#21497,#21498)) ;
#4568 = EDGE_LOOP('',(#21499,#21500,#21501,#21502,#21503)) ;
#4569 = EDGE_LOOP('',(#21504)) ;
#4570 = EDGE_LOOP('',(#21505)) ;
#4571 = EDGE_LOOP('',(#21506,#21507,#21508,#21509)) ;
#4572 = EDGE_LOOP('',(#21510,#21511,#21512,#21513)) ;
#4573 = EDGE_LOOP('',(#21514,#21515,#21516,#21517)) ;
#4574 = EDGE_LOOP('',(#21518,#21519,#21520,#21521)) ;
#4575 = EDGE_LOOP('',(#21522,#21523,#21524,#21525)) ;
#4576 = EDGE_LOOP('',(#21526,#21527,#21528,#21529)) ;
#4577 = EDGE_LOOP('',(#21530,#21531,#21532,#21533)) ;
#4578 = EDGE_LOOP('',(#21534,#21535,#21536,#21537)) ;
#4579 = EDGE_LOOP('',(#21538)) ;
#4580 = EDGE_LOOP('',(#21539)) ;
#4581 = EDGE_LOOP('',(#21540)) ;
#4582 = EDGE_LOOP('',(#21541,#21542,#21543,#21544)) ;
#4583 = EDGE_LOOP('',(#21545,#21546,#21547,#21548)) ;
#4584 = EDGE_LOOP('',(#21549,#21550,#21551,#21552,#21553)) ;
#4585 = EDGE_LOOP('',(#21554)) ;
#4586 = EDGE_LOOP('',(#21555)) ;
#4587 = EDGE_LOOP('',(#21556)) ;
#4588 = EDGE_LOOP('',(#21557)) ;
#4589 = EDGE_LOOP('',(#21558)) ;
#4590 = EDGE_LOOP('',(#21559)) ;
#4591 = EDGE_LOOP('',(#21560,#21561,#21562,#21563)) ;
#4592 = EDGE_LOOP('',(#21564,#21565,#21566,#21567)) ;
#4593 = EDGE_LOOP('',(#21568,#21569,#21570,#21571,#21572,#21573,#21574,#21575,
#21576,#21577,#21578,#21579)) ;
#4594 = EDGE_LOOP('',(#21580,#21581,#21582,#21583)) ;
#4595 = EDGE_LOOP('',(#21584,#21585,#21586,#21587)) ;
#4596 = EDGE_LOOP('',(#21588,#21589,#21590,#21591)) ;
#4597 = EDGE_LOOP('',(#21592,#21593,#21594,#21595)) ;
#4598 = EDGE_LOOP('',(#21596,#21597,#21598,#21599,#21600,#21601,#21602,#21603,
#21604,#21605)) ;
#4599 = EDGE_LOOP('',(#21606)) ;
#4600 = EDGE_LOOP('',(#21607,#21608,#21609,#21610)) ;
#4601 = EDGE_LOOP('',(#21611,#21612,#21613,#21614)) ;
#4602 = EDGE_LOOP('',(#21615,#21616,#21617,#21618,#21619,#21620,#21621,#21622)) ;
#4603 = EDGE_LOOP('',(#21623,#21624,#21625,#21626)) ;
#4604 = EDGE_LOOP('',(#21627,#21628,#21629,#21630,#21631,#21632,#21633,#21634,
#21635,#21636,#21637,#21638,#21639,#21640,#21641,#21642,#21643,#21644)) ;
#4605 = EDGE_LOOP('',(#21645,#21646,#21647,#21648,#21649,#21650,#21651,#21652)) ;
#4606 = EDGE_LOOP('',(#21653,#21654,#21655,#21656)) ;
#4607 = EDGE_LOOP('',(#21657,#21658,#21659,#21660)) ;
#4608 = EDGE_LOOP('',(#21661,#21662,#21663,#21664,#21665,#21666,#21667,#21668)) ;
#4609 = EDGE_LOOP('',(#21669)) ;
#4610 = EDGE_LOOP('',(#21670,#21671,#21672,#21673)) ;
#4611 = EDGE_LOOP('',(#21674,#21675,#21676,#21677)) ;
#4612 = EDGE_LOOP('',(#21678,#21679,#21680,#21681,#21682,#21683,#21684,#21685)) ;
#4613 = EDGE_LOOP('',(#21686)) ;
#4614 = EDGE_LOOP('',(#21687,#21688,#21689,#21690)) ;
#4615 = EDGE_LOOP('',(#21691,#21692,#21693,#21694)) ;
#4616 = EDGE_LOOP('',(#21695,#21696,#21697,#21698)) ;
#4617 = EDGE_LOOP('',(#21699,#21700,#21701,#21702)) ;
#4618 = EDGE_LOOP('',(#21703,#21704,#21705,#21706)) ;
#4619 = EDGE_LOOP('',(#21707,#21708,#21709,#21710)) ;
#4620 = EDGE_LOOP('',(#21711,#21712,#21713,#21714)) ;
#4621 = EDGE_LOOP('',(#21715,#21716,#21717,#21718)) ;
#4622 = EDGE_LOOP('',(#21719,#21720,#21721,#21722)) ;
#4623 = EDGE_LOOP('',(#21723,#21724,#21725,#21726)) ;
#4624 = EDGE_LOOP('',(#21727,#21728,#21729,#21730)) ;
#4625 = EDGE_LOOP('',(#21731,#21732,#21733,#21734)) ;
#4626 = EDGE_LOOP('',(#21735,#21736,#21737,#21738)) ;
#4627 = EDGE_LOOP('',(#21739,#21740)) ;
#4628 = EDGE_LOOP('',(#21741,#21742)) ;
#4629 = EDGE_LOOP('',(#21743,#21744,#21745,#21746)) ;
#4630 = EDGE_LOOP('',(#21747,#21748,#21749,#21750)) ;
#4631 = EDGE_LOOP('',(#21751,#21752,#21753,#21754)) ;
#4632 = EDGE_LOOP('',(#21755,#21756,#21757,#21758)) ;
#4633 = EDGE_LOOP('',(#21759,#21760,#21761)) ;
#4634 = EDGE_LOOP('',(#21762,#21763,#21764)) ;
#4635 = EDGE_LOOP('',(#21765,#21766,#21767,#21768)) ;
#4636 = EDGE_LOOP('',(#21769,#21770,#21771)) ;
#4637 = EDGE_LOOP('',(#21772,#21773,#21774,#21775)) ;
#4638 = EDGE_LOOP('',(#21776,#21777,#21778)) ;
#4639 = EDGE_LOOP('',(#21779,#21780,#21781,#21782)) ;
#4640 = EDGE_LOOP('',(#21783,#21784,#21785,#21786)) ;
#4641 = EDGE_LOOP('',(#21787,#21788,#21789,#21790)) ;
#4642 = EDGE_LOOP('',(#21791,#21792,#21793,#21794)) ;
#4643 = EDGE_LOOP('',(#21795,#21796,#21797)) ;
#4644 = EDGE_LOOP('',(#21798,#21799,#21800)) ;
#4645 = EDGE_LOOP('',(#21801,#21802,#21803,#21804)) ;
#4646 = EDGE_LOOP('',(#21805,#21806,#21807)) ;
#4647 = EDGE_LOOP('',(#21808,#21809,#21810)) ;
#4648 = EDGE_LOOP('',(#21811,#21812,#21813,#21814)) ;
#4649 = EDGE_LOOP('',(#21815,#21816,#21817,#21818)) ;
#4650 = EDGE_LOOP('',(#21819,#21820,#21821,#21822)) ;
#4651 = EDGE_LOOP('',(#21823,#21824,#21825,#21826)) ;
#4652 = EDGE_LOOP('',(#21827,#21828,#21829,#21830)) ;
#4653 = EDGE_LOOP('',(#21831,#21832,#21833)) ;
#4654 = EDGE_LOOP('',(#21834,#21835,#21836,#21837)) ;
#4655 = EDGE_LOOP('',(#21838,#21839,#21840)) ;
#4656 = EDGE_LOOP('',(#21841,#21842,#21843)) ;
#4657 = EDGE_LOOP('',(#21844,#21845,#21846)) ;
#4658 = EDGE_LOOP('',(#21847,#21848,#21849,#21850)) ;
#4659 = EDGE_LOOP('',(#21851,#21852,#21853,#21854)) ;
#4660 = EDGE_LOOP('',(#21855,#21856,#21857,#21858)) ;
#4661 = EDGE_LOOP('',(#21859,#21860,#21861,#21862)) ;
#4662 = EDGE_LOOP('',(#21863,#21864)) ;
#4663 = EDGE_LOOP('',(#21865,#21866)) ;
#4664 = EDGE_LOOP('',(#21867,#21868,#21869,#21870)) ;
#4665 = EDGE_LOOP('',(#21871,#21872,#21873,#21874)) ;
#4666 = EDGE_LOOP('',(#21875,#21876)) ;
#4667 = EDGE_LOOP('',(#21877,#21878)) ;
#4668 = EDGE_LOOP('',(#21879,#21880,#21881,#21882)) ;
#4669 = EDGE_LOOP('',(#21883,#21884,#21885,#21886)) ;
#4670 = EDGE_LOOP('',(#21887,#21888)) ;
#4671 = EDGE_LOOP('',(#21889,#21890)) ;
#4672 = EDGE_LOOP('',(#21891,#21892,#21893,#21894)) ;
#4673 = EDGE_LOOP('',(#21895,#21896,#21897,#21898)) ;
#4674 = EDGE_LOOP('',(#21899,#21900)) ;
#4675 = EDGE_LOOP('',(#21901,#21902)) ;
#4676 = EDGE_LOOP('',(#21903,#21904,#21905,#21906)) ;
#4677 = EDGE_LOOP('',(#21907,#21908,#21909,#21910)) ;
#4678 = EDGE_LOOP('',(#21911,#21912)) ;
#4679 = EDGE_LOOP('',(#21913,#21914,#21915,#21916)) ;
#4680 = EDGE_LOOP('',(#21917,#21918)) ;
#4681 = EDGE_LOOP('',(#21919,#21920,#21921,#21922)) ;
#4682 = EDGE_LOOP('',(#21923,#21924,#21925,#21926)) ;
#4683 = EDGE_LOOP('',(#21927,#21928,#21929,#21930)) ;
#4684 = EDGE_LOOP('',(#21931,#21932,#21933,#21934)) ;
#4685 = EDGE_LOOP('',(#21935,#21936,#21937,#21938)) ;
#4686 = EDGE_LOOP('',(#21939,#21940,#21941,#21942)) ;
#4687 = EDGE_LOOP('',(#21943,#21944,#21945,#21946)) ;
#4688 = EDGE_LOOP('',(#21947,#21948,#21949,#21950)) ;
#4689 = EDGE_LOOP('',(#21951,#21952,#21953,#21954)) ;
#4690 = EDGE_LOOP('',(#21955,#21956,#21957,#21958)) ;
#4691 = EDGE_LOOP('',(#21959,#21960,#21961,#21962)) ;
#4692 = EDGE_LOOP('',(#21963,#21964,#21965,#21966)) ;
#4693 = EDGE_LOOP('',(#21967,#21968,#21969,#21970)) ;
#4694 = EDGE_LOOP('',(#21971,#21972,#21973,#21974)) ;
#4695 = EDGE_LOOP('',(#21975,#21976,#21977,#21978)) ;
#4696 = EDGE_LOOP('',(#21979,#21980,#21981,#21982,#21983,#21984,#21985,#21986,
#21987,#21988,#21989,#21990)) ;
#4697 = EDGE_LOOP('',(#21991,#21992,#21993,#21994)) ;
#4698 = EDGE_LOOP('',(#21995,#21996,#21997,#21998)) ;
#4699 = EDGE_LOOP('',(#21999,#22000,#22001,#22002,#22003,#22004,#22005,#22006,
#22007,#22008,#22009,#22010)) ;
#4700 = EDGE_LOOP('',(#22011,#22012,#22013,#22014)) ;
#4701 = EDGE_LOOP('',(#22015,#22016,#22017,#22018)) ;
#4702 = EDGE_LOOP('',(#22019,#22020,#22021,#22022)) ;
#4703 = EDGE_LOOP('',(#22023,#22024,#22025,#22026)) ;
#4704 = EDGE_LOOP('',(#22027,#22028,#22029,#22030)) ;
#4705 = EDGE_LOOP('',(#22031,#22032,#22033,#22034)) ;
#4706 = EDGE_LOOP('',(#22035,#22036,#22037,#22038)) ;
#4707 = EDGE_LOOP('',(#22039,#22040,#22041,#22042)) ;
#4708 = EDGE_LOOP('',(#22043,#22044,#22045,#22046)) ;
#4709 = EDGE_LOOP('',(#22047,#22048)) ;
#4710 = EDGE_LOOP('',(#22049,#22050)) ;
#4711 = EDGE_LOOP('',(#22051,#22052)) ;
#4712 = EDGE_LOOP('',(#22053,#22054,#22055,#22056)) ;
#4713 = EDGE_LOOP('',(#22057,#22058,#22059,#22060,#22061,#22062,#22063,#22064,
#22065,#22066,#22067,#22068)) ;
#4714 = EDGE_LOOP('',(#22069,#22070)) ;
#4715 = EDGE_LOOP('',(#22071,#22072,#22073,#22074)) ;
#4716 = EDGE_LOOP('',(#22075,#22076,#22077,#22078)) ;
#4717 = EDGE_LOOP('',(#22079,#22080,#22081,#22082)) ;
#4718 = EDGE_LOOP('',(#22083,#22084,#22085,#22086)) ;
#4719 = EDGE_LOOP('',(#22087,#22088,#22089,#22090)) ;
#4720 = EDGE_LOOP('',(#22091,#22092,#22093,#22094)) ;
#4721 = EDGE_LOOP('',(#22095,#22096,#22097,#22098)) ;
#4722 = EDGE_LOOP('',(#22099,#22100,#22101,#22102)) ;
#4723 = EDGE_LOOP('',(#22103,#22104,#22105,#22106)) ;
#4724 = EDGE_LOOP('',(#22107,#22108,#22109,#22110)) ;
#4725 = EDGE_LOOP('',(#22111,#22112,#22113,#22114,#22115,#22116)) ;
#4726 = EDGE_LOOP('',(#22117)) ;
#4727 = EDGE_LOOP('',(#22118)) ;
#4728 = EDGE_LOOP('',(#22119,#22120,#22121,#22122)) ;
#4729 = EDGE_LOOP('',(#22123)) ;
#4730 = EDGE_LOOP('',(#22124,#22125,#22126,#22127)) ;
#4731 = EDGE_LOOP('',(#22128,#22129)) ;
#4732 = EDGE_LOOP('',(#22130,#22131)) ;
#4733 = EDGE_LOOP('',(#22132)) ;
#4734 = EDGE_LOOP('',(#22133,#22134,#22135,#22136,#22137,#22138)) ;
#4735 = EDGE_LOOP('',(#22139)) ;
#4736 = EDGE_LOOP('',(#22140)) ;
#4737 = EDGE_LOOP('',(#22141,#22142,#22143,#22144)) ;
#4738 = EDGE_LOOP('',(#22145)) ;
#4739 = EDGE_LOOP('',(#22146,#22147,#22148,#22149)) ;
#4740 = EDGE_LOOP('',(#22150,#22151)) ;
#4741 = EDGE_LOOP('',(#22152,#22153)) ;
#4742 = EDGE_LOOP('',(#22154)) ;
#4743 = EDGE_LOOP('',(#22155,#22156,#22157,#22158)) ;
#4744 = EDGE_LOOP('',(#22159,#22160,#22161,#22162)) ;
#4745 = EDGE_LOOP('',(#22163,#22164,#22165,#22166)) ;
#4746 = EDGE_LOOP('',(#22167,#22168,#22169,#22170)) ;
#4747 = EDGE_LOOP('',(#22171,#22172,#22173,#22174)) ;
#4748 = EDGE_LOOP('',(#22175,#22176)) ;
#4749 = EDGE_LOOP('',(#22177,#22178,#22179,#22180,#22181,#22182,#22183,#22184,
#22185,#22186,#22187,#22188,#22189,#22190,#22191,#22192,#22193,#22194)) ;
#4750 = EDGE_LOOP('',(#22195,#22196)) ;
#4751 = EDGE_LOOP('',(#22197,#22198,#22199,#22200)) ;
#4752 = EDGE_LOOP('',(#22201,#22202,#22203,#22204,#22205,#22206,#22207,#22208,
#22209,#22210,#22211,#22212,#22213,#22214,#22215,#22216,#22217,#22218,#22219,
#22220)) ;
#4753 = EDGE_LOOP('',(#22221)) ;
#4754 = EDGE_LOOP('',(#22222,#22223)) ;
#4755 = EDGE_LOOP('',(#22224,#22225,#22226,#22227)) ;
#4756 = EDGE_LOOP('',(#22228,#22229,#22230,#22231,#22232,#22233,#22234,#22235,
#22236,#22237,#22238,#22239,#22240,#22241,#22242,#22243,#22244,#22245,#22246,
#22247)) ;
#4757 = EDGE_LOOP('',(#22248)) ;
#4758 = EDGE_LOOP('',(#22249,#22250)) ;
#4759 = EDGE_LOOP('',(#22251,#22252,#22253,#22254)) ;
#4760 = EDGE_LOOP('',(#22255,#22256,#22257,#22258)) ;
#4761 = EDGE_LOOP('',(#22259)) ;
#4762 = EDGE_LOOP('',(#22260,#22261,#22262,#22263)) ;
#4763 = EDGE_LOOP('',(#22264)) ;
#4764 = EDGE_LOOP('',(#22265)) ;
#4765 = EDGE_LOOP('',(#22266,#22267,#22268,#22269)) ;
#4766 = EDGE_LOOP('',(#22270,#22271,#22272,#22273)) ;
#4767 = EDGE_LOOP('',(#22274,#22275,#22276,#22277,#22278,#22279)) ;
#4768 = EDGE_LOOP('',(#22280,#22281,#22282,#22283)) ;
#4769 = EDGE_LOOP('',(#22284,#22285,#22286,#22287)) ;
#4770 = EDGE_LOOP('',(#22288,#22289,#22290,#22291,#22292,#22293)) ;
#4771 = EDGE_LOOP('',(#22294,#22295,#22296,#22297)) ;
#4772 = EDGE_LOOP('',(#22298,#22299,#22300,#22301)) ;
#4773 = EDGE_LOOP('',(#22302,#22303,#22304,#22305)) ;
#4774 = EDGE_LOOP('',(#22306,#22307,#22308,#22309)) ;
#4775 = EDGE_LOOP('',(#22310,#22311,#22312,#22313,#22314,#22315)) ;
#4776 = EDGE_LOOP('',(#22316,#22317,#22318,#22319)) ;
#4777 = EDGE_LOOP('',(#22320,#22321,#22322,#22323)) ;
#4778 = EDGE_LOOP('',(#22324,#22325,#22326,#22327,#22328,#22329)) ;
#4779 = EDGE_LOOP('',(#22330,#22331)) ;
#4780 = EDGE_LOOP('',(#22332,#22333,#22334,#22335,#22336,#22337,#22338,#22339)) ;
#4781 = EDGE_LOOP('',(#22340,#22341,#22342,#22343,#22344,#22345,#22346,#22347,
#22348)) ;
#4782 = EDGE_LOOP('',(#22349,#22350,#22351,#22352)) ;
#4783 = EDGE_LOOP('',(#22353)) ;
#4784 = EDGE_LOOP('',(#22354)) ;
#4785 = EDGE_LOOP('',(#22355)) ;
#4786 = EDGE_LOOP('',(#22356,#22357,#22358,#22359)) ;
#4787 = EDGE_LOOP('',(#22360)) ;
#4788 = EDGE_LOOP('',(#22361,#22362,#22363,#22364)) ;
#4789 = EDGE_LOOP('',(#22365)) ;
#4790 = EDGE_LOOP('',(#22366)) ;
#4791 = EDGE_LOOP('',(#22367,#22368,#22369,#22370)) ;
#4792 = EDGE_LOOP('',(#22371)) ;
#4793 = EDGE_LOOP('',(#22372,#22373,#22374,#22375)) ;
#4794 = EDGE_LOOP('',(#22376)) ;
#4795 = EDGE_LOOP('',(#22377)) ;
#4796 = EDGE_LOOP('',(#22378,#22379,#22380,#22381)) ;
#4797 = EDGE_LOOP('',(#22382)) ;
#4798 = EDGE_LOOP('',(#22383,#22384,#22385,#22386)) ;
#4799 = EDGE_LOOP('',(#22387)) ;
#4800 = EDGE_LOOP('',(#22388,#22389,#22390,#22391)) ;
#4801 = EDGE_LOOP('',(#22392,#22393,#22394,#22395)) ;
#4802 = EDGE_LOOP('',(#22396,#22397,#22398,#22399,#22400,#22401,#22402,#22403,
#22404,#22405,#22406,#22407,#22408)) ;
#4803 = EDGE_LOOP('',(#22409)) ;
#4804 = EDGE_LOOP('',(#22410,#22411,#22412,#22413)) ;
#4805 = EDGE_LOOP('',(#22414)) ;
#4806 = EDGE_LOOP('',(#22415,#22416,#22417,#22418)) ;
#4807 = EDGE_LOOP('',(#22419)) ;
#4808 = EDGE_LOOP('',(#22420,#22421,#22422,#22423)) ;
#4809 = EDGE_LOOP('',(#22424,#22425,#22426,#22427)) ;
#4810 = EDGE_LOOP('',(#22428,#22429,#22430,#22431)) ;
#4811 = EDGE_LOOP('',(#22432)) ;
#4812 = EDGE_LOOP('',(#22433,#22434,#22435,#22436)) ;
#4813 = EDGE_LOOP('',(#22437)) ;
#4814 = EDGE_LOOP('',(#22438,#22439,#22440,#22441)) ;
#4815 = EDGE_LOOP('',(#22442,#22443,#22444,#22445)) ;
#4816 = EDGE_LOOP('',(#22446,#22447,#22448,#22449)) ;
#4817 = EDGE_LOOP('',(#22450)) ;
#4818 = EDGE_LOOP('',(#22451,#22452,#22453,#22454)) ;
#4819 = EDGE_LOOP('',(#22455)) ;
#4820 = EDGE_LOOP('',(#22456,#22457,#22458,#22459)) ;
#4821 = EDGE_LOOP('',(#22460,#22461,#22462,#22463)) ;
#4822 = EDGE_LOOP('',(#22464,#22465,#22466,#22467,#22468,#22469,#22470,#22471,
#22472,#22473,#22474,#22475)) ;
#4823 = EDGE_LOOP('',(#22476,#22477,#22478,#22479)) ;
#4824 = EDGE_LOOP('',(#22480,#22481,#22482,#22483)) ;
#4825 = EDGE_LOOP('',(#22484,#22485,#22486,#22487)) ;
#4826 = EDGE_LOOP('',(#22488)) ;
#4827 = EDGE_LOOP('',(#22489,#22490,#22491,#22492)) ;
#4828 = EDGE_LOOP('',(#22493)) ;
#4829 = EDGE_LOOP('',(#22494,#22495,#22496,#22497)) ;
#4830 = EDGE_LOOP('',(#22498,#22499,#22500,#22501)) ;
#4831 = EDGE_LOOP('',(#22502,#22503,#22504,#22505,#22506,#22507)) ;
#4832 = EDGE_LOOP('',(#22508)) ;
#4833 = EDGE_LOOP('',(#22509,#22510,#22511,#22512)) ;
#4834 = EDGE_LOOP('',(#22513,#22514,#22515,#22516)) ;
#4835 = EDGE_LOOP('',(#22517,#22518,#22519,#22520)) ;
#4836 = EDGE_LOOP('',(#22521,#22522,#22523,#22524)) ;
#4837 = EDGE_LOOP('',(#22525,#22526,#22527,#22528,#22529,#22530)) ;
#4838 = EDGE_LOOP('',(#22531,#22532,#22533,#22534,#22535)) ;
#4839 = EDGE_LOOP('',(#22536,#22537,#22538,#22539,#22540)) ;
#4840 = EDGE_LOOP('',(#22541,#22542,#22543,#22544)) ;
#4841 = EDGE_LOOP('',(#22545,#22546,#22547,#22548,#22549)) ;
#4842 = EDGE_LOOP('',(#22550,#22551,#22552,#22553,#22554)) ;
#4843 = EDGE_LOOP('',(#22555,#22556,#22557,#22558)) ;
#4844 = EDGE_LOOP('',(#22559,#22560,#22561,#22562)) ;
#4845 = EDGE_LOOP('',(#22563,#22564,#22565,#22566)) ;
#4846 = EDGE_LOOP('',(#22567,#22568,#22569,#22570)) ;
#4847 = EDGE_LOOP('',(#22571,#22572,#22573,#22574)) ;
#4848 = EDGE_LOOP('',(#22575,#22576,#22577,#22578)) ;
#4849 = EDGE_LOOP('',(#22579,#22580,#22581,#22582)) ;
#4850 = EDGE_LOOP('',(#22583,#22584,#22585,#22586,#22587)) ;
#4851 = EDGE_LOOP('',(#22588,#22589,#22590,#22591,#22592)) ;
#4852 = EDGE_LOOP('',(#22593,#22594,#22595,#22596,#22597)) ;
#4853 = EDGE_LOOP('',(#22598,#22599,#22600,#22601,#22602)) ;
#4854 = EDGE_LOOP('',(#22603,#22604,#22605,#22606,#22607)) ;
#4855 = EDGE_LOOP('',(#22608,#22609,#22610,#22611)) ;
#4856 = EDGE_LOOP('',(#22612,#22613,#22614,#22615,#22616,#22617,#22618,#22619)) ;
#4857 = EDGE_LOOP('',(#22620,#22621,#22622,#22623,#22624,#22625,#22626,#22627)) ;
#4858 = EDGE_LOOP('',(#22628,#22629,#22630,#22631)) ;
#4859 = EDGE_LOOP('',(#22632,#22633,#22634,#22635,#22636,#22637,#22638,#22639)) ;
#4860 = EDGE_LOOP('',(#22640,#22641,#22642,#22643)) ;
#4861 = EDGE_LOOP('',(#22644,#22645,#22646,#22647)) ;
#4862 = EDGE_LOOP('',(#22648,#22649,#22650,#22651,#22652,#22653,#22654,#22655)) ;
#4863 = EDGE_LOOP('',(#22656,#22657,#22658,#22659)) ;
#4864 = EDGE_LOOP('',(#22660,#22661,#22662,#22663,#22664,#22665,#22666,#22667)) ;
#4865 = EDGE_LOOP('',(#22668,#22669,#22670,#22671)) ;
#4866 = EDGE_LOOP('',(#22672,#22673,#22674,#22675)) ;
#4867 = EDGE_LOOP('',(#22676,#22677,#22678,#22679,#22680,#22681,#22682,#22683)) ;
#4868 = EDGE_LOOP('',(#22684,#22685,#22686,#22687)) ;
#4869 = EDGE_LOOP('',(#22688,#22689,#22690,#22691)) ;
#4870 = EDGE_LOOP('',(#22692,#22693,#22694,#22695)) ;
#4871 = EDGE_LOOP('',(#22696,#22697,#22698,#22699)) ;
#4872 = EDGE_LOOP('',(#22700,#22701,#22702,#22703)) ;
#4873 = EDGE_LOOP('',(#22704,#22705,#22706,#22707)) ;
#4874 = EDGE_LOOP('',(#22708,#22709,#22710,#22711)) ;
#4875 = EDGE_LOOP('',(#22712,#22713,#22714,#22715,#22716,#22717,#22718,#22719,
#22720,#22721,#22722,#22723,#22724,#22725,#22726,#22727,#22728,#22729,#22730,
#22731,#22732,#22733,#22734,#22735)) ;
#4876 = EDGE_LOOP('',(#22736,#22737,#22738,#22739,#22740,#22741,#22742,#22743)) ;
#4877 = EDGE_LOOP('',(#22744,#22745,#22746,#22747)) ;
#4878 = EDGE_LOOP('',(#22748,#22749,#22750,#22751,#22752,#22753,#22754,#22755)) ;
#4879 = EDGE_LOOP('',(#22756,#22757,#22758,#22759)) ;
#4880 = EDGE_LOOP('',(#22760,#22761,#22762,#22763)) ;
#4881 = EDGE_LOOP('',(#22764,#22765,#22766,#22767)) ;
#4882 = EDGE_LOOP('',(#22768,#22769,#22770,#22771,#22772,#22773,#22774,#22775,
#22776,#22777,#22778,#22779,#22780,#22781,#22782,#22783,#22784,#22785,#22786,
#22787,#22788,#22789,#22790,#22791,#22792,#22793,#22794,#22795)) ;
#4883 = EDGE_LOOP('',(#22796,#22797,#22798,#22799)) ;
#4884 = EDGE_LOOP('',(#22800,#22801,#22802,#22803,#22804,#22805,#22806,#22807)) ;
#4885 = EDGE_LOOP('',(#22808,#22809,#22810,#22811,#22812,#22813,#22814,#22815)) ;
#4886 = EDGE_LOOP('',(#22816,#22817,#22818,#22819)) ;
#4887 = EDGE_LOOP('',(#22820,#22821,#22822,#22823,#22824,#22825,#22826,#22827)) ;
#4888 = EDGE_LOOP('',(#22828,#22829,#22830,#22831)) ;
#4889 = EDGE_LOOP('',(#22832,#22833,#22834,#22835,#22836,#22837,#22838,#22839)) ;
#4890 = EDGE_LOOP('',(#22840,#22841,#22842,#22843)) ;
#4891 = EDGE_LOOP('',(#22844,#22845,#22846,#22847)) ;
#4892 = EDGE_LOOP('',(#22848,#22849,#22850,#22851)) ;
#4893 = EDGE_LOOP('',(#22852)) ;
#4894 = EDGE_LOOP('',(#22853)) ;
#4895 = EDGE_LOOP('',(#22854)) ;
#4896 = EDGE_LOOP('',(#22855,#22856,#22857,#22858)) ;
#4897 = EDGE_LOOP('',(#22859)) ;
#4898 = EDGE_LOOP('',(#22860)) ;
#4899 = EDGE_LOOP('',(#22861,#22862,#22863,#22864)) ;
#4900 = EDGE_LOOP('',(#22865,#22866,#22867,#22868)) ;
#4901 = EDGE_LOOP('',(#22869)) ;
#4902 = EDGE_LOOP('',(#22870)) ;
#4903 = EDGE_LOOP('',(#22871)) ;
#4904 = EDGE_LOOP('',(#22872)) ;
#4905 = EDGE_LOOP('',(#22873,#22874,#22875,#22876)) ;
#4906 = EDGE_LOOP('',(#22877,#22878,#22879,#22880,#22881,#22882)) ;
#4907 = EDGE_LOOP('',(#22883,#22884,#22885,#22886)) ;
#4908 = EDGE_LOOP('',(#22887,#22888,#22889,#22890,#22891,#22892)) ;
#4909 = EDGE_LOOP('',(#22893,#22894,#22895,#22896,#22897,#22898,#22899,#22900)) ;
#4910 = EDGE_LOOP('',(#22901,#22902,#22903,#22904)) ;
#4911 = EDGE_LOOP('',(#22905,#22906,#22907,#22908,#22909,#22910)) ;
#4912 = EDGE_LOOP('',(#22911,#22912,#22913,#22914,#22915,#22916,#22917,#22918)) ;
#4913 = EDGE_LOOP('',(#22919,#22920,#22921,#22922,#22923,#22924,#22925,#22926)) ;
#4914 = EDGE_LOOP('',(#22927,#22928,#22929,#22930)) ;
#4915 = EDGE_LOOP('',(#22931,#22932,#22933,#22934)) ;
#4916 = EDGE_LOOP('',(#22935,#22936,#22937,#22938)) ;
#4917 = EDGE_LOOP('',(#22939,#22940,#22941,#22942,#22943,#22944)) ;
#4918 = EDGE_LOOP('',(#22945,#22946,#22947,#22948)) ;
#4919 = EDGE_LOOP('',(#22949,#22950,#22951,#22952)) ;
#4920 = EDGE_LOOP('',(#22953)) ;
#4921 = EDGE_LOOP('',(#22954)) ;
#4922 = EDGE_LOOP('',(#22955,#22956,#22957,#22958)) ;
#4923 = EDGE_LOOP('',(#22959)) ;
#4924 = EDGE_LOOP('',(#22960,#22961,#22962,#22963)) ;
#4925 = EDGE_LOOP('',(#22964,#22965,#22966,#22967)) ;
#4926 = EDGE_LOOP('',(#22968)) ;
#4927 = EDGE_LOOP('',(#22969)) ;
#4928 = EDGE_LOOP('',(#22970)) ;
#4929 = EDGE_LOOP('',(#22971)) ;
#4930 = EDGE_LOOP('',(#22972)) ;
#4931 = EDGE_LOOP('',(#22973,#22974,#22975,#22976)) ;
#4932 = EDGE_LOOP('',(#22977,#22978,#22979,#22980)) ;
#4933 = EDGE_LOOP('',(#22981)) ;
#4934 = EDGE_LOOP('',(#22982)) ;
#4935 = EDGE_LOOP('',(#22983)) ;
#4936 = EDGE_LOOP('',(#22984)) ;
#4937 = EDGE_LOOP('',(#22985,#22986,#22987,#22988)) ;
#4938 = EDGE_LOOP('',(#22989,#22990,#22991,#22992)) ;
#4939 = EDGE_LOOP('',(#22993)) ;
#4940 = EDGE_LOOP('',(#22994)) ;
#4941 = EDGE_LOOP('',(#22995)) ;
#4942 = EDGE_LOOP('',(#22996)) ;
#4943 = EDGE_LOOP('',(#22997,#22998,#22999,#23000)) ;
#4944 = EDGE_LOOP('',(#23001)) ;
#4945 = EDGE_LOOP('',(#23002)) ;
#4946 = EDGE_LOOP('',(#23003)) ;
#4947 = EDGE_LOOP('',(#23004)) ;
#4948 = EDGE_LOOP('',(#23005)) ;
#4949 = EDGE_LOOP('',(#23006)) ;
#4950 = EDGE_LOOP('',(#23007,#23008,#23009,#23010)) ;
#4951 = EDGE_LOOP('',(#23011,#23012,#23013,#23014,#23015,#23016,#23017,#23018,
#23019,#23020,#23021,#23022,#23023,#23024,#23025,#23026,#23027,#23028,#23029,
#23030)) ;
#4952 = EDGE_LOOP('',(#23031,#23032,#23033,#23034)) ;
#4953 = EDGE_LOOP('',(#23035,#23036,#23037,#23038)) ;
#4954 = EDGE_LOOP('',(#23039,#23040,#23041,#23042)) ;
#4955 = EDGE_LOOP('',(#23043,#23044,#23045,#23046)) ;
#4956 = EDGE_LOOP('',(#23047,#23048,#23049,#23050)) ;
#4957 = EDGE_LOOP('',(#23051,#23052,#23053,#23054)) ;
#4958 = EDGE_LOOP('',(#23055,#23056,#23057,#23058)) ;
#4959 = EDGE_LOOP('',(#23059,#23060,#23061,#23062)) ;
#4960 = EDGE_LOOP('',(#23063,#23064,#23065,#23066)) ;
#4961 = EDGE_LOOP('',(#23067,#23068,#23069,#23070)) ;
#4962 = EDGE_LOOP('',(#23071,#23072,#23073,#23074)) ;
#4963 = EDGE_LOOP('',(#23075,#23076,#23077,#23078)) ;
#4964 = EDGE_LOOP('',(#23079,#23080,#23081,#23082)) ;
#4965 = EDGE_LOOP('',(#23083,#23084,#23085,#23086)) ;
#4966 = EDGE_LOOP('',(#23087,#23088,#23089,#23090)) ;
#4967 = EDGE_LOOP('',(#23091,#23092,#23093,#23094)) ;
#4968 = EDGE_LOOP('',(#23095,#23096,#23097,#23098)) ;
#4969 = EDGE_LOOP('',(#23099,#23100,#23101,#23102)) ;
#4970 = EDGE_LOOP('',(#23103,#23104,#23105,#23106)) ;
#4971 = EDGE_LOOP('',(#23107,#23108,#23109,#23110,#23111)) ;
#4972 = EDGE_LOOP('',(#23112,#23113,#23114,#23115)) ;
#4973 = EDGE_LOOP('',(#23116,#23117,#23118,#23119)) ;
#4974 = EDGE_LOOP('',(#23120,#23121,#23122,#23123)) ;
#4975 = EDGE_LOOP('',(#23124,#23125,#23126,#23127,#23128)) ;
#4976 = EDGE_LOOP('',(#23129,#23130,#23131,#23132)) ;
#4977 = EDGE_LOOP('',(#23133,#23134,#23135,#23136)) ;
#4978 = EDGE_LOOP('',(#23137,#23138,#23139,#23140)) ;
#4979 = EDGE_LOOP('',(#23141,#23142,#23143,#23144)) ;
#4980 = EDGE_LOOP('',(#23145,#23146,#23147,#23148)) ;
#4981 = EDGE_LOOP('',(#23149,#23150,#23151,#23152)) ;
#4982 = EDGE_LOOP('',(#23153,#23154,#23155,#23156)) ;
#4983 = EDGE_LOOP('',(#23157,#23158,#23159,#23160)) ;
#4984 = EDGE_LOOP('',(#23161,#23162,#23163,#23164)) ;
#4985 = EDGE_LOOP('',(#23165,#23166,#23167,#23168)) ;
#4986 = EDGE_LOOP('',(#23169,#23170,#23171,#23172)) ;
#4987 = EDGE_LOOP('',(#23173,#23174,#23175,#23176)) ;
#4988 = EDGE_LOOP('',(#23177,#23178,#23179,#23180)) ;
#4989 = EDGE_LOOP('',(#23181,#23182,#23183,#23184)) ;
#4990 = EDGE_LOOP('',(#23185,#23186,#23187,#23188)) ;
#4991 = EDGE_LOOP('',(#23189,#23190,#23191,#23192,#23193)) ;
#4992 = EDGE_LOOP('',(#23194,#23195,#23196,#23197)) ;
#4993 = EDGE_LOOP('',(#23198,#23199,#23200,#23201)) ;
#4994 = EDGE_LOOP('',(#23202,#23203,#23204,#23205)) ;
#4995 = EDGE_LOOP('',(#23206,#23207,#23208,#23209,#23210)) ;
#4996 = EDGE_LOOP('',(#23211,#23212,#23213,#23214)) ;
#4997 = EDGE_LOOP('',(#23215,#23216,#23217,#23218)) ;
#4998 = EDGE_LOOP('',(#23219,#23220,#23221,#23222)) ;
#4999 = EDGE_LOOP('',(#23223)) ;
#5000 = EDGE_LOOP('',(#23224)) ;
#5001 = EDGE_LOOP('',(#23225,#23226,#23227,#23228)) ;
#5002 = EDGE_LOOP('',(#23229,#23230,#23231,#23232)) ;
#5003 = EDGE_LOOP('',(#23233)) ;
#5004 = EDGE_LOOP('',(#23234)) ;
#5005 = EDGE_LOOP('',(#23235)) ;
#5006 = EDGE_LOOP('',(#23236)) ;
#5007 = EDGE_LOOP('',(#23237,#23238,#23239,#23240)) ;
#5008 = EDGE_LOOP('',(#23241,#23242,#23243,#23244)) ;
#5009 = EDGE_LOOP('',(#23245)) ;
#5010 = EDGE_LOOP('',(#23246,#23247,#23248,#23249)) ;
#5011 = EDGE_LOOP('',(#23250,#23251,#23252,#23253,#23254,#23255)) ;
#5012 = EDGE_LOOP('',(#23256,#23257,#23258,#23259)) ;
#5013 = EDGE_LOOP('',(#23260,#23261,#23262,#23263)) ;
#5014 = EDGE_LOOP('',(#23264)) ;
#5015 = EDGE_LOOP('',(#23265,#23266,#23267,#23268,#23269,#23270)) ;
#5016 = EDGE_LOOP('',(#23271,#23272,#23273,#23274)) ;
#5017 = EDGE_LOOP('',(#23275,#23276,#23277,#23278)) ;
#5018 = EDGE_LOOP('',(#23279,#23280,#23281,#23282)) ;
#5019 = EDGE_LOOP('',(#23283,#23284,#23285,#23286)) ;
#5020 = EDGE_LOOP('',(#23287,#23288,#23289,#23290)) ;
#5021 = EDGE_LOOP('',(#23291)) ;
#5022 = EDGE_LOOP('',(#23292,#23293,#23294,#23295)) ;
#5023 = EDGE_LOOP('',(#23296,#23297,#23298,#23299)) ;
#5024 = EDGE_LOOP('',(#23300)) ;
#5025 = EDGE_LOOP('',(#23301,#23302,#23303,#23304)) ;
#5026 = EDGE_LOOP('',(#23305,#23306,#23307,#23308)) ;
#5027 = EDGE_LOOP('',(#23309,#23310,#23311,#23312)) ;
#5028 = EDGE_LOOP('',(#23313,#23314,#23315,#23316)) ;
#5029 = EDGE_LOOP('',(#23317,#23318,#23319,#23320,#23321,#23322,#23323,#23324)) ;
#5030 = EDGE_LOOP('',(#23325,#23326,#23327,#23328,#23329,#23330,#23331,#23332,
#23333,#23334,#23335,#23336,#23337,#23338,#23339,#23340,#23341,#23342,#23343)) ;
#5031 = EDGE_LOOP('',(#23344,#23345,#23346,#23347)) ;
#5032 = EDGE_LOOP('',(#23348,#23349,#23350,#23351)) ;
#5033 = EDGE_LOOP('',(#23352,#23353,#23354,#23355)) ;
#5034 = EDGE_LOOP('',(#23356,#23357,#23358,#23359,#23360,#23361)) ;
#5035 = EDGE_LOOP('',(#23362)) ;
#5036 = EDGE_LOOP('',(#23363)) ;
#5037 = EDGE_LOOP('',(#23364,#23365,#23366,#23367)) ;
#5038 = EDGE_LOOP('',(#23368,#23369,#23370,#23371)) ;
#5039 = EDGE_LOOP('',(#23372,#23373,#23374,#23375)) ;
#5040 = EDGE_LOOP('',(#23376,#23377,#23378,#23379)) ;
#5041 = EDGE_LOOP('',(#23380,#23381,#23382,#23383,#23384,#23385)) ;
#5042 = EDGE_LOOP('',(#23386)) ;
#5043 = EDGE_LOOP('',(#23387)) ;
#5044 = EDGE_LOOP('',(#23388,#23389,#23390,#23391)) ;
#5045 = EDGE_LOOP('',(#23392,#23393,#23394,#23395)) ;
#5046 = EDGE_LOOP('',(#23396,#23397,#23398,#23399)) ;
#5047 = EDGE_LOOP('',(#23400,#23401,#23402,#23403,#23404,#23405,#23406,#23407)) ;
#5048 = EDGE_LOOP('',(#23408,#23409,#23410,#23411)) ;
#5049 = EDGE_LOOP('',(#23412)) ;
#5050 = EDGE_LOOP('',(#23413)) ;
#5051 = EDGE_LOOP('',(#23414)) ;
#5052 = EDGE_LOOP('',(#23415)) ;
#5053 = EDGE_LOOP('',(#23416)) ;
#5054 = EDGE_LOOP('',(#23417,#23418)) ;
#5055 = EDGE_LOOP('',(#23419,#23420,#23421,#23422)) ;
#5056 = EDGE_LOOP('',(#23423,#23424,#23425,#23426,#23427,#23428,#23429,#23430)) ;
#5057 = EDGE_LOOP('',(#23431,#23432,#23433,#23434)) ;
#5058 = EDGE_LOOP('',(#23435,#23436,#23437,#23438,#23439,#23440,#23441,#23442)) ;
#5059 = EDGE_LOOP('',(#23443,#23444,#23445,#23446)) ;
#5060 = EDGE_LOOP('',(#23447,#23448,#23449,#23450)) ;
#5061 = EDGE_LOOP('',(#23451,#23452,#23453,#23454)) ;
#5062 = EDGE_LOOP('',(#23455,#23456,#23457,#23458,#23459,#23460)) ;
#5063 = EDGE_LOOP('',(#23461,#23462,#23463,#23464,#23465)) ;
#5064 = EDGE_LOOP('',(#23466,#23467,#23468,#23469,#23470,#23471)) ;
#5065 = EDGE_LOOP('',(#23472,#23473,#23474,#23475)) ;
#5066 = EDGE_LOOP('',(#23476,#23477,#23478,#23479)) ;
#5067 = EDGE_LOOP('',(#23480,#23481,#23482,#23483)) ;
#5068 = EDGE_LOOP('',(#23484,#23485,#23486,#23487)) ;
#5069 = EDGE_LOOP('',(#23488,#23489,#23490,#23491)) ;
#5070 = EDGE_LOOP('',(#23492,#23493,#23494,#23495)) ;
#5071 = EDGE_LOOP('',(#23496,#23497,#23498,#23499)) ;
#5072 = EDGE_LOOP('',(#23500,#23501,#23502,#23503,#23504,#23505,#23506,#23507)) ;
#5073 = EDGE_LOOP('',(#23508,#23509,#23510,#23511)) ;
#5074 = EDGE_LOOP('',(#23512,#23513,#23514,#23515)) ;
#5075 = EDGE_LOOP('',(#23516,#23517,#23518,#23519)) ;
#5076 = EDGE_LOOP('',(#23520,#23521,#23522,#23523)) ;
#5077 = EDGE_LOOP('',(#23524,#23525,#23526,#23527)) ;
#5078 = EDGE_LOOP('',(#23528,#23529,#23530,#23531)) ;
#5079 = EDGE_LOOP('',(#23532,#23533,#23534,#23535)) ;
#5080 = EDGE_LOOP('',(#23536,#23537,#23538,#23539,#23540,#23541,#23542,#23543,
#23544,#23545,#23546,#23547,#23548,#23549)) ;
#5081 = EDGE_LOOP('',(#23550)) ;
#5082 = EDGE_LOOP('',(#23551)) ;
#5083 = EDGE_LOOP('',(#23552)) ;
#5084 = EDGE_LOOP('',(#23553,#23554,#23555,#23556,#23557,#23558,#23559,#23560,
#23561,#23562,#23563,#23564)) ;
#5085 = EDGE_LOOP('',(#23565)) ;
#5086 = EDGE_LOOP('',(#23566)) ;
#5087 = EDGE_LOOP('',(#23567)) ;
#5088 = EDGE_LOOP('',(#23568,#23569,#23570,#23571)) ;
#5089 = EDGE_LOOP('',(#23572,#23573,#23574,#23575,#23576)) ;
#5090 = EDGE_LOOP('',(#23577,#23578,#23579,#23580)) ;
#5091 = EDGE_LOOP('',(#23581,#23582,#23583,#23584)) ;
#5092 = EDGE_LOOP('',(#23585,#23586,#23587,#23588)) ;
#5093 = EDGE_LOOP('',(#23589,#23590,#23591,#23592)) ;
#5094 = EDGE_LOOP('',(#23593,#23594,#23595,#23596,#23597,#23598,#23599,#23600,
#23601,#23602,#23603,#23604,#23605,#23606,#23607,#23608,#23609,#23610,#23611,
#23612,#23613,#23614,#23615,#23616,#23617,#23618,#23619,#23620,#23621,#23622,
#23623,#23624,#23625,#23626,#23627,#23628,#23629,#23630,#23631,#23632)) ;
#5095 = EDGE_LOOP('',(#23633,#23634,#23635,#23636)) ;
#5096 = EDGE_LOOP('',(#23637,#23638,#23639,#23640)) ;
#5097 = EDGE_LOOP('',(#23641,#23642,#23643,#23644)) ;
#5098 = EDGE_LOOP('',(#23645,#23646,#23647,#23648)) ;
#5099 = EDGE_LOOP('',(#23649,#23650,#23651,#23652,#23653,#23654,#23655,#23656,
#23657,#23658,#23659,#23660,#23661,#23662,#23663,#23664,#23665,#23666,#23667,
#23668,#23669,#23670,#23671,#23672,#23673,#23674,#23675,#23676,#23677,#23678,
#23679,#23680,#23681,#23682,#23683,#23684,#23685,#23686,#23687,#23688)) ;
#5100 = EDGE_LOOP('',(#23689,#23690,#23691,#23692)) ;
#5101 = EDGE_LOOP('',(#23693,#23694,#23695,#23696)) ;
#5102 = EDGE_LOOP('',(#23697,#23698,#23699,#23700)) ;
#5103 = EDGE_LOOP('',(#23701,#23702,#23703,#23704)) ;
#5104 = EDGE_LOOP('',(#23705,#23706,#23707,#23708)) ;
#5105 = EDGE_LOOP('',(#23709,#23710,#23711,#23712)) ;
#5106 = EDGE_LOOP('',(#23713,#23714,#23715,#23716)) ;
#5107 = EDGE_LOOP('',(#23717,#23718,#23719,#23720)) ;
#5108 = EDGE_LOOP('',(#23721,#23722,#23723,#23724)) ;
#5109 = EDGE_LOOP('',(#23725,#23726,#23727,#23728)) ;
#5110 = EDGE_LOOP('',(#23729,#23730,#23731,#23732)) ;
#5111 = EDGE_LOOP('',(#23733,#23734,#23735,#23736)) ;
#5112 = EDGE_LOOP('',(#23737,#23738,#23739,#23740)) ;
#5113 = EDGE_LOOP('',(#23741,#23742,#23743,#23744)) ;
#5114 = EDGE_LOOP('',(#23745,#23746,#23747,#23748)) ;
#5115 = EDGE_LOOP('',(#23749,#23750,#23751,#23752)) ;
#5116 = EDGE_LOOP('',(#23753,#23754,#23755,#23756)) ;
#5117 = EDGE_LOOP('',(#23757,#23758,#23759,#23760)) ;
#5118 = EDGE_LOOP('',(#23761,#23762,#23763,#23764)) ;
#5119 = EDGE_LOOP('',(#23765,#23766,#23767,#23768)) ;
#5120 = EDGE_LOOP('',(#23769,#23770,#23771,#23772)) ;
#5121 = EDGE_LOOP('',(#23773,#23774,#23775,#23776)) ;
#5122 = EDGE_LOOP('',(#23777,#23778,#23779,#23780)) ;
#5123 = EDGE_LOOP('',(#23781,#23782,#23783,#23784)) ;
#5124 = EDGE_LOOP('',(#23785,#23786,#23787,#23788)) ;
#5125 = EDGE_LOOP('',(#23789,#23790,#23791,#23792)) ;
#5126 = EDGE_LOOP('',(#23793,#23794,#23795,#23796)) ;
#5127 = EDGE_LOOP('',(#23797,#23798,#23799,#23800)) ;
#5128 = EDGE_LOOP('',(#23801,#23802,#23803,#23804)) ;
#5129 = EDGE_LOOP('',(#23805,#23806,#23807,#23808)) ;
#5130 = EDGE_LOOP('',(#23809,#23810,#23811,#23812)) ;
#5131 = EDGE_LOOP('',(#23813,#23814,#23815,#23816)) ;
#5132 = EDGE_LOOP('',(#23817,#23818,#23819,#23820)) ;
#5133 = EDGE_LOOP('',(#23821,#23822,#23823,#23824)) ;
#5134 = EDGE_LOOP('',(#23825,#23826,#23827,#23828)) ;
#5135 = EDGE_LOOP('',(#23829,#23830,#23831,#23832)) ;
#5136 = EDGE_LOOP('',(#23833,#23834,#23835,#23836)) ;
#5137 = EDGE_LOOP('',(#23837,#23838)) ;
#5138 = EDGE_LOOP('',(#23839,#23840,#23841,#23842)) ;
#5139 = EDGE_LOOP('',(#23843)) ;
#5140 = EDGE_LOOP('',(#23844)) ;
#5141 = EDGE_LOOP('',(#23845)) ;
#5142 = EDGE_LOOP('',(#23846)) ;
#5143 = EDGE_LOOP('',(#23847,#23848)) ;
#5144 = EDGE_LOOP('',(#23849,#23850,#23851,#23852,#23853)) ;
#5145 = EDGE_LOOP('',(#23854,#23855,#23856,#23857,#23858,#23859)) ;
#5146 = EDGE_LOOP('',(#23860,#23861,#23862,#23863)) ;
#5147 = EDGE_LOOP('',(#23864)) ;
#5148 = EDGE_LOOP('',(#23865)) ;
#5149 = EDGE_LOOP('',(#23866)) ;
#5150 = EDGE_LOOP('',(#23867)) ;
#5151 = EDGE_LOOP('',(#23868,#23869,#23870)) ;
#5152 = EDGE_LOOP('',(#23871,#23872,#23873,#23874)) ;
#5153 = EDGE_LOOP('',(#23875,#23876,#23877,#23878)) ;
#5154 = EDGE_LOOP('',(#23879,#23880,#23881,#23882)) ;
#5155 = EDGE_LOOP('',(#23883,#23884,#23885,#23886)) ;
#5156 = EDGE_LOOP('',(#23887,#23888,#23889,#23890,#23891,#23892)) ;
#5157 = EDGE_LOOP('',(#23893)) ;
#5158 = EDGE_LOOP('',(#23894)) ;
#5159 = EDGE_LOOP('',(#23895,#23896,#23897,#23898)) ;
#5160 = EDGE_LOOP('',(#23899,#23900,#23901,#23902)) ;
#5161 = EDGE_LOOP('',(#23903,#23904,#23905,#23906)) ;
#5162 = EDGE_LOOP('',(#23907)) ;
#5163 = EDGE_LOOP('',(#23908)) ;
#5164 = EDGE_LOOP('',(#23909)) ;
#5165 = EDGE_LOOP('',(#23910)) ;
#5166 = EDGE_LOOP('',(#23911)) ;
#5167 = EDGE_LOOP('',(#23912)) ;
#5168 = EDGE_LOOP('',(#23913)) ;
#5169 = EDGE_LOOP('',(#23914)) ;
#5170 = EDGE_LOOP('',(#23915,#23916,#23917,#23918)) ;
#5171 = EDGE_LOOP('',(#23919,#23920,#23921,#23922)) ;
#5172 = EDGE_LOOP('',(#23923,#23924,#23925,#23926)) ;
#5173 = EDGE_LOOP('',(#23927,#23928,#23929,#23930)) ;
#5174 = EDGE_LOOP('',(#23931,#23932,#23933,#23934)) ;
#5175 = EDGE_LOOP('',(#23935,#23936,#23937,#23938)) ;
#5176 = EDGE_LOOP('',(#23939,#23940,#23941,#23942)) ;
#5177 = EDGE_LOOP('',(#23943,#23944,#23945,#23946)) ;
#5178 = EDGE_LOOP('',(#23947,#23948,#23949,#23950)) ;
#5179 = EDGE_LOOP('',(#23951,#23952,#23953,#23954)) ;
#5180 = EDGE_LOOP('',(#23955,#23956,#23957,#23958)) ;
#5181 = EDGE_LOOP('',(#23959,#23960)) ;
#5182 = EDGE_LOOP('',(#23961)) ;
#5183 = EDGE_LOOP('',(#23962)) ;
#5184 = EDGE_LOOP('',(#23963)) ;
#5185 = EDGE_LOOP('',(#23964)) ;
#5186 = EDGE_LOOP('',(#23965)) ;
#5187 = EDGE_LOOP('',(#23966)) ;
#5188 = EDGE_LOOP('',(#23967)) ;
#5189 = EDGE_LOOP('',(#23968)) ;
#5190 = EDGE_LOOP('',(#23969,#23970)) ;
#5191 = EDGE_LOOP('',(#23971)) ;
#5192 = EDGE_LOOP('',(#23972)) ;
#5193 = EDGE_LOOP('',(#23973)) ;
#5194 = EDGE_LOOP('',(#23974)) ;
#5195 = EDGE_LOOP('',(#23975)) ;
#5196 = EDGE_LOOP('',(#23976)) ;
#5197 = EDGE_LOOP('',(#23977)) ;
#5198 = EDGE_LOOP('',(#23978)) ;
#5199 = EDGE_LOOP('',(#23979,#23980,#23981,#23982)) ;
#5200 = EDGE_LOOP('',(#23983,#23984,#23985,#23986,#23987)) ;
#5201 = EDGE_LOOP('',(#23988)) ;
#5202 = EDGE_LOOP('',(#23989,#23990,#23991,#23992)) ;
#5203 = EDGE_LOOP('',(#23993,#23994,#23995,#23996)) ;
#5204 = EDGE_LOOP('',(#23997,#23998,#23999,#24000)) ;
#5205 = EDGE_LOOP('',(#24001)) ;
#5206 = EDGE_LOOP('',(#24002)) ;
#5207 = EDGE_LOOP('',(#24003)) ;
#5208 = EDGE_LOOP('',(#24004,#24005,#24006,#24007)) ;
#5209 = EDGE_LOOP('',(#24008,#24009,#24010,#24011)) ;
#5210 = EDGE_LOOP('',(#24012,#24013,#24014,#24015)) ;
#5211 = EDGE_LOOP('',(#24016,#24017,#24018,#24019)) ;
#5212 = EDGE_LOOP('',(#24020,#24021,#24022,#24023)) ;
#5213 = EDGE_LOOP('',(#24024,#24025,#24026,#24027)) ;
#5214 = EDGE_LOOP('',(#24028,#24029,#24030,#24031)) ;
#5215 = EDGE_LOOP('',(#24032)) ;
#5216 = EDGE_LOOP('',(#24033,#24034,#24035,#24036)) ;
#5217 = EDGE_LOOP('',(#24037,#24038,#24039,#24040)) ;
#5218 = EDGE_LOOP('',(#24041)) ;
#5219 = EDGE_LOOP('',(#24042,#24043,#24044,#24045)) ;
#5220 = EDGE_LOOP('',(#24046,#24047,#24048,#24049,#24050)) ;
#5221 = EDGE_LOOP('',(#24051,#24052,#24053,#24054,#24055)) ;
#5222 = EDGE_LOOP('',(#24056,#24057,#24058,#24059)) ;
#5223 = EDGE_LOOP('',(#24060,#24061,#24062,#24063)) ;
#5224 = EDGE_LOOP('',(#24064,#24065,#24066,#24067)) ;
#5225 = EDGE_LOOP('',(#24068,#24069,#24070,#24071)) ;
#5226 = EDGE_LOOP('',(#24072,#24073,#24074,#24075)) ;
#5227 = EDGE_LOOP('',(#24076,#24077,#24078,#24079)) ;
#5228 = EDGE_LOOP('',(#24080,#24081,#24082,#24083)) ;
#5229 = EDGE_LOOP('',(#24084)) ;
#5230 = EDGE_LOOP('',(#24085,#24086,#24087,#24088)) ;
#5231 = EDGE_LOOP('',(#24089)) ;
#5232 = EDGE_LOOP('',(#24090,#24091,#24092)) ;
#5233 = EDGE_LOOP('',(#24093)) ;
#5234 = EDGE_LOOP('',(#24094)) ;
#5235 = EDGE_LOOP('',(#24095,#24096,#24097,#24098)) ;
#5236 = EDGE_LOOP('',(#24099)) ;
#5237 = EDGE_LOOP('',(#24100,#24101,#24102,#24103)) ;
#5238 = EDGE_LOOP('',(#24104)) ;
#5239 = EDGE_LOOP('',(#24105,#24106)) ;
#5240 = EDGE_LOOP('',(#24107,#24108)) ;
#5241 = EDGE_LOOP('',(#24109,#24110)) ;
#5242 = EDGE_LOOP('',(#24111)) ;
#5243 = EDGE_LOOP('',(#24112,#24113,#24114,#24115)) ;
#5244 = EDGE_LOOP('',(#24116)) ;
#5245 = EDGE_LOOP('',(#24117,#24118)) ;
#5246 = EDGE_LOOP('',(#24119,#24120,#24121,#24122)) ;
#5247 = EDGE_LOOP('',(#24123,#24124)) ;
#5248 = EDGE_LOOP('',(#24125,#24126,#24127)) ;
#5249 = EDGE_LOOP('',(#24128,#24129,#24130,#24131,#24132,#24133)) ;
#5250 = EDGE_LOOP('',(#24134,#24135,#24136,#24137)) ;
#5251 = EDGE_LOOP('',(#24138,#24139,#24140,#24141,#24142,#24143)) ;
#5252 = EDGE_LOOP('',(#24144)) ;
#5253 = EDGE_LOOP('',(#24145)) ;
#5254 = EDGE_LOOP('',(#24146,#24147,#24148,#24149,#24150,#24151,#24152,#24153,
#24154)) ;
#5255 = EDGE_LOOP('',(#24155,#24156,#24157,#24158,#24159,#24160,#24161,#24162)) ;
#5256 = EDGE_LOOP('',(#24163,#24164,#24165,#24166,#24167,#24168,#24169)) ;
#5257 = EDGE_LOOP('',(#24170,#24171,#24172,#24173,#24174,#24175,#24176,#24177)) ;
#5258 = EDGE_LOOP('',(#24178,#24179,#24180)) ;
#5259 = EDGE_LOOP('',(#24181,#24182,#24183,#24184,#24185,#24186)) ;
#5260 = EDGE_LOOP('',(#24187)) ;
#5261 = EDGE_LOOP('',(#24188)) ;
#5262 = EDGE_LOOP('',(#24189,#24190)) ;
#5263 = EDGE_LOOP('',(#24191,#24192,#24193)) ;
#5264 = EDGE_LOOP('',(#24194)) ;
#5265 = EDGE_LOOP('',(#24195)) ;
#5266 = EDGE_LOOP('',(#24196,#24197,#24198)) ;
#5267 = EDGE_LOOP('',(#24199,#24200,#24201,#24202,#24203,#24204)) ;
#5268 = EDGE_LOOP('',(#24205,#24206)) ;
#5269 = EDGE_LOOP('',(#24207,#24208)) ;
#5270 = EDGE_LOOP('',(#24209,#24210,#24211)) ;
#5271 = EDGE_LOOP('',(#24212,#24213)) ;
#5272 = EDGE_LOOP('',(#24214,#24215)) ;
#5273 = EDGE_LOOP('',(#24216,#24217,#24218,#24219,#24220,#24221,#24222,#24223)) ;
#5274 = EDGE_LOOP('',(#24224,#24225,#24226)) ;
#5275 = EDGE_LOOP('',(#24227,#24228,#24229,#24230,#24231)) ;
#5276 = EDGE_LOOP('',(#24232,#24233)) ;
#5277 = EDGE_LOOP('',(#24234,#24235,#24236,#24237,#24238,#24239,#24240,#24241)) ;
#5278 = EDGE_LOOP('',(#24242,#24243)) ;
#5279 = EDGE_LOOP('',(#24244,#24245,#24246)) ;
#5280 = EDGE_LOOP('',(#24247,#24248)) ;
#5281 = EDGE_LOOP('',(#24249,#24250,#24251,#24252,#24253,#24254,#24255,#24256)) ;
#5282 = EDGE_LOOP('',(#24257)) ;
#5283 = EDGE_LOOP('',(#24258,#24259,#24260,#24261)) ;
#5284 = EDGE_LOOP('',(#24262,#24263,#24264)) ;
#5285 = EDGE_LOOP('',(#24265,#24266,#24267,#24268,#24269,#24270,#24271,#24272,
#24273,#24274,#24275)) ;
#5286 = EDGE_LOOP('',(#24276)) ;
#5287 = EDGE_LOOP('',(#24277,#24278,#24279,#24280)) ;
#5288 = EDGE_LOOP('',(#24281)) ;
#5289 = EDGE_LOOP('',(#24282)) ;
#5290 = EDGE_LOOP('',(#24283,#24284,#24285,#24286)) ;
#5291 = EDGE_LOOP('',(#24287)) ;
#5292 = EDGE_LOOP('',(#24288)) ;
#5293 = EDGE_LOOP('',(#24289,#24290,#24291,#24292)) ;
#5294 = EDGE_LOOP('',(#24293)) ;
#5295 = EDGE_LOOP('',(#24294)) ;
#5296 = EDGE_LOOP('',(#24295,#24296,#24297,#24298)) ;
#5297 = EDGE_LOOP('',(#24299,#24300)) ;
#5298 = EDGE_LOOP('',(#24301,#24302,#24303,#24304)) ;
#5299 = EDGE_LOOP('',(#24305)) ;
#5300 = EDGE_LOOP('',(#24306)) ;
#5301 = EDGE_LOOP('',(#24307)) ;
#5302 = EDGE_LOOP('',(#24308)) ;
#5303 = EDGE_LOOP('',(#24309,#24310,#24311,#24312,#24313)) ;
#5304 = EDGE_LOOP('',(#24314)) ;
#5305 = EDGE_LOOP('',(#24315,#24316,#24317,#24318)) ;
#5306 = EDGE_LOOP('',(#24319,#24320,#24321,#24322)) ;
#5307 = EDGE_LOOP('',(#24323)) ;
#5308 = EDGE_LOOP('',(#24324)) ;
#5309 = EDGE_LOOP('',(#24325)) ;
#5310 = EDGE_LOOP('',(#24326)) ;
#5311 = EDGE_LOOP('',(#24327,#24328,#24329,#24330,#24331,#24332,#24333,#24334)) ;
#5312 = EDGE_LOOP('',(#24335,#24336,#24337,#24338)) ;
#5313 = EDGE_LOOP('',(#24339)) ;
#5314 = EDGE_LOOP('',(#24340,#24341,#24342,#24343,#24344,#24345,#24346)) ;
#5315 = EDGE_LOOP('',(#24347)) ;
#5316 = EDGE_LOOP('',(#24348)) ;
#5317 = EDGE_LOOP('',(#24349,#24350,#24351)) ;
#5318 = EDGE_LOOP('',(#24352,#24353,#24354)) ;
#5319 = EDGE_LOOP('',(#24355,#24356,#24357,#24358)) ;
#5320 = EDGE_LOOP('',(#24359,#24360,#24361)) ;
#5321 = EDGE_LOOP('',(#24362,#24363,#24364,#24365,#24366,#24367)) ;
#5322 = EDGE_LOOP('',(#24368,#24369,#24370)) ;
#5323 = EDGE_LOOP('',(#24371,#24372,#24373)) ;
#5324 = EDGE_LOOP('',(#24374,#24375,#24376)) ;
#5325 = EDGE_LOOP('',(#24377,#24378,#24379,#24380,#24381,#24382)) ;
#5326 = EDGE_LOOP('',(#24383,#24384,#24385)) ;
#5327 = EDGE_LOOP('',(#24386,#24387,#24388)) ;
#5328 = EDGE_LOOP('',(#24389,#24390,#24391)) ;
#5329 = EDGE_LOOP('',(#24392,#24393,#24394,#24395,#24396,#24397)) ;
#5330 = EDGE_LOOP('',(#24398,#24399,#24400)) ;
#5331 = EDGE_LOOP('',(#24401,#24402,#24403)) ;
#5332 = EDGE_LOOP('',(#24404,#24405,#24406)) ;
#5333 = EDGE_LOOP('',(#24407,#24408,#24409,#24410,#24411,#24412)) ;
#5334 = EDGE_LOOP('',(#24413,#24414,#24415)) ;
#5335 = EDGE_LOOP('',(#24416,#24417,#24418)) ;
#5336 = EDGE_LOOP('',(#24419,#24420,#24421)) ;
#5337 = EDGE_LOOP('',(#24422,#24423,#24424,#24425,#24426,#24427)) ;
#5338 = EDGE_LOOP('',(#24428,#24429,#24430)) ;
#5339 = EDGE_LOOP('',(#24431,#24432,#24433)) ;
#5340 = EDGE_LOOP('',(#24434,#24435,#24436)) ;
#5341 = EDGE_LOOP('',(#24437,#24438,#24439,#24440,#24441,#24442)) ;
#5342 = EDGE_LOOP('',(#24443,#24444,#24445)) ;
#5343 = EDGE_LOOP('',(#24446,#24447,#24448)) ;
#5344 = EDGE_LOOP('',(#24449,#24450,#24451)) ;
#5345 = EDGE_LOOP('',(#24452,#24453,#24454,#24455,#24456,#24457)) ;
#5346 = EDGE_LOOP('',(#24458,#24459,#24460)) ;
#5347 = EDGE_LOOP('',(#24461,#24462,#24463)) ;
#5348 = EDGE_LOOP('',(#24464,#24465,#24466)) ;
#5349 = EDGE_LOOP('',(#24467,#24468,#24469,#24470,#24471,#24472)) ;
#5350 = EDGE_LOOP('',(#24473,#24474,#24475)) ;
#5351 = EDGE_LOOP('',(#24476,#24477,#24478)) ;
#5352 = EDGE_LOOP('',(#24479,#24480,#24481)) ;
#5353 = EDGE_LOOP('',(#24482,#24483,#24484,#24485,#24486,#24487)) ;
#5354 = EDGE_LOOP('',(#24488,#24489,#24490)) ;
#5355 = EDGE_LOOP('',(#24491,#24492,#24493)) ;
#5356 = EDGE_LOOP('',(#24494,#24495,#24496)) ;
#5357 = EDGE_LOOP('',(#24497,#24498,#24499,#24500,#24501,#24502)) ;
#5358 = EDGE_LOOP('',(#24503,#24504,#24505)) ;
#5359 = EDGE_LOOP('',(#24506,#24507,#24508)) ;
#5360 = EDGE_LOOP('',(#24509,#24510,#24511)) ;
#5361 = EDGE_LOOP('',(#24512,#24513,#24514,#24515,#24516,#24517)) ;
#5362 = EDGE_LOOP('',(#24518,#24519,#24520)) ;
#5363 = EDGE_LOOP('',(#24521,#24522,#24523)) ;
#5364 = EDGE_LOOP('',(#24524,#24525,#24526)) ;
#5365 = EDGE_LOOP('',(#24527,#24528,#24529,#24530,#24531,#24532)) ;
#5366 = EDGE_LOOP('',(#24533,#24534,#24535)) ;
#5367 = EDGE_LOOP('',(#24536,#24537,#24538)) ;
#5368 = EDGE_LOOP('',(#24539,#24540,#24541)) ;
#5369 = EDGE_LOOP('',(#24542,#24543,#24544,#24545,#24546,#24547)) ;
#5370 = EDGE_LOOP('',(#24548,#24549,#24550)) ;
#5371 = EDGE_LOOP('',(#24551,#24552,#24553)) ;
#5372 = EDGE_LOOP('',(#24554,#24555,#24556)) ;
#5373 = EDGE_LOOP('',(#24557,#24558,#24559,#24560,#24561,#24562)) ;
#5374 = EDGE_LOOP('',(#24563,#24564,#24565)) ;
#5375 = EDGE_LOOP('',(#24566,#24567,#24568)) ;
#5376 = EDGE_LOOP('',(#24569,#24570,#24571)) ;
#5377 = EDGE_LOOP('',(#24572,#24573,#24574,#24575,#24576,#24577)) ;
#5378 = EDGE_LOOP('',(#24578,#24579,#24580)) ;
#5379 = EDGE_LOOP('',(#24581,#24582,#24583)) ;
#5380 = EDGE_LOOP('',(#24584,#24585,#24586)) ;
#5381 = EDGE_LOOP('',(#24587,#24588,#24589,#24590,#24591,#24592)) ;
#5382 = EDGE_LOOP('',(#24593,#24594,#24595)) ;
#5383 = EDGE_LOOP('',(#24596,#24597,#24598)) ;
#5384 = EDGE_LOOP('',(#24599,#24600,#24601)) ;
#5385 = EDGE_LOOP('',(#24602,#24603,#24604,#24605,#24606,#24607)) ;
#5386 = EDGE_LOOP('',(#24608,#24609,#24610)) ;
#5387 = EDGE_LOOP('',(#24611,#24612,#24613)) ;
#5388 = EDGE_LOOP('',(#24614,#24615,#24616)) ;
#5389 = EDGE_LOOP('',(#24617,#24618,#24619,#24620,#24621,#24622)) ;
#5390 = EDGE_LOOP('',(#24623,#24624,#24625)) ;
#5391 = EDGE_LOOP('',(#24626,#24627,#24628)) ;
#5392 = EDGE_LOOP('',(#24629,#24630,#24631)) ;
#5393 = EDGE_LOOP('',(#24632,#24633,#24634,#24635,#24636,#24637)) ;
#5394 = EDGE_LOOP('',(#24638,#24639,#24640)) ;
#5395 = EDGE_LOOP('',(#24641,#24642,#24643)) ;
#5396 = EDGE_LOOP('',(#24644,#24645,#24646)) ;
#5397 = EDGE_LOOP('',(#24647,#24648,#24649,#24650,#24651,#24652)) ;
#5398 = EDGE_LOOP('',(#24653,#24654,#24655)) ;
#5399 = EDGE_LOOP('',(#24656,#24657,#24658)) ;
#5400 = EDGE_LOOP('',(#24659,#24660,#24661)) ;
#5401 = EDGE_LOOP('',(#24662,#24663,#24664,#24665,#24666,#24667)) ;
#5402 = EDGE_LOOP('',(#24668,#24669,#24670)) ;
#5403 = EDGE_LOOP('',(#24671,#24672,#24673)) ;
#5404 = EDGE_LOOP('',(#24674,#24675,#24676)) ;
#5405 = EDGE_LOOP('',(#24677,#24678,#24679,#24680,#24681,#24682)) ;
#5406 = EDGE_LOOP('',(#24683,#24684,#24685)) ;
#5407 = EDGE_LOOP('',(#24686,#24687,#24688)) ;
#5408 = EDGE_LOOP('',(#24689,#24690,#24691)) ;
#5409 = EDGE_LOOP('',(#24692,#24693,#24694,#24695,#24696,#24697)) ;
#5410 = EDGE_LOOP('',(#24698,#24699,#24700)) ;
#5411 = EDGE_LOOP('',(#24701,#24702,#24703)) ;
#5412 = EDGE_LOOP('',(#24704,#24705,#24706)) ;
#5413 = EDGE_LOOP('',(#24707,#24708,#24709,#24710,#24711,#24712)) ;
#5414 = EDGE_LOOP('',(#24713,#24714,#24715)) ;
#5415 = EDGE_LOOP('',(#24716,#24717,#24718)) ;
#5416 = EDGE_LOOP('',(#24719,#24720,#24721)) ;
#5417 = EDGE_LOOP('',(#24722,#24723,#24724,#24725,#24726,#24727)) ;
#5418 = EDGE_LOOP('',(#24728,#24729,#24730)) ;
#5419 = EDGE_LOOP('',(#24731,#24732,#24733)) ;
#5420 = EDGE_LOOP('',(#24734,#24735,#24736)) ;
#5421 = EDGE_LOOP('',(#24737,#24738,#24739,#24740,#24741,#24742)) ;
#5422 = EDGE_LOOP('',(#24743,#24744,#24745)) ;
#5423 = EDGE_LOOP('',(#24746,#24747,#24748)) ;
#5424 = EDGE_LOOP('',(#24749,#24750,#24751)) ;
#5425 = EDGE_LOOP('',(#24752,#24753,#24754,#24755,#24756,#24757)) ;
#5426 = EDGE_LOOP('',(#24758,#24759,#24760)) ;
#5427 = EDGE_LOOP('',(#24761,#24762,#24763)) ;
#5428 = EDGE_LOOP('',(#24764,#24765,#24766)) ;
#5429 = EDGE_LOOP('',(#24767,#24768,#24769,#24770,#24771,#24772)) ;
#5430 = EDGE_LOOP('',(#24773,#24774,#24775)) ;
#5431 = EDGE_LOOP('',(#24776,#24777,#24778)) ;
#5432 = EDGE_LOOP('',(#24779,#24780,#24781)) ;
#5433 = EDGE_LOOP('',(#24782,#24783,#24784,#24785,#24786,#24787)) ;
#5434 = EDGE_LOOP('',(#24788,#24789,#24790)) ;
#5435 = EDGE_LOOP('',(#24791,#24792,#24793)) ;
#5436 = EDGE_LOOP('',(#24794,#24795,#24796)) ;
#5437 = EDGE_LOOP('',(#24797,#24798,#24799,#24800,#24801,#24802)) ;
#5438 = EDGE_LOOP('',(#24803,#24804,#24805)) ;
#5439 = EDGE_LOOP('',(#24806,#24807,#24808)) ;
#5440 = EDGE_LOOP('',(#24809,#24810,#24811)) ;
#5441 = EDGE_LOOP('',(#24812,#24813,#24814,#24815,#24816,#24817)) ;
#5442 = EDGE_LOOP('',(#24818,#24819,#24820)) ;
#5443 = EDGE_LOOP('',(#24821,#24822,#24823)) ;
#5444 = EDGE_LOOP('',(#24824,#24825,#24826)) ;
#5445 = EDGE_LOOP('',(#24827,#24828,#24829,#24830,#24831)) ;
#5446 = EDGE_LOOP('',(#24832,#24833,#24834,#24835,#24836,#24837)) ;
#5447 = EDGE_LOOP('',(#24838,#24839,#24840,#24841,#24842,#24843,#24844,#24845,
#24846,#24847)) ;
#5448 = EDGE_LOOP('',(#24848,#24849,#24850,#24851,#24852,#24853,#24854,#24855,
#24856)) ;
#5449 = EDGE_LOOP('',(#24857,#24858,#24859,#24860,#24861,#24862,#24863,#24864,
#24865,#24866)) ;
#5450 = EDGE_LOOP('',(#24867,#24868,#24869,#24870,#24871,#24872,#24873,#24874,
#24875)) ;
#5451 = EDGE_LOOP('',(#24876,#24877,#24878,#24879,#24880,#24881,#24882,#24883,
#24884)) ;
#5452 = EDGE_LOOP('',(#24885,#24886,#24887,#24888,#24889,#24890,#24891,#24892,
#24893)) ;
#5453 = EDGE_LOOP('',(#24894,#24895,#24896,#24897,#24898,#24899,#24900,#24901,
#24902,#24903)) ;
#5454 = EDGE_LOOP('',(#24904,#24905,#24906,#24907,#24908,#24909,#24910,#24911,
#24912)) ;
#5455 = EDGE_LOOP('',(#24913,#24914,#24915,#24916,#24917,#24918,#24919,#24920,
#24921)) ;
#5456 = EDGE_LOOP('',(#24922,#24923,#24924,#24925,#24926,#24927,#24928,#24929,
#24930)) ;
#5457 = EDGE_LOOP('',(#24931,#24932,#24933,#24934,#24935,#24936,#24937,#24938,
#24939,#24940)) ;
#5458 = EDGE_LOOP('',(#24941,#24942,#24943,#24944,#24945,#24946,#24947,#24948,
#24949)) ;
#5459 = EDGE_LOOP('',(#24950,#24951,#24952,#24953,#24954,#24955,#24956,#24957,
#24958)) ;
#5460 = EDGE_LOOP('',(#24959,#24960,#24961,#24962,#24963,#24964,#24965,#24966,
#24967)) ;
#5461 = EDGE_LOOP('',(#24968,#24969,#24970,#24971,#24972,#24973,#24974,#24975,
#24976,#24977)) ;
#5462 = EDGE_LOOP('',(#24978,#24979,#24980,#24981,#24982,#24983,#24984,#24985,
#24986)) ;
#5463 = EDGE_LOOP('',(#24987,#24988,#24989,#24990,#24991,#24992,#24993,#24994,
#24995)) ;
#5464 = EDGE_LOOP('',(#24996,#24997,#24998,#24999,#25000,#25001,#25002,#25003,
#25004)) ;
#5465 = EDGE_LOOP('',(#25005,#25006,#25007,#25008,#25009,#25010,#25011,#25012,
#25013,#25014)) ;
#5466 = EDGE_LOOP('',(#25015,#25016,#25017,#25018,#25019,#25020,#25021,#25022,
#25023)) ;
#5467 = EDGE_LOOP('',(#25024,#25025,#25026,#25027,#25028,#25029,#25030,#25031,
#25032)) ;
#5468 = EDGE_LOOP('',(#25033,#25034,#25035,#25036,#25037,#25038,#25039,#25040,
#25041)) ;
#5469 = EDGE_LOOP('',(#25042,#25043,#25044,#25045,#25046,#25047,#25048,#25049,
#25050,#25051)) ;
#5470 = EDGE_LOOP('',(#25052,#25053,#25054,#25055,#25056,#25057,#25058,#25059,
#25060)) ;
#5471 = EDGE_LOOP('',(#25061,#25062,#25063,#25064,#25065,#25066,#25067,#25068,
#25069)) ;
#5472 = EDGE_LOOP('',(#25070,#25071,#25072,#25073,#25074,#25075,#25076,#25077,
#25078)) ;
#5473 = EDGE_LOOP('',(#25079,#25080,#25081,#25082,#25083,#25084,#25085,#25086,
#25087,#25088)) ;
#5474 = EDGE_LOOP('',(#25089,#25090,#25091,#25092,#25093,#25094,#25095,#25096,
#25097)) ;
#5475 = EDGE_LOOP('',(#25098,#25099,#25100,#25101,#25102,#25103,#25104,#25105,
#25106)) ;
#5476 = EDGE_LOOP('',(#25107,#25108,#25109,#25110,#25111,#25112,#25113,#25114,
#25115)) ;
#5477 = EDGE_LOOP('',(#25116,#25117,#25118,#25119,#25120,#25121,#25122,#25123,
#25124,#25125)) ;
#5478 = EDGE_LOOP('',(#25126,#25127,#25128,#25129,#25130,#25131,#25132,#25133,
#25134)) ;
#5479 = EDGE_LOOP('',(#25135,#25136,#25137,#25138,#25139,#25140,#25141,#25142,
#25143)) ;
#5480 = EDGE_LOOP('',(#25144,#25145,#25146,#25147,#25148,#25149,#25150,#25151,
#25152)) ;
#5481 = EDGE_LOOP('',(#25153,#25154,#25155,#25156,#25157,#25158,#25159,#25160,
#25161,#25162)) ;
#5482 = EDGE_LOOP('',(#25163,#25164,#25165,#25166,#25167,#25168,#25169,#25170,
#25171)) ;
#5483 = EDGE_LOOP('',(#25172,#25173,#25174,#25175,#25176,#25177,#25178,#25179,
#25180)) ;
#5484 = EDGE_LOOP('',(#25181,#25182,#25183,#25184,#25185,#25186,#25187,#25188,
#25189)) ;
#5485 = EDGE_LOOP('',(#25190,#25191,#25192,#25193,#25194,#25195,#25196,#25197,
#25198,#25199)) ;
#5486 = EDGE_LOOP('',(#25200,#25201,#25202,#25203,#25204,#25205,#25206,#25207,
#25208)) ;
#5487 = EDGE_LOOP('',(#25209,#25210,#25211,#25212,#25213,#25214,#25215,#25216,
#25217)) ;
#5488 = EDGE_LOOP('',(#25218,#25219,#25220,#25221,#25222,#25223,#25224,#25225,
#25226)) ;
#5489 = EDGE_LOOP('',(#25227,#25228,#25229,#25230,#25231,#25232,#25233,#25234,
#25235,#25236)) ;
#5490 = EDGE_LOOP('',(#25237,#25238,#25239,#25240,#25241,#25242,#25243,#25244,
#25245)) ;
#5491 = EDGE_LOOP('',(#25246,#25247,#25248,#25249,#25250,#25251,#25252,#25253,
#25254)) ;
#5492 = EDGE_LOOP('',(#25255,#25256,#25257,#25258,#25259,#25260,#25261,#25262,
#25263)) ;
#5493 = EDGE_LOOP('',(#25264,#25265,#25266,#25267,#25268,#25269,#25270,#25271,
#25272,#25273)) ;
#5494 = EDGE_LOOP('',(#25274,#25275,#25276,#25277,#25278,#25279,#25280,#25281,
#25282)) ;
#5495 = EDGE_LOOP('',(#25283,#25284,#25285,#25286,#25287,#25288,#25289,#25290,
#25291)) ;
#5496 = EDGE_LOOP('',(#25292,#25293,#25294,#25295,#25296,#25297,#25298,#25299,
#25300)) ;
#5497 = EDGE_LOOP('',(#25301,#25302,#25303,#25304,#25305,#25306,#25307,#25308,
#25309,#25310)) ;
#5498 = EDGE_LOOP('',(#25311,#25312,#25313,#25314,#25315,#25316,#25317,#25318,
#25319)) ;
#5499 = EDGE_LOOP('',(#25320,#25321,#25322,#25323,#25324,#25325,#25326,#25327,
#25328)) ;
#5500 = EDGE_LOOP('',(#25329,#25330,#25331,#25332,#25333,#25334,#25335,#25336,
#25337)) ;
#5501 = EDGE_LOOP('',(#25338,#25339,#25340,#25341,#25342,#25343,#25344,#25345,
#25346,#25347)) ;
#5502 = EDGE_LOOP('',(#25348,#25349,#25350,#25351,#25352,#25353,#25354,#25355,
#25356)) ;
#5503 = EDGE_LOOP('',(#25357,#25358,#25359,#25360,#25361,#25362,#25363,#25364,
#25365)) ;
#5504 = EDGE_LOOP('',(#25366,#25367,#25368,#25369,#25370,#25371,#25372,#25373,
#25374)) ;
#5505 = EDGE_LOOP('',(#25375,#25376,#25377,#25378,#25379,#25380,#25381,#25382,
#25383,#25384)) ;
#5506 = EDGE_LOOP('',(#25385,#25386,#25387,#25388,#25389,#25390,#25391,#25392,
#25393)) ;
#5507 = EDGE_LOOP('',(#25394,#25395,#25396,#25397,#25398,#25399,#25400,#25401,
#25402)) ;
#5508 = EDGE_LOOP('',(#25403,#25404,#25405,#25406,#25407,#25408,#25409,#25410,
#25411)) ;
#5509 = EDGE_LOOP('',(#25412,#25413,#25414,#25415,#25416,#25417,#25418,#25419,
#25420,#25421)) ;
#5510 = EDGE_LOOP('',(#25422,#25423,#25424,#25425,#25426,#25427,#25428,#25429,
#25430)) ;
#5511 = EDGE_LOOP('',(#25431,#25432,#25433,#25434,#25435,#25436,#25437,#25438,
#25439)) ;
#5512 = EDGE_LOOP('',(#25440,#25441,#25442,#25443,#25444,#25445,#25446,#25447,
#25448)) ;
#5513 = EDGE_LOOP('',(#25449,#25450,#25451,#25452,#25453,#25454,#25455,#25456,
#25457,#25458)) ;
#5514 = EDGE_LOOP('',(#25459,#25460,#25461,#25462,#25463,#25464,#25465,#25466,
#25467)) ;
#5515 = EDGE_LOOP('',(#25468,#25469,#25470,#25471,#25472,#25473,#25474,#25475,
#25476)) ;
#5516 = EDGE_LOOP('',(#25477,#25478,#25479,#25480,#25481,#25482,#25483,#25484,
#25485)) ;
#5517 = EDGE_LOOP('',(#25486,#25487,#25488,#25489,#25490,#25491,#25492,#25493,
#25494,#25495)) ;
#5518 = EDGE_LOOP('',(#25496,#25497,#25498,#25499,#25500,#25501,#25502,#25503,
#25504)) ;
#5519 = EDGE_LOOP('',(#25505,#25506,#25507,#25508,#25509,#25510,#25511,#25512,
#25513)) ;
#5520 = EDGE_LOOP('',(#25514,#25515,#25516,#25517,#25518,#25519,#25520,#25521,
#25522)) ;
#5521 = EDGE_LOOP('',(#25523,#25524,#25525,#25526,#25527,#25528,#25529,#25530,
#25531,#25532)) ;
#5522 = EDGE_LOOP('',(#25533,#25534,#25535,#25536,#25537,#25538,#25539,#25540,
#25541)) ;
#5523 = EDGE_LOOP('',(#25542,#25543,#25544,#25545,#25546,#25547,#25548,#25549,
#25550)) ;
#5524 = EDGE_LOOP('',(#25551,#25552,#25553,#25554,#25555,#25556,#25557,#25558,
#25559)) ;
#5525 = EDGE_LOOP('',(#25560,#25561,#25562,#25563,#25564,#25565,#25566,#25567,
#25568,#25569)) ;
#5526 = EDGE_LOOP('',(#25570,#25571,#25572,#25573,#25574,#25575,#25576,#25577,
#25578)) ;
#5527 = EDGE_LOOP('',(#25579,#25580,#25581,#25582,#25583,#25584,#25585,#25586,
#25587)) ;
#5528 = EDGE_LOOP('',(#25588,#25589,#25590,#25591,#25592,#25593,#25594,#25595,
#25596)) ;
#5529 = EDGE_LOOP('',(#25597,#25598,#25599,#25600,#25601,#25602,#25603,#25604,
#25605,#25606)) ;
#5530 = EDGE_LOOP('',(#25607,#25608,#25609,#25610,#25611,#25612,#25613,#25614,
#25615)) ;
#5531 = EDGE_LOOP('',(#25616,#25617,#25618,#25619,#25620,#25621,#25622,#25623,
#25624)) ;
#5532 = EDGE_LOOP('',(#25625,#25626,#25627,#25628,#25629,#25630,#25631,#25632,
#25633)) ;
#5533 = EDGE_LOOP('',(#25634,#25635,#25636,#25637,#25638,#25639,#25640,#25641,
#25642,#25643)) ;
#5534 = EDGE_LOOP('',(#25644,#25645,#25646,#25647,#25648,#25649,#25650,#25651,
#25652)) ;
#5535 = EDGE_LOOP('',(#25653,#25654,#25655,#25656,#25657,#25658,#25659,#25660,
#25661)) ;
#5536 = EDGE_LOOP('',(#25662,#25663,#25664,#25665,#25666,#25667,#25668,#25669,
#25670)) ;
#5537 = EDGE_LOOP('',(#25671,#25672,#25673,#25674,#25675,#25676,#25677,#25678,
#25679,#25680)) ;
#5538 = EDGE_LOOP('',(#25681,#25682,#25683,#25684,#25685,#25686,#25687,#25688,
#25689)) ;
#5539 = EDGE_LOOP('',(#25690,#25691,#25692,#25693,#25694,#25695,#25696,#25697,
#25698)) ;
#5540 = EDGE_LOOP('',(#25699,#25700,#25701,#25702,#25703,#25704,#25705,#25706,
#25707)) ;
#5541 = EDGE_LOOP('',(#25708,#25709,#25710,#25711,#25712,#25713,#25714,#25715,
#25716,#25717)) ;
#5542 = EDGE_LOOP('',(#25718,#25719,#25720,#25721,#25722,#25723,#25724,#25725,
#25726)) ;
#5543 = EDGE_LOOP('',(#25727,#25728,#25729,#25730,#25731,#25732,#25733,#25734,
#25735)) ;
#5544 = EDGE_LOOP('',(#25736,#25737,#25738,#25739,#25740,#25741,#25742,#25743,
#25744)) ;
#5545 = EDGE_LOOP('',(#25745,#25746,#25747,#25748,#25749,#25750,#25751,#25752,
#25753,#25754)) ;
#5546 = EDGE_LOOP('',(#25755,#25756,#25757,#25758,#25759,#25760,#25761,#25762,
#25763)) ;
#5547 = EDGE_LOOP('',(#25764,#25765,#25766,#25767,#25768,#25769,#25770,#25771,
#25772)) ;
#5548 = EDGE_LOOP('',(#25773,#25774,#25775,#25776,#25777,#25778,#25779,#25780,
#25781)) ;
#5549 = EDGE_LOOP('',(#25782,#25783,#25784,#25785,#25786,#25787,#25788,#25789,
#25790,#25791)) ;
#5550 = EDGE_LOOP('',(#25792,#25793,#25794,#25795,#25796,#25797,#25798,#25799,
#25800)) ;
#5551 = EDGE_LOOP('',(#25801,#25802,#25803,#25804,#25805,#25806,#25807,#25808,
#25809)) ;
#5552 = EDGE_LOOP('',(#25810,#25811,#25812,#25813,#25814,#25815,#25816,#25817,
#25818)) ;
#5553 = EDGE_LOOP('',(#25819,#25820,#25821,#25822,#25823,#25824,#25825,#25826,
#25827,#25828)) ;
#5554 = EDGE_LOOP('',(#25829,#25830,#25831,#25832,#25833,#25834,#25835,#25836,
#25837)) ;
#5555 = EDGE_LOOP('',(#25838,#25839,#25840,#25841,#25842,#25843,#25844,#25845,
#25846)) ;
#5556 = EDGE_LOOP('',(#25847,#25848,#25849,#25850,#25851,#25852,#25853,#25854,
#25855)) ;
#5557 = EDGE_LOOP('',(#25856,#25857,#25858,#25859,#25860,#25861,#25862,#25863,
#25864,#25865)) ;
#5558 = EDGE_LOOP('',(#25866,#25867,#25868,#25869,#25870,#25871,#25872,#25873,
#25874)) ;
#5559 = EDGE_LOOP('',(#25875,#25876,#25877,#25878,#25879,#25880,#25881,#25882,
#25883)) ;
#5560 = EDGE_LOOP('',(#25884,#25885,#25886,#25887,#25888,#25889,#25890,#25891,
#25892)) ;
#5561 = EDGE_LOOP('',(#25893,#25894,#25895,#25896,#25897,#25898,#25899,#25900,
#25901,#25902)) ;
#5562 = EDGE_LOOP('',(#25903,#25904,#25905,#25906,#25907,#25908,#25909,#25910,
#25911)) ;
#5563 = EDGE_LOOP('',(#25912,#25913,#25914,#25915,#25916,#25917,#25918,#25919,
#25920)) ;
#5564 = EDGE_LOOP('',(#25921,#25922,#25923,#25924,#25925,#25926,#25927,#25928,
#25929)) ;
#5565 = EDGE_LOOP('',(#25930,#25931,#25932,#25933,#25934,#25935,#25936,#25937,
#25938,#25939)) ;
#5566 = EDGE_LOOP('',(#25940,#25941,#25942,#25943,#25944,#25945,#25946,#25947,
#25948)) ;
#5567 = EDGE_LOOP('',(#25949,#25950,#25951,#25952,#25953,#25954,#25955,#25956,
#25957)) ;
#5568 = EDGE_LOOP('',(#25958,#25959,#25960,#25961,#25962,#25963,#25964,#25965,
#25966)) ;
#5569 = EDGE_LOOP('',(#25967,#25968,#25969,#25970,#25971,#25972,#25973,#25974,
#25975,#25976)) ;
#5570 = EDGE_LOOP('',(#25977,#25978,#25979,#25980,#25981,#25982,#25983,#25984,
#25985)) ;
#5571 = EDGE_LOOP('',(#25986,#25987,#25988,#25989,#25990,#25991,#25992,#25993,
#25994)) ;
#5572 = EDGE_LOOP('',(#25995,#25996,#25997,#25998,#25999,#26000,#26001)) ;
#5573 = EDGE_LOOP('',(#26002)) ;
#5574 = EDGE_LOOP('',(#26003,#26004,#26005,#26006,#26007,#26008,#26009,#26010,
#26011)) ;
#5575 = EDGE_LOOP('',(#26012,#26013,#26014,#26015)) ;
#5576 = EDGE_LOOP('',(#26016)) ;
#5577 = EDGE_LOOP('',(#26017)) ;
#5578 = EDGE_LOOP('',(#26018)) ;
#5579 = EDGE_LOOP('',(#26019)) ;
#5580 = EDGE_LOOP('',(#26020,#26021,#26022,#26023,#26024,#26025)) ;
#5581 = EDGE_LOOP('',(#26026)) ;
#5582 = EDGE_LOOP('',(#26027,#26028)) ;
#5583 = EDGE_LOOP('',(#26029,#26030)) ;
#5584 = EDGE_LOOP('',(#26031,#26032)) ;
#5585 = EDGE_LOOP('',(#26033,#26034)) ;
#5586 = EDGE_LOOP('',(#26035)) ;
#5587 = EDGE_LOOP('',(#26036)) ;
#5588 = EDGE_LOOP('',(#26037,#26038)) ;
#5589 = EDGE_LOOP('',(#26039,#26040,#26041,#26042,#26043,#26044)) ;
#5590 = EDGE_LOOP('',(#26045)) ;
#5591 = EDGE_LOOP('',(#26046)) ;
#5592 = EDGE_LOOP('',(#26047,#26048)) ;
#5593 = EDGE_LOOP('',(#26049,#26050,#26051,#26052,#26053,#26054)) ;
#5594 = EDGE_LOOP('',(#26055,#26056,#26057,#26058,#26059,#26060)) ;
#5595 = EDGE_LOOP('',(#26061,#26062,#26063,#26064,#26065,#26066)) ;
#5596 = EDGE_LOOP('',(#26067,#26068,#26069)) ;
#5597 = EDGE_LOOP('',(#26070,#26071,#26072,#26073)) ;
#5598 = EDGE_LOOP('',(#26074,#26075,#26076,#26077,#26078)) ;
#5599 = EDGE_LOOP('',(#26079,#26080,#26081,#26082)) ;
#5600 = EDGE_LOOP('',(#26083)) ;
#5601 = EDGE_LOOP('',(#26084,#26085,#26086,#26087)) ;
#5602 = EDGE_LOOP('',(#26088,#26089,#26090,#26091,#26092)) ;
#5603 = EDGE_LOOP('',(#26093,#26094,#26095,#26096,#26097)) ;
#5604 = EDGE_LOOP('',(#26098,#26099,#26100,#26101)) ;
#5605 = EDGE_LOOP('',(#26102)) ;
#5606 = EDGE_LOOP('',(#26103,#26104,#26105,#26106)) ;
#5607 = EDGE_LOOP('',(#26107,#26108,#26109,#26110)) ;
#5608 = EDGE_LOOP('',(#26111,#26112,#26113,#26114)) ;
#5609 = EDGE_LOOP('',(#26115)) ;
#5610 = EDGE_LOOP('',(#26116,#26117)) ;
#5611 = EDGE_LOOP('',(#26118,#26119,#26120,#26121,#26122,#26123,#26124,#26125,
#26126)) ;
#5612 = EDGE_LOOP('',(#26127,#26128)) ;
#5613 = EDGE_LOOP('',(#26129,#26130)) ;
#5614 = EDGE_LOOP('',(#26131,#26132,#26133,#26134,#26135,#26136)) ;
#5615 = EDGE_LOOP('',(#26137,#26138,#26139,#26140,#26141,#26142)) ;
#5616 = EDGE_LOOP('',(#26143,#26144)) ;
#5617 = EDGE_LOOP('',(#26145,#26146,#26147,#26148,#26149,#26150,#26151,#26152,
#26153)) ;
#5618 = EDGE_LOOP('',(#26154,#26155)) ;
#5619 = EDGE_LOOP('',(#26156)) ;
#5620 = EDGE_LOOP('',(#26157,#26158)) ;
#5621 = EDGE_LOOP('',(#26159,#26160,#26161,#26162,#26163,#26164,#26165,#26166)) ;
#5622 = EDGE_LOOP('',(#26167,#26168)) ;
#5623 = EDGE_LOOP('',(#26169,#26170)) ;
#5624 = EDGE_LOOP('',(#26171)) ;
#5625 = EDGE_LOOP('',(#26172,#26173)) ;
#5626 = EDGE_LOOP('',(#26174)) ;
#5627 = EDGE_LOOP('',(#26175,#26176,#26177,#26178,#26179,#26180,#26181,#26182)) ;
#5628 = EDGE_LOOP('',(#26183,#26184,#26185,#26186)) ;
#5629 = EDGE_LOOP('',(#26187,#26188,#26189,#26190)) ;
#5630 = EDGE_LOOP('',(#26191,#26192,#26193,#26194)) ;
#5631 = EDGE_LOOP('',(#26195)) ;
#5632 = EDGE_LOOP('',(#26196)) ;
#5633 = EDGE_LOOP('',(#26197)) ;
#5634 = EDGE_LOOP('',(#26198)) ;
#5635 = EDGE_LOOP('',(#26199,#26200,#26201,#26202)) ;
#5636 = EDGE_LOOP('',(#26203,#26204,#26205,#26206,#26207,#26208)) ;
#5637 = EDGE_LOOP('',(#26209,#26210,#26211,#26212)) ;
#5638 = EDGE_LOOP('',(#26213,#26214,#26215,#26216)) ;
#5639 = EDGE_LOOP('',(#26217,#26218,#26219,#26220)) ;
#5640 = EDGE_LOOP('',(#26221,#26222,#26223,#26224)) ;
#5641 = EDGE_LOOP('',(#26225,#26226,#26227,#26228)) ;
#5642 = EDGE_LOOP('',(#26229,#26230,#26231,#26232,#26233,#26234)) ;
#5643 = EDGE_LOOP('',(#26235,#26236,#26237,#26238)) ;
#5644 = EDGE_LOOP('',(#26239,#26240,#26241,#26242)) ;
#5645 = EDGE_LOOP('',(#26243,#26244,#26245,#26246)) ;
#5646 = EDGE_LOOP('',(#26247,#26248,#26249,#26250)) ;
#5647 = EDGE_LOOP('',(#26251,#26252,#26253,#26254)) ;
#5648 = EDGE_LOOP('',(#26255,#26256,#26257,#26258)) ;
#5649 = EDGE_LOOP('',(#26259,#26260,#26261,#26262,#26263,#26264)) ;
#5650 = EDGE_LOOP('',(#26265,#26266,#26267,#26268)) ;
#5651 = EDGE_LOOP('',(#26269,#26270,#26271,#26272)) ;
#5652 = EDGE_LOOP('',(#26273,#26274,#26275,#26276)) ;
#5653 = EDGE_LOOP('',(#26277,#26278,#26279,#26280)) ;
#5654 = EDGE_LOOP('',(#26281,#26282,#26283,#26284,#26285,#26286)) ;
#5655 = EDGE_LOOP('',(#26287,#26288,#26289,#26290,#26291)) ;
#5656 = EDGE_LOOP('',(#26292)) ;
#5657 = EDGE_LOOP('',(#26293,#26294,#26295,#26296)) ;
#5658 = EDGE_LOOP('',(#26297,#26298,#26299,#26300,#26301,#26302,#26303,#26304)) ;
#5659 = EDGE_LOOP('',(#26305)) ;
#5660 = EDGE_LOOP('',(#26306)) ;
#5661 = EDGE_LOOP('',(#26307,#26308,#26309,#26310)) ;
#5662 = EDGE_LOOP('',(#26311)) ;
#5663 = EDGE_LOOP('',(#26312,#26313,#26314,#26315)) ;
#5664 = EDGE_LOOP('',(#26316,#26317,#26318,#26319)) ;
#5665 = EDGE_LOOP('',(#26320,#26321,#26322,#26323,#26324,#26325)) ;
#5666 = EDGE_LOOP('',(#26326,#26327,#26328,#26329)) ;
#5667 = EDGE_LOOP('',(#26330,#26331,#26332,#26333)) ;
#5668 = EDGE_LOOP('',(#26334,#26335,#26336,#26337)) ;
#5669 = EDGE_LOOP('',(#26338,#26339,#26340,#26341)) ;
#5670 = EDGE_LOOP('',(#26342,#26343,#26344,#26345,#26346,#26347)) ;
#5671 = EDGE_LOOP('',(#26348)) ;
#5672 = EDGE_LOOP('',(#26349,#26350,#26351,#26352)) ;
#5673 = EDGE_LOOP('',(#26353,#26354,#26355,#26356)) ;
#5674 = EDGE_LOOP('',(#26357,#26358,#26359,#26360)) ;
#5675 = EDGE_LOOP('',(#26361,#26362,#26363,#26364,#26365,#26366)) ;
#5676 = EDGE_LOOP('',(#26367)) ;
#5677 = EDGE_LOOP('',(#26368,#26369,#26370,#26371)) ;
#5678 = EDGE_LOOP('',(#26372,#26373,#26374,#26375)) ;
#5679 = EDGE_LOOP('',(#26376,#26377,#26378,#26379)) ;
#5680 = EDGE_LOOP('',(#26380,#26381,#26382,#26383)) ;
#5681 = EDGE_LOOP('',(#26384,#26385,#26386,#26387,#26388,#26389)) ;
#5682 = EDGE_LOOP('',(#26390)) ;
#5683 = EDGE_LOOP('',(#26391,#26392,#26393,#26394)) ;
#5684 = EDGE_LOOP('',(#26395)) ;
#5685 = EDGE_LOOP('',(#26396,#26397,#26398,#26399)) ;
#5686 = EDGE_LOOP('',(#26400,#26401,#26402,#26403)) ;
#5687 = EDGE_LOOP('',(#26404,#26405,#26406,#26407,#26408,#26409)) ;
#5688 = EDGE_LOOP('',(#26410,#26411,#26412,#26413)) ;
#5689 = EDGE_LOOP('',(#26414,#26415,#26416,#26417)) ;
#5690 = EDGE_LOOP('',(#26418,#26419,#26420,#26421)) ;
#5691 = EDGE_LOOP('',(#26422,#26423,#26424,#26425)) ;
#5692 = EDGE_LOOP('',(#26426,#26427,#26428,#26429,#26430,#26431)) ;
#5693 = EDGE_LOOP('',(#26432)) ;
#5694 = EDGE_LOOP('',(#26433,#26434,#26435,#26436)) ;
#5695 = EDGE_LOOP('',(#26437,#26438,#26439,#26440)) ;
#5696 = EDGE_LOOP('',(#26441,#26442,#26443,#26444)) ;
#5697 = EDGE_LOOP('',(#26445,#26446,#26447,#26448,#26449,#26450)) ;
#5698 = EDGE_LOOP('',(#26451)) ;
#5699 = EDGE_LOOP('',(#26452,#26453,#26454,#26455)) ;
#5700 = EDGE_LOOP('',(#26456,#26457,#26458,#26459)) ;
#5701 = EDGE_LOOP('',(#26460,#26461,#26462,#26463)) ;
#5702 = EDGE_LOOP('',(#26464,#26465,#26466,#26467)) ;
#5703 = EDGE_LOOP('',(#26468,#26469,#26470,#26471,#26472,#26473)) ;
#5704 = EDGE_LOOP('',(#26474)) ;
#5705 = EDGE_LOOP('',(#26475)) ;
#5706 = EDGE_LOOP('',(#26476)) ;
#5707 = EDGE_LOOP('',(#26477,#26478,#26479,#26480)) ;
#5708 = EDGE_LOOP('',(#26481)) ;
#5709 = EDGE_LOOP('',(#26482,#26483,#26484,#26485)) ;
#5710 = EDGE_LOOP('',(#26486)) ;
#5711 = EDGE_LOOP('',(#26487)) ;
#5712 = EDGE_LOOP('',(#26488)) ;
#5713 = EDGE_LOOP('',(#26489,#26490,#26491,#26492)) ;
#5714 = EDGE_LOOP('',(#26493)) ;
#5715 = EDGE_LOOP('',(#26494,#26495,#26496,#26497)) ;
#5716 = EDGE_LOOP('',(#26498)) ;
#5717 = EDGE_LOOP('',(#26499,#26500,#26501,#26502,#26503,#26504,#26505,#26506,
#26507,#26508)) ;
#5718 = EDGE_LOOP('',(#26509,#26510)) ;
#5719 = EDGE_LOOP('',(#26511,#26512)) ;
#5720 = EDGE_LOOP('',(#26513,#26514)) ;
#5721 = EDGE_LOOP('',(#26515,#26516,#26517,#26518,#26519)) ;
#5722 = EDGE_LOOP('',(#26520,#26521,#26522,#26523)) ;
#5723 = EDGE_LOOP('',(#26524,#26525,#26526,#26527)) ;
#5724 = EDGE_LOOP('',(#26528,#26529,#26530,#26531)) ;
#5725 = EDGE_LOOP('',(#26532,#26533,#26534,#26535)) ;
#5726 = EDGE_LOOP('',(#26536,#26537,#26538,#26539)) ;
#5727 = EDGE_LOOP('',(#26540,#26541)) ;
#5728 = EDGE_LOOP('',(#26542,#26543)) ;
#5729 = EDGE_LOOP('',(#26544,#26545,#26546,#26547,#26548,#26549,#26550,#26551)) ;
#5730 = EDGE_LOOP('',(#26552,#26553,#26554,#26555,#26556,#26557,#26558,#26559)) ;
#5731 = EDGE_LOOP('',(#26560,#26561,#26562,#26563,#26564,#26565,#26566,#26567)) ;
#5732 = EDGE_LOOP('',(#26568,#26569,#26570,#26571,#26572,#26573,#26574,#26575,
#26576)) ;
#5733 = EDGE_LOOP('',(#26577,#26578,#26579,#26580,#26581,#26582,#26583,#26584)) ;
#5734 = EDGE_LOOP('',(#26585,#26586,#26587,#26588,#26589,#26590,#26591,#26592)) ;
#5735 = EDGE_LOOP('',(#26593,#26594,#26595,#26596,#26597,#26598,#26599,#26600)) ;
#5736 = EDGE_LOOP('',(#26601,#26602,#26603,#26604,#26605,#26606,#26607,#26608)) ;
#5737 = EDGE_LOOP('',(#26609,#26610,#26611,#26612,#26613,#26614,#26615,#26616,
#26617,#26618,#26619)) ;
#5738 = EDGE_LOOP('',(#26620,#26621,#26622,#26623,#26624,#26625,#26626,#26627)) ;
#5739 = EDGE_LOOP('',(#26628,#26629,#26630,#26631,#26632,#26633,#26634,#26635)) ;
#5740 = EDGE_LOOP('',(#26636,#26637,#26638)) ;
#5741 = EDGE_LOOP('',(#26639,#26640,#26641,#26642,#26643,#26644,#26645,#26646)) ;
#5742 = EDGE_LOOP('',(#26647)) ;
#5743 = EDGE_LOOP('',(#26648,#26649,#26650)) ;
#5744 = LINE('',#41230,#8216) ;
#5745 = LINE('',#41235,#8217) ;
#5746 = LINE('',#41237,#8218) ;
#5747 = LINE('',#41239,#8219) ;
#5748 = LINE('',#41241,#8220) ;
#5749 = LINE('',#41243,#8221) ;
#5750 = LINE('',#41245,#8222) ;
#5751 = LINE('',#41247,#8223) ;
#5752 = LINE('',#41248,#8224) ;
#5753 = LINE('',#41251,#8225) ;
#5754 = LINE('',#41253,#8226) ;
#5755 = LINE('',#41254,#8227) ;
#5756 = LINE('',#41257,#8228) ;
#5757 = LINE('',#41259,#8229) ;
#5758 = LINE('',#41260,#8230) ;
#5759 = LINE('',#41263,#8231) ;
#5760 = LINE('',#41264,#8232) ;
#5761 = LINE('',#41268,#8233) ;
#5762 = LINE('',#41271,#8234) ;
#5763 = LINE('',#41272,#8235) ;
#5764 = LINE('',#41275,#8236) ;
#5765 = LINE('',#41276,#8237) ;
#5766 = LINE('',#41277,#8238) ;
#5767 = LINE('',#41283,#8239) ;
#5768 = LINE('',#41287,#8240) ;
#5769 = LINE('',#41291,#8241) ;
#5770 = LINE('',#41298,#8242) ;
#5771 = LINE('',#41302,#8243) ;
#5772 = LINE('',#41304,#8244) ;
#5773 = LINE('',#41306,#8245) ;
#5774 = LINE('',#41308,#8246) ;
#5775 = LINE('',#41310,#8247) ;
#5776 = LINE('',#41312,#8248) ;
#5777 = LINE('',#41313,#8249) ;
#5778 = LINE('',#41316,#8250) ;
#5779 = LINE('',#41318,#8251) ;
#5780 = LINE('',#41319,#8252) ;
#5781 = LINE('',#41322,#8253) ;
#5782 = LINE('',#41324,#8254) ;
#5783 = LINE('',#41325,#8255) ;
#5784 = LINE('',#41328,#8256) ;
#5785 = LINE('',#41329,#8257) ;
#5786 = LINE('',#41331,#8258) ;
#5787 = LINE('',#41334,#8259) ;
#5788 = LINE('',#41335,#8260) ;
#5789 = LINE('',#41337,#8261) ;
#5790 = LINE('',#41338,#8262) ;
#5791 = LINE('',#41345,#8263) ;
#5792 = LINE('',#41347,#8264) ;
#5793 = LINE('',#41348,#8265) ;
#5794 = LINE('',#41355,#8266) ;
#5795 = LINE('',#41356,#8267) ;
#5796 = LINE('',#41363,#8268) ;
#5797 = LINE('',#41364,#8269) ;
#5798 = LINE('',#41372,#8270) ;
#5799 = LINE('',#41374,#8271) ;
#5800 = LINE('',#41375,#8272) ;
#5801 = LINE('',#41378,#8273) ;
#5802 = LINE('',#41383,#8274) ;
#5803 = LINE('',#41384,#8275) ;
#5804 = LINE('',#41389,#8276) ;
#5805 = LINE('',#41390,#8277) ;
#5806 = LINE('',#41395,#8278) ;
#5807 = LINE('',#41403,#8279) ;
#5808 = LINE('',#41405,#8280) ;
#5809 = LINE('',#41406,#8281) ;
#5810 = LINE('',#41413,#8282) ;
#5811 = LINE('',#41414,#8283) ;
#5812 = LINE('',#41421,#8284) ;
#5813 = LINE('',#41422,#8285) ;
#5814 = LINE('',#41430,#8286) ;
#5815 = LINE('',#41432,#8287) ;
#5816 = LINE('',#41433,#8288) ;
#5817 = LINE('',#41436,#8289) ;
#5818 = LINE('',#41441,#8290) ;
#5819 = LINE('',#41442,#8291) ;
#5820 = LINE('',#41447,#8292) ;
#5821 = LINE('',#41448,#8293) ;
#5822 = LINE('',#41453,#8294) ;
#5823 = LINE('',#41461,#8295) ;
#5824 = LINE('',#41463,#8296) ;
#5825 = LINE('',#41464,#8297) ;
#5826 = LINE('',#41471,#8298) ;
#5827 = LINE('',#41472,#8299) ;
#5828 = LINE('',#41479,#8300) ;
#5829 = LINE('',#41480,#8301) ;
#5830 = LINE('',#41488,#8302) ;
#5831 = LINE('',#41490,#8303) ;
#5832 = LINE('',#41491,#8304) ;
#5833 = LINE('',#41494,#8305) ;
#5834 = LINE('',#41499,#8306) ;
#5835 = LINE('',#41500,#8307) ;
#5836 = LINE('',#41505,#8308) ;
#5837 = LINE('',#41506,#8309) ;
#5838 = LINE('',#41511,#8310) ;
#5839 = LINE('',#41519,#8311) ;
#5840 = LINE('',#41521,#8312) ;
#5841 = LINE('',#41522,#8313) ;
#5842 = LINE('',#41529,#8314) ;
#5843 = LINE('',#41530,#8315) ;
#5844 = LINE('',#41537,#8316) ;
#5845 = LINE('',#41538,#8317) ;
#5846 = LINE('',#41546,#8318) ;
#5847 = LINE('',#41548,#8319) ;
#5848 = LINE('',#41549,#8320) ;
#5849 = LINE('',#41552,#8321) ;
#5850 = LINE('',#41557,#8322) ;
#5851 = LINE('',#41558,#8323) ;
#5852 = LINE('',#41563,#8324) ;
#5853 = LINE('',#41564,#8325) ;
#5854 = LINE('',#41569,#8326) ;
#5855 = LINE('',#41576,#8327) ;
#5856 = LINE('',#41582,#8328) ;
#5857 = LINE('',#41589,#8329) ;
#5858 = LINE('',#41592,#8330) ;
#5859 = LINE('',#41599,#8331) ;
#5860 = LINE('',#41601,#8332) ;
#5861 = LINE('',#41603,#8333) ;
#5862 = LINE('',#41604,#8334) ;
#5863 = LINE('',#41607,#8335) ;
#5864 = LINE('',#41609,#8336) ;
#5865 = LINE('',#41610,#8337) ;
#5866 = LINE('',#41613,#8338) ;
#5867 = LINE('',#41615,#8339) ;
#5868 = LINE('',#41616,#8340) ;
#5869 = LINE('',#41619,#8341) ;
#5870 = LINE('',#41621,#8342) ;
#5871 = LINE('',#41623,#8343) ;
#5872 = LINE('',#41625,#8344) ;
#5873 = LINE('',#41626,#8345) ;
#5874 = LINE('',#41629,#8346) ;
#5875 = LINE('',#41631,#8347) ;
#5876 = LINE('',#41633,#8348) ;
#5877 = LINE('',#41635,#8349) ;
#5878 = LINE('',#41636,#8350) ;
#5879 = LINE('',#41638,#8351) ;
#5880 = LINE('',#41639,#8352) ;
#5881 = LINE('',#41641,#8353) ;
#5882 = LINE('',#41643,#8354) ;
#5883 = LINE('',#41648,#8355) ;
#5884 = LINE('',#41656,#8356) ;
#5885 = LINE('',#41663,#8357) ;
#5886 = LINE('',#41665,#8358) ;
#5887 = LINE('',#41667,#8359) ;
#5888 = LINE('',#41668,#8360) ;
#5889 = LINE('',#41672,#8361) ;
#5890 = LINE('',#41674,#8362) ;
#5891 = LINE('',#41676,#8363) ;
#5892 = LINE('',#41677,#8364) ;
#5893 = LINE('',#41679,#8365) ;
#5894 = LINE('',#41680,#8366) ;
#5895 = LINE('',#41690,#8367) ;
#5896 = LINE('',#41692,#8368) ;
#5897 = LINE('',#41694,#8369) ;
#5898 = LINE('',#41695,#8370) ;
#5899 = LINE('',#41699,#8371) ;
#5900 = LINE('',#41701,#8372) ;
#5901 = LINE('',#41703,#8373) ;
#5902 = LINE('',#41704,#8374) ;
#5903 = LINE('',#41708,#8375) ;
#5904 = LINE('',#41710,#8376) ;
#5905 = LINE('',#41712,#8377) ;
#5906 = LINE('',#41713,#8378) ;
#5907 = LINE('',#41717,#8379) ;
#5908 = LINE('',#41719,#8380) ;
#5909 = LINE('',#41721,#8381) ;
#5910 = LINE('',#41722,#8382) ;
#5911 = LINE('',#41726,#8383) ;
#5912 = LINE('',#41728,#8384) ;
#5913 = LINE('',#41730,#8385) ;
#5914 = LINE('',#41731,#8386) ;
#5915 = LINE('',#41735,#8387) ;
#5916 = LINE('',#41737,#8388) ;
#5917 = LINE('',#41739,#8389) ;
#5918 = LINE('',#41740,#8390) ;
#5919 = LINE('',#41744,#8391) ;
#5920 = LINE('',#41746,#8392) ;
#5921 = LINE('',#41748,#8393) ;
#5922 = LINE('',#41749,#8394) ;
#5923 = LINE('',#41753,#8395) ;
#5924 = LINE('',#41755,#8396) ;
#5925 = LINE('',#41757,#8397) ;
#5926 = LINE('',#41758,#8398) ;
#5927 = LINE('',#41762,#8399) ;
#5928 = LINE('',#41764,#8400) ;
#5929 = LINE('',#41766,#8401) ;
#5930 = LINE('',#41767,#8402) ;
#5931 = LINE('',#41771,#8403) ;
#5932 = LINE('',#41773,#8404) ;
#5933 = LINE('',#41775,#8405) ;
#5934 = LINE('',#41776,#8406) ;
#5935 = LINE('',#41780,#8407) ;
#5936 = LINE('',#41782,#8408) ;
#5937 = LINE('',#41784,#8409) ;
#5938 = LINE('',#41785,#8410) ;
#5939 = LINE('',#41789,#8411) ;
#5940 = LINE('',#41791,#8412) ;
#5941 = LINE('',#41793,#8413) ;
#5942 = LINE('',#41794,#8414) ;
#5943 = LINE('',#41798,#8415) ;
#5944 = LINE('',#41799,#8416) ;
#5945 = LINE('',#41800,#8417) ;
#5946 = LINE('',#41804,#8418) ;
#5947 = LINE('',#41805,#8419) ;
#5948 = LINE('',#41806,#8420) ;
#5949 = LINE('',#41811,#8421) ;
#5950 = LINE('',#41817,#8422) ;
#5951 = LINE('',#41823,#8423) ;
#5952 = LINE('',#41827,#8424) ;
#5953 = LINE('',#41829,#8425) ;
#5954 = LINE('',#41830,#8426) ;
#5955 = LINE('',#41833,#8427) ;
#5956 = LINE('',#41835,#8428) ;
#5957 = LINE('',#41836,#8429) ;
#5958 = LINE('',#41839,#8430) ;
#5959 = LINE('',#41841,#8431) ;
#5960 = LINE('',#41842,#8432) ;
#5961 = LINE('',#41845,#8433) ;
#5962 = LINE('',#41847,#8434) ;
#5963 = LINE('',#41848,#8435) ;
#5964 = LINE('',#41851,#8436) ;
#5965 = LINE('',#41853,#8437) ;
#5966 = LINE('',#41854,#8438) ;
#5967 = LINE('',#41857,#8439) ;
#5968 = LINE('',#41859,#8440) ;
#5969 = LINE('',#41860,#8441) ;
#5970 = LINE('',#41863,#8442) ;
#5971 = LINE('',#41865,#8443) ;
#5972 = LINE('',#41866,#8444) ;
#5973 = LINE('',#41869,#8445) ;
#5974 = LINE('',#41871,#8446) ;
#5975 = LINE('',#41872,#8447) ;
#5976 = LINE('',#41875,#8448) ;
#5977 = LINE('',#41877,#8449) ;
#5978 = LINE('',#41881,#8450) ;
#5979 = LINE('',#41883,#8451) ;
#5980 = LINE('',#41887,#8452) ;
#5981 = LINE('',#41889,#8453) ;
#5982 = LINE('',#41893,#8454) ;
#5983 = LINE('',#41895,#8455) ;
#5984 = LINE('',#41897,#8456) ;
#5985 = LINE('',#41901,#8457) ;
#5986 = LINE('',#41903,#8458) ;
#5987 = LINE('',#41907,#8459) ;
#5988 = LINE('',#41909,#8460) ;
#5989 = LINE('',#41913,#8461) ;
#5990 = LINE('',#41915,#8462) ;
#5991 = LINE('',#41919,#8463) ;
#5992 = LINE('',#41921,#8464) ;
#5993 = LINE('',#41925,#8465) ;
#5994 = LINE('',#41927,#8466) ;
#5995 = LINE('',#41931,#8467) ;
#5996 = LINE('',#41933,#8468) ;
#5997 = LINE('',#41937,#8469) ;
#5998 = LINE('',#41939,#8470) ;
#5999 = LINE('',#41941,#8471) ;
#6000 = LINE('',#41945,#8472) ;
#6001 = LINE('',#41947,#8473) ;
#6002 = LINE('',#41951,#8474) ;
#6003 = LINE('',#41953,#8475) ;
#6004 = LINE('',#41957,#8476) ;
#6005 = LINE('',#41959,#8477) ;
#6006 = LINE('',#41963,#8478) ;
#6007 = LINE('',#41965,#8479) ;
#6008 = LINE('',#41969,#8480) ;
#6009 = LINE('',#41971,#8481) ;
#6010 = LINE('',#41975,#8482) ;
#6011 = LINE('',#41977,#8483) ;
#6012 = LINE('',#41981,#8484) ;
#6013 = LINE('',#41983,#8485) ;
#6014 = LINE('',#41985,#8486) ;
#6015 = LINE('',#41989,#8487) ;
#6016 = LINE('',#41991,#8488) ;
#6017 = LINE('',#41995,#8489) ;
#6018 = LINE('',#41997,#8490) ;
#6019 = LINE('',#42001,#8491) ;
#6020 = LINE('',#42003,#8492) ;
#6021 = LINE('',#42008,#8493) ;
#6022 = LINE('',#42010,#8494) ;
#6023 = LINE('',#42014,#8495) ;
#6024 = LINE('',#42016,#8496) ;
#6025 = LINE('',#42020,#8497) ;
#6026 = LINE('',#42022,#8498) ;
#6027 = LINE('',#42024,#8499) ;
#6028 = LINE('',#42028,#8500) ;
#6029 = LINE('',#42030,#8501) ;
#6030 = LINE('',#42034,#8502) ;
#6031 = LINE('',#42035,#8503) ;
#6032 = LINE('',#42036,#8504) ;
#6033 = LINE('',#42039,#8505) ;
#6034 = LINE('',#42042,#8506) ;
#6035 = LINE('',#42045,#8507) ;
#6036 = LINE('',#42046,#8508) ;
#6037 = LINE('',#42048,#8509) ;
#6038 = LINE('',#42049,#8510) ;
#6039 = LINE('',#42051,#8511) ;
#6040 = LINE('',#42052,#8512) ;
#6041 = LINE('',#42054,#8513) ;
#6042 = LINE('',#42055,#8514) ;
#6043 = LINE('',#42057,#8515) ;
#6044 = LINE('',#42059,#8516) ;
#6045 = LINE('',#42063,#8517) ;
#6046 = LINE('',#42066,#8518) ;
#6047 = LINE('',#42069,#8519) ;
#6048 = LINE('',#42071,#8520) ;
#6049 = LINE('',#42073,#8521) ;
#6050 = LINE('',#42074,#8522) ;
#6051 = LINE('',#42077,#8523) ;
#6052 = LINE('',#42079,#8524) ;
#6053 = LINE('',#42081,#8525) ;
#6054 = LINE('',#42082,#8526) ;
#6055 = LINE('',#42085,#8527) ;
#6056 = LINE('',#42087,#8528) ;
#6057 = LINE('',#42089,#8529) ;
#6058 = LINE('',#42090,#8530) ;
#6059 = LINE('',#42093,#8531) ;
#6060 = LINE('',#42095,#8532) ;
#6061 = LINE('',#42097,#8533) ;
#6062 = LINE('',#42098,#8534) ;
#6063 = LINE('',#42101,#8535) ;
#6064 = LINE('',#42103,#8536) ;
#6065 = LINE('',#42106,#8537) ;
#6066 = LINE('',#42109,#8538) ;
#6067 = LINE('',#42111,#8539) ;
#6068 = LINE('',#42114,#8540) ;
#6069 = LINE('',#42117,#8541) ;
#6070 = LINE('',#42119,#8542) ;
#6071 = LINE('',#42121,#8543) ;
#6072 = LINE('',#42124,#8544) ;
#6073 = LINE('',#42127,#8545) ;
#6074 = LINE('',#42130,#8546) ;
#6075 = LINE('',#42135,#8547) ;
#6076 = LINE('',#42137,#8548) ;
#6077 = LINE('',#42138,#8549) ;
#6078 = LINE('',#42141,#8550) ;
#6079 = LINE('',#42143,#8551) ;
#6080 = LINE('',#42145,#8552) ;
#6081 = LINE('',#42146,#8553) ;
#6082 = LINE('',#42149,#8554) ;
#6083 = LINE('',#42151,#8555) ;
#6084 = LINE('',#42153,#8556) ;
#6085 = LINE('',#42154,#8557) ;
#6086 = LINE('',#42157,#8558) ;
#6087 = LINE('',#42159,#8559) ;
#6088 = LINE('',#42161,#8560) ;
#6089 = LINE('',#42162,#8561) ;
#6090 = LINE('',#42165,#8562) ;
#6091 = LINE('',#42167,#8563) ;
#6092 = LINE('',#42169,#8564) ;
#6093 = LINE('',#42170,#8565) ;
#6094 = LINE('',#42173,#8566) ;
#6095 = LINE('',#42175,#8567) ;
#6096 = LINE('',#42177,#8568) ;
#6097 = LINE('',#42178,#8569) ;
#6098 = LINE('',#42181,#8570) ;
#6099 = LINE('',#42183,#8571) ;
#6100 = LINE('',#42186,#8572) ;
#6101 = LINE('',#42189,#8573) ;
#6102 = LINE('',#42191,#8574) ;
#6103 = LINE('',#42193,#8575) ;
#6104 = LINE('',#42194,#8576) ;
#6105 = LINE('',#42197,#8577) ;
#6106 = LINE('',#42199,#8578) ;
#6107 = LINE('',#42201,#8579) ;
#6108 = LINE('',#42202,#8580) ;
#6109 = LINE('',#42205,#8581) ;
#6110 = LINE('',#42208,#8582) ;
#6111 = LINE('',#42211,#8583) ;
#6112 = LINE('',#42213,#8584) ;
#6113 = LINE('',#42217,#8585) ;
#6114 = LINE('',#42218,#8586) ;
#6115 = LINE('',#42221,#8587) ;
#6116 = LINE('',#42224,#8588) ;
#6117 = LINE('',#42227,#8589) ;
#6118 = LINE('',#42229,#8590) ;
#6119 = LINE('',#42231,#8591) ;
#6120 = LINE('',#42232,#8592) ;
#6121 = LINE('',#42235,#8593) ;
#6122 = LINE('',#42238,#8594) ;
#6123 = LINE('',#42241,#8595) ;
#6124 = LINE('',#42243,#8596) ;
#6125 = LINE('',#42246,#8597) ;
#6126 = LINE('',#42249,#8598) ;
#6127 = LINE('',#42251,#8599) ;
#6128 = LINE('',#42253,#8600) ;
#6129 = LINE('',#42254,#8601) ;
#6130 = LINE('',#42257,#8602) ;
#6131 = LINE('',#42259,#8603) ;
#6132 = LINE('',#42261,#8604) ;
#6133 = LINE('',#42262,#8605) ;
#6134 = LINE('',#42265,#8606) ;
#6135 = LINE('',#42267,#8607) ;
#6136 = LINE('',#42269,#8608) ;
#6137 = LINE('',#42270,#8609) ;
#6138 = LINE('',#42273,#8610) ;
#6139 = LINE('',#42275,#8611) ;
#6140 = LINE('',#42277,#8612) ;
#6141 = LINE('',#42278,#8613) ;
#6142 = LINE('',#42281,#8614) ;
#6143 = LINE('',#42283,#8615) ;
#6144 = LINE('',#42285,#8616) ;
#6145 = LINE('',#42286,#8617) ;
#6146 = LINE('',#42289,#8618) ;
#6147 = LINE('',#42291,#8619) ;
#6148 = LINE('',#42293,#8620) ;
#6149 = LINE('',#42294,#8621) ;
#6150 = LINE('',#42297,#8622) ;
#6151 = LINE('',#42299,#8623) ;
#6152 = LINE('',#42303,#8624) ;
#6153 = LINE('',#42305,#8625) ;
#6154 = LINE('',#42307,#8626) ;
#6155 = LINE('',#42308,#8627) ;
#6156 = LINE('',#42313,#8628) ;
#6157 = LINE('',#42315,#8629) ;
#6158 = LINE('',#42316,#8630) ;
#6159 = LINE('',#42319,#8631) ;
#6160 = LINE('',#42321,#8632) ;
#6161 = LINE('',#42323,#8633) ;
#6162 = LINE('',#42324,#8634) ;
#6163 = LINE('',#42327,#8635) ;
#6164 = LINE('',#42329,#8636) ;
#6165 = LINE('',#42331,#8637) ;
#6166 = LINE('',#42332,#8638) ;
#6167 = LINE('',#42335,#8639) ;
#6168 = LINE('',#42337,#8640) ;
#6169 = LINE('',#42339,#8641) ;
#6170 = LINE('',#42340,#8642) ;
#6171 = LINE('',#42343,#8643) ;
#6172 = LINE('',#42345,#8644) ;
#6173 = LINE('',#42347,#8645) ;
#6174 = LINE('',#42348,#8646) ;
#6175 = LINE('',#42351,#8647) ;
#6176 = LINE('',#42353,#8648) ;
#6177 = LINE('',#42355,#8649) ;
#6178 = LINE('',#42356,#8650) ;
#6179 = LINE('',#42359,#8651) ;
#6180 = LINE('',#42361,#8652) ;
#6181 = LINE('',#42363,#8653) ;
#6182 = LINE('',#42364,#8654) ;
#6183 = LINE('',#42367,#8655) ;
#6184 = LINE('',#42369,#8656) ;
#6185 = LINE('',#42371,#8657) ;
#6186 = LINE('',#42372,#8658) ;
#6187 = LINE('',#42375,#8659) ;
#6188 = LINE('',#42377,#8660) ;
#6189 = LINE('',#42379,#8661) ;
#6190 = LINE('',#42380,#8662) ;
#6191 = LINE('',#42383,#8663) ;
#6192 = LINE('',#42385,#8664) ;
#6193 = LINE('',#42387,#8665) ;
#6194 = LINE('',#42388,#8666) ;
#6195 = LINE('',#42392,#8667) ;
#6196 = LINE('',#42394,#8668) ;
#6197 = LINE('',#42395,#8669) ;
#6198 = LINE('',#42399,#8670) ;
#6199 = LINE('',#42402,#8671) ;
#6200 = LINE('',#42404,#8672) ;
#6201 = LINE('',#42408,#8673) ;
#6202 = LINE('',#42410,#8674) ;
#6203 = LINE('',#42414,#8675) ;
#6204 = LINE('',#42416,#8676) ;
#6205 = LINE('',#42418,#8677) ;
#6206 = LINE('',#42422,#8678) ;
#6207 = LINE('',#42424,#8679) ;
#6208 = LINE('',#42428,#8680) ;
#6209 = LINE('',#42430,#8681) ;
#6210 = LINE('',#42435,#8682) ;
#6211 = LINE('',#42437,#8683) ;
#6212 = LINE('',#42441,#8684) ;
#6213 = LINE('',#42443,#8685) ;
#6214 = LINE('',#42447,#8686) ;
#6215 = LINE('',#42449,#8687) ;
#6216 = LINE('',#42453,#8688) ;
#6217 = LINE('',#42455,#8689) ;
#6218 = LINE('',#42457,#8690) ;
#6219 = LINE('',#42461,#8691) ;
#6220 = LINE('',#42463,#8692) ;
#6221 = LINE('',#42467,#8693) ;
#6222 = LINE('',#42469,#8694) ;
#6223 = LINE('',#42473,#8695) ;
#6224 = LINE('',#42475,#8696) ;
#6225 = LINE('',#42479,#8697) ;
#6226 = LINE('',#42481,#8698) ;
#6227 = LINE('',#42485,#8699) ;
#6228 = LINE('',#42487,#8700) ;
#6229 = LINE('',#42491,#8701) ;
#6230 = LINE('',#42493,#8702) ;
#6231 = LINE('',#42497,#8703) ;
#6232 = LINE('',#42499,#8704) ;
#6233 = LINE('',#42501,#8705) ;
#6234 = LINE('',#42505,#8706) ;
#6235 = LINE('',#42507,#8707) ;
#6236 = LINE('',#42511,#8708) ;
#6237 = LINE('',#42513,#8709) ;
#6238 = LINE('',#42517,#8710) ;
#6239 = LINE('',#42519,#8711) ;
#6240 = LINE('',#42523,#8712) ;
#6241 = LINE('',#42525,#8713) ;
#6242 = LINE('',#42529,#8714) ;
#6243 = LINE('',#42531,#8715) ;
#6244 = LINE('',#42535,#8716) ;
#6245 = LINE('',#42537,#8717) ;
#6246 = LINE('',#42541,#8718) ;
#6247 = LINE('',#42543,#8719) ;
#6248 = LINE('',#42545,#8720) ;
#6249 = LINE('',#42549,#8721) ;
#6250 = LINE('',#42551,#8722) ;
#6251 = LINE('',#42555,#8723) ;
#6252 = LINE('',#42557,#8724) ;
#6253 = LINE('',#42561,#8725) ;
#6254 = LINE('',#42562,#8726) ;
#6255 = LINE('',#42564,#8727) ;
#6256 = LINE('',#42565,#8728) ;
#6257 = LINE('',#42567,#8729) ;
#6258 = LINE('',#42568,#8730) ;
#6259 = LINE('',#42570,#8731) ;
#6260 = LINE('',#42571,#8732) ;
#6261 = LINE('',#42573,#8733) ;
#6262 = LINE('',#42574,#8734) ;
#6263 = LINE('',#42578,#8735) ;
#6264 = LINE('',#42579,#8736) ;
#6265 = LINE('',#42581,#8737) ;
#6266 = LINE('',#42584,#8738) ;
#6267 = LINE('',#42588,#8739) ;
#6268 = LINE('',#42590,#8740) ;
#6269 = LINE('',#42591,#8741) ;
#6270 = LINE('',#42592,#8742) ;
#6271 = LINE('',#42595,#8743) ;
#6272 = LINE('',#42599,#8744) ;
#6273 = LINE('',#42601,#8745) ;
#6274 = LINE('',#42602,#8746) ;
#6275 = LINE('',#42605,#8747) ;
#6276 = LINE('',#42607,#8748) ;
#6277 = LINE('',#42609,#8749) ;
#6278 = LINE('',#42610,#8750) ;
#6279 = LINE('',#42613,#8751) ;
#6280 = LINE('',#42615,#8752) ;
#6281 = LINE('',#42617,#8753) ;
#6282 = LINE('',#42618,#8754) ;
#6283 = LINE('',#42621,#8755) ;
#6284 = LINE('',#42623,#8756) ;
#6285 = LINE('',#42625,#8757) ;
#6286 = LINE('',#42626,#8758) ;
#6287 = LINE('',#42629,#8759) ;
#6288 = LINE('',#42631,#8760) ;
#6289 = LINE('',#42633,#8761) ;
#6290 = LINE('',#42634,#8762) ;
#6291 = LINE('',#42637,#8763) ;
#6292 = LINE('',#42640,#8764) ;
#6293 = LINE('',#42643,#8765) ;
#6294 = LINE('',#42645,#8766) ;
#6295 = LINE('',#42647,#8767) ;
#6296 = LINE('',#42648,#8768) ;
#6297 = LINE('',#42651,#8769) ;
#6298 = LINE('',#42653,#8770) ;
#6299 = LINE('',#42655,#8771) ;
#6300 = LINE('',#42656,#8772) ;
#6301 = LINE('',#42659,#8773) ;
#6302 = LINE('',#42661,#8774) ;
#6303 = LINE('',#42663,#8775) ;
#6304 = LINE('',#42664,#8776) ;
#6305 = LINE('',#42667,#8777) ;
#6306 = LINE('',#42669,#8778) ;
#6307 = LINE('',#42671,#8779) ;
#6308 = LINE('',#42672,#8780) ;
#6309 = LINE('',#42675,#8781) ;
#6310 = LINE('',#42677,#8782) ;
#6311 = LINE('',#42679,#8783) ;
#6312 = LINE('',#42680,#8784) ;
#6313 = LINE('',#42683,#8785) ;
#6314 = LINE('',#42685,#8786) ;
#6315 = LINE('',#42687,#8787) ;
#6316 = LINE('',#42688,#8788) ;
#6317 = LINE('',#42691,#8789) ;
#6318 = LINE('',#42693,#8790) ;
#6319 = LINE('',#42695,#8791) ;
#6320 = LINE('',#42699,#8792) ;
#6321 = LINE('',#42703,#8793) ;
#6322 = LINE('',#42704,#8794) ;
#6323 = LINE('',#42707,#8795) ;
#6324 = LINE('',#42709,#8796) ;
#6325 = LINE('',#42713,#8797) ;
#6326 = LINE('',#42714,#8798) ;
#6327 = LINE('',#42717,#8799) ;
#6328 = LINE('',#42720,#8800) ;
#6329 = LINE('',#42723,#8801) ;
#6330 = LINE('',#42725,#8802) ;
#6331 = LINE('',#42727,#8803) ;
#6332 = LINE('',#42728,#8804) ;
#6333 = LINE('',#42731,#8805) ;
#6334 = LINE('',#42734,#8806) ;
#6335 = LINE('',#42737,#8807) ;
#6336 = LINE('',#42739,#8808) ;
#6337 = LINE('',#42741,#8809) ;
#6338 = LINE('',#42742,#8810) ;
#6339 = LINE('',#42745,#8811) ;
#6340 = LINE('',#42747,#8812) ;
#6341 = LINE('',#42749,#8813) ;
#6342 = LINE('',#42750,#8814) ;
#6343 = LINE('',#42753,#8815) ;
#6344 = LINE('',#42755,#8816) ;
#6345 = LINE('',#42757,#8817) ;
#6346 = LINE('',#42758,#8818) ;
#6347 = LINE('',#42761,#8819) ;
#6348 = LINE('',#42763,#8820) ;
#6349 = LINE('',#42765,#8821) ;
#6350 = LINE('',#42766,#8822) ;
#6351 = LINE('',#42769,#8823) ;
#6352 = LINE('',#42773,#8824) ;
#6353 = LINE('',#42774,#8825) ;
#6354 = LINE('',#42777,#8826) ;
#6355 = LINE('',#42779,#8827) ;
#6356 = LINE('',#42781,#8828) ;
#6357 = LINE('',#42785,#8829) ;
#6358 = LINE('',#42787,#8830) ;
#6359 = LINE('',#42789,#8831) ;
#6360 = LINE('',#42790,#8832) ;
#6361 = LINE('',#42793,#8833) ;
#6362 = LINE('',#42795,#8834) ;
#6363 = LINE('',#42797,#8835) ;
#6364 = LINE('',#42798,#8836) ;
#6365 = LINE('',#42801,#8837) ;
#6366 = LINE('',#42803,#8838) ;
#6367 = LINE('',#42805,#8839) ;
#6368 = LINE('',#42806,#8840) ;
#6369 = LINE('',#42811,#8841) ;
#6370 = LINE('',#42812,#8842) ;
#6371 = LINE('',#42815,#8843) ;
#6372 = LINE('',#42817,#8844) ;
#6373 = LINE('',#42819,#8845) ;
#6374 = LINE('',#42820,#8846) ;
#6375 = LINE('',#42823,#8847) ;
#6376 = LINE('',#42825,#8848) ;
#6377 = LINE('',#42827,#8849) ;
#6378 = LINE('',#42828,#8850) ;
#6379 = LINE('',#42831,#8851) ;
#6380 = LINE('',#42833,#8852) ;
#6381 = LINE('',#42835,#8853) ;
#6382 = LINE('',#42836,#8854) ;
#6383 = LINE('',#42839,#8855) ;
#6384 = LINE('',#42841,#8856) ;
#6385 = LINE('',#42843,#8857) ;
#6386 = LINE('',#42844,#8858) ;
#6387 = LINE('',#42847,#8859) ;
#6388 = LINE('',#42849,#8860) ;
#6389 = LINE('',#42851,#8861) ;
#6390 = LINE('',#42852,#8862) ;
#6391 = LINE('',#42855,#8863) ;
#6392 = LINE('',#42857,#8864) ;
#6393 = LINE('',#42859,#8865) ;
#6394 = LINE('',#42860,#8866) ;
#6395 = LINE('',#42863,#8867) ;
#6396 = LINE('',#42865,#8868) ;
#6397 = LINE('',#42867,#8869) ;
#6398 = LINE('',#42868,#8870) ;
#6399 = LINE('',#42871,#8871) ;
#6400 = LINE('',#42873,#8872) ;
#6401 = LINE('',#42875,#8873) ;
#6402 = LINE('',#42876,#8874) ;
#6403 = LINE('',#42879,#8875) ;
#6404 = LINE('',#42881,#8876) ;
#6405 = LINE('',#42883,#8877) ;
#6406 = LINE('',#42884,#8878) ;
#6407 = LINE('',#42887,#8879) ;
#6408 = LINE('',#42890,#8880) ;
#6409 = LINE('',#42893,#8881) ;
#6410 = LINE('',#42896,#8882) ;
#6411 = LINE('',#42899,#8883) ;
#6412 = LINE('',#42903,#8884) ;
#6413 = LINE('',#42904,#8885) ;
#6414 = LINE('',#42907,#8886) ;
#6415 = LINE('',#42911,#8887) ;
#6416 = LINE('',#42912,#8888) ;
#6417 = LINE('',#42915,#8889) ;
#6418 = LINE('',#42917,#8890) ;
#6419 = LINE('',#42919,#8891) ;
#6420 = LINE('',#42920,#8892) ;
#6421 = LINE('',#42922,#8893) ;
#6422 = LINE('',#42924,#8894) ;
#6423 = LINE('',#42926,#8895) ;
#6424 = LINE('',#42928,#8896) ;
#6425 = LINE('',#42929,#8897) ;
#6426 = LINE('',#42931,#8898) ;
#6427 = LINE('',#42932,#8899) ;
#6428 = LINE('',#42934,#8900) ;
#6429 = LINE('',#42935,#8901) ;
#6430 = LINE('',#42937,#8902) ;
#6431 = LINE('',#42938,#8903) ;
#6432 = LINE('',#42940,#8904) ;
#6433 = LINE('',#42941,#8905) ;
#6434 = LINE('',#42943,#8906) ;
#6435 = LINE('',#42944,#8907) ;
#6436 = LINE('',#42946,#8908) ;
#6437 = LINE('',#42947,#8909) ;
#6438 = LINE('',#42949,#8910) ;
#6439 = LINE('',#42950,#8911) ;
#6440 = LINE('',#42952,#8912) ;
#6441 = LINE('',#42953,#8913) ;
#6442 = LINE('',#42955,#8914) ;
#6443 = LINE('',#42956,#8915) ;
#6444 = LINE('',#42958,#8916) ;
#6445 = LINE('',#42960,#8917) ;
#6446 = LINE('',#42962,#8918) ;
#6447 = LINE('',#42963,#8919) ;
#6448 = LINE('',#42965,#8920) ;
#6449 = LINE('',#42967,#8921) ;
#6450 = LINE('',#42969,#8922) ;
#6451 = LINE('',#42972,#8923) ;
#6452 = LINE('',#42974,#8924) ;
#6453 = LINE('',#42976,#8925) ;
#6454 = LINE('',#42978,#8926) ;
#6455 = LINE('',#42980,#8927) ;
#6456 = LINE('',#42982,#8928) ;
#6457 = LINE('',#42984,#8929) ;
#6458 = LINE('',#42986,#8930) ;
#6459 = LINE('',#42988,#8931) ;
#6460 = LINE('',#42990,#8932) ;
#6461 = LINE('',#42991,#8933) ;
#6462 = LINE('',#42993,#8934) ;
#6463 = LINE('',#42995,#8935) ;
#6464 = LINE('',#42997,#8936) ;
#6465 = LINE('',#42998,#8937) ;
#6466 = LINE('',#43000,#8938) ;
#6467 = LINE('',#43002,#8939) ;
#6468 = LINE('',#43004,#8940) ;
#6469 = LINE('',#43007,#8941) ;
#6470 = LINE('',#43008,#8942) ;
#6471 = LINE('',#43010,#8943) ;
#6472 = LINE('',#43011,#8944) ;
#6473 = LINE('',#43013,#8945) ;
#6474 = LINE('',#43014,#8946) ;
#6475 = LINE('',#43016,#8947) ;
#6476 = LINE('',#43017,#8948) ;
#6477 = LINE('',#43019,#8949) ;
#6478 = LINE('',#43020,#8950) ;
#6479 = LINE('',#43022,#8951) ;
#6480 = LINE('',#43024,#8952) ;
#6481 = LINE('',#43027,#8953) ;
#6482 = LINE('',#43029,#8954) ;
#6483 = LINE('',#43032,#8955) ;
#6484 = LINE('',#43035,#8956) ;
#6485 = LINE('',#43038,#8957) ;
#6486 = LINE('',#43041,#8958) ;
#6487 = LINE('',#43043,#8959) ;
#6488 = LINE('',#43045,#8960) ;
#6489 = LINE('',#43047,#8961) ;
#6490 = LINE('',#43048,#8962) ;
#6491 = LINE('',#43050,#8963) ;
#6492 = LINE('',#43051,#8964) ;
#6493 = LINE('',#43053,#8965) ;
#6494 = LINE('',#43055,#8966) ;
#6495 = LINE('',#43057,#8967) ;
#6496 = LINE('',#43060,#8968) ;
#6497 = LINE('',#43062,#8969) ;
#6498 = LINE('',#43063,#8970) ;
#6499 = LINE('',#43065,#8971) ;
#6500 = LINE('',#43066,#8972) ;
#6501 = LINE('',#43068,#8973) ;
#6502 = LINE('',#43070,#8974) ;
#6503 = LINE('',#43071,#8975) ;
#6504 = LINE('',#43073,#8976) ;
#6505 = LINE('',#43074,#8977) ;
#6506 = LINE('',#43076,#8978) ;
#6507 = LINE('',#43079,#8979) ;
#6508 = LINE('',#43081,#8980) ;
#6509 = LINE('',#43084,#8981) ;
#6510 = LINE('',#43087,#8982) ;
#6511 = LINE('',#43089,#8983) ;
#6512 = LINE('',#43091,#8984) ;
#6513 = LINE('',#43093,#8985) ;
#6514 = LINE('',#43096,#8986) ;
#6515 = LINE('',#43099,#8987) ;
#6516 = LINE('',#43101,#8988) ;
#6517 = LINE('',#43102,#8989) ;
#6518 = LINE('',#43104,#8990) ;
#6519 = LINE('',#43106,#8991) ;
#6520 = LINE('',#43107,#8992) ;
#6521 = LINE('',#43109,#8993) ;
#6522 = LINE('',#43111,#8994) ;
#6523 = LINE('',#43113,#8995) ;
#6524 = LINE('',#43115,#8996) ;
#6525 = LINE('',#43118,#8997) ;
#6526 = LINE('',#43119,#8998) ;
#6527 = LINE('',#43121,#8999) ;
#6528 = LINE('',#43122,#9000) ;
#6529 = LINE('',#43124,#9001) ;
#6530 = LINE('',#43125,#9002) ;
#6531 = LINE('',#43127,#9003) ;
#6532 = LINE('',#43128,#9004) ;
#6533 = LINE('',#43130,#9005) ;
#6534 = LINE('',#43131,#9006) ;
#6535 = LINE('',#43133,#9007) ;
#6536 = LINE('',#43135,#9008) ;
#6537 = LINE('',#43139,#9009) ;
#6538 = LINE('',#43141,#9010) ;
#6539 = LINE('',#43144,#9011) ;
#6540 = LINE('',#43146,#9012) ;
#6541 = LINE('',#43149,#9013) ;
#6542 = LINE('',#43152,#9014) ;
#6543 = LINE('',#43155,#9015) ;
#6544 = LINE('',#43158,#9016) ;
#6545 = LINE('',#43160,#9017) ;
#6546 = LINE('',#43161,#9018) ;
#6547 = LINE('',#43163,#9019) ;
#6548 = LINE('',#43164,#9020) ;
#6549 = LINE('',#43166,#9021) ;
#6550 = LINE('',#43167,#9022) ;
#6551 = LINE('',#43169,#9023) ;
#6552 = LINE('',#43170,#9024) ;
#6553 = LINE('',#43172,#9025) ;
#6554 = LINE('',#43174,#9026) ;
#6555 = LINE('',#43175,#9027) ;
#6556 = LINE('',#43177,#9028) ;
#6557 = LINE('',#43179,#9029) ;
#6558 = LINE('',#43180,#9030) ;
#6559 = LINE('',#43182,#9031) ;
#6560 = LINE('',#43184,#9032) ;
#6561 = LINE('',#43186,#9033) ;
#6562 = LINE('',#43189,#9034) ;
#6563 = LINE('',#43192,#9035) ;
#6564 = LINE('',#43194,#9036) ;
#6565 = LINE('',#43197,#9037) ;
#6566 = LINE('',#43199,#9038) ;
#6567 = LINE('',#43202,#9039) ;
#6568 = LINE('',#43205,#9040) ;
#6569 = LINE('',#43208,#9041) ;
#6570 = LINE('',#43210,#9042) ;
#6571 = LINE('',#43212,#9043) ;
#6572 = LINE('',#43214,#9044) ;
#6573 = LINE('',#43216,#9045) ;
#6574 = LINE('',#43218,#9046) ;
#6575 = LINE('',#43220,#9047) ;
#6576 = LINE('',#43221,#9048) ;
#6577 = LINE('',#43223,#9049) ;
#6578 = LINE('',#43226,#9050) ;
#6579 = LINE('',#43228,#9051) ;
#6580 = LINE('',#43229,#9052) ;
#6581 = LINE('',#43231,#9053) ;
#6582 = LINE('',#43232,#9054) ;
#6583 = LINE('',#43234,#9055) ;
#6584 = LINE('',#43235,#9056) ;
#6585 = LINE('',#43237,#9057) ;
#6586 = LINE('',#43238,#9058) ;
#6587 = LINE('',#43240,#9059) ;
#6588 = LINE('',#43241,#9060) ;
#6589 = LINE('',#43243,#9061) ;
#6590 = LINE('',#43244,#9062) ;
#6591 = LINE('',#43248,#9063) ;
#6592 = LINE('',#43250,#9064) ;
#6593 = LINE('',#43254,#9065) ;
#6594 = LINE('',#43257,#9066) ;
#6595 = LINE('',#43260,#9067) ;
#6596 = LINE('',#43262,#9068) ;
#6597 = LINE('',#43265,#9069) ;
#6598 = LINE('',#43268,#9070) ;
#6599 = LINE('',#43270,#9071) ;
#6600 = LINE('',#43272,#9072) ;
#6601 = LINE('',#43274,#9073) ;
#6602 = LINE('',#43276,#9074) ;
#6603 = LINE('',#43278,#9075) ;
#6604 = LINE('',#43281,#9076) ;
#6605 = LINE('',#43282,#9077) ;
#6606 = LINE('',#43284,#9078) ;
#6607 = LINE('',#43285,#9079) ;
#6608 = LINE('',#43287,#9080) ;
#6609 = LINE('',#43288,#9081) ;
#6610 = LINE('',#43290,#9082) ;
#6611 = LINE('',#43291,#9083) ;
#6612 = LINE('',#43293,#9084) ;
#6613 = LINE('',#43294,#9085) ;
#6614 = LINE('',#43298,#9086) ;
#6615 = LINE('',#43303,#9087) ;
#6616 = LINE('',#43305,#9088) ;
#6617 = LINE('',#43308,#9089) ;
#6618 = LINE('',#43310,#9090) ;
#6619 = LINE('',#43313,#9091) ;
#6620 = LINE('',#43315,#9092) ;
#6621 = LINE('',#43317,#9093) ;
#6622 = LINE('',#43318,#9094) ;
#6623 = LINE('',#43320,#9095) ;
#6624 = LINE('',#43321,#9096) ;
#6625 = LINE('',#43323,#9097) ;
#6626 = LINE('',#43324,#9098) ;
#6627 = LINE('',#43326,#9099) ;
#6628 = LINE('',#43328,#9100) ;
#6629 = LINE('',#43329,#9101) ;
#6630 = LINE('',#43332,#9102) ;
#6631 = LINE('',#43334,#9103) ;
#6632 = LINE('',#43337,#9104) ;
#6633 = LINE('',#43341,#9105) ;
#6634 = LINE('',#43344,#9106) ;
#6635 = LINE('',#43346,#9107) ;
#6636 = LINE('',#43348,#9108) ;
#6637 = LINE('',#43351,#9109) ;
#6638 = LINE('',#43353,#9110) ;
#6639 = LINE('',#43355,#9111) ;
#6640 = LINE('',#43358,#9112) ;
#6641 = LINE('',#43360,#9113) ;
#6642 = LINE('',#43362,#9114) ;
#6643 = LINE('',#43363,#9115) ;
#6644 = LINE('',#43365,#9116) ;
#6645 = LINE('',#43366,#9117) ;
#6646 = LINE('',#43368,#9118) ;
#6647 = LINE('',#43369,#9119) ;
#6648 = LINE('',#43371,#9120) ;
#6649 = LINE('',#43373,#9121) ;
#6650 = LINE('',#43376,#9122) ;
#6651 = LINE('',#43379,#9123) ;
#6652 = LINE('',#43383,#9124) ;
#6653 = LINE('',#43385,#9125) ;
#6654 = LINE('',#43388,#9126) ;
#6655 = LINE('',#43391,#9127) ;
#6656 = LINE('',#43392,#9128) ;
#6657 = LINE('',#43395,#9129) ;
#6658 = LINE('',#43396,#9130) ;
#6659 = LINE('',#43399,#9131) ;
#6660 = LINE('',#43402,#9132) ;
#6661 = LINE('',#43405,#9133) ;
#6662 = LINE('',#43407,#9134) ;
#6663 = LINE('',#43409,#9135) ;
#6664 = LINE('',#43411,#9136) ;
#6665 = LINE('',#43413,#9137) ;
#6666 = LINE('',#43415,#9138) ;
#6667 = LINE('',#43418,#9139) ;
#6668 = LINE('',#43421,#9140) ;
#6669 = LINE('',#43423,#9141) ;
#6670 = LINE('',#43427,#9142) ;
#6671 = LINE('',#43429,#9143) ;
#6672 = LINE('',#43431,#9144) ;
#6673 = LINE('',#43435,#9145) ;
#6674 = LINE('',#43437,#9146) ;
#6675 = LINE('',#43643,#9147) ;
#6676 = LINE('',#43648,#9148) ;
#6677 = LINE('',#43653,#9149) ;
#6678 = LINE('',#43658,#9150) ;
#6679 = LINE('',#43663,#9151) ;
#6680 = LINE('',#43668,#9152) ;
#6681 = LINE('',#43673,#9153) ;
#6682 = LINE('',#43677,#9154) ;
#6683 = LINE('',#43680,#9155) ;
#6684 = LINE('',#43683,#9156) ;
#6685 = LINE('',#43686,#9157) ;
#6686 = LINE('',#43689,#9158) ;
#6687 = LINE('',#43692,#9159) ;
#6688 = LINE('',#43695,#9160) ;
#6689 = LINE('',#43698,#9161) ;
#6690 = LINE('',#43701,#9162) ;
#6691 = LINE('',#43704,#9163) ;
#6692 = LINE('',#43707,#9164) ;
#6693 = LINE('',#43710,#9165) ;
#6694 = LINE('',#43713,#9166) ;
#6695 = LINE('',#43716,#9167) ;
#6696 = LINE('',#43722,#9168) ;
#6697 = LINE('',#43727,#9169) ;
#6698 = LINE('',#43732,#9170) ;
#6699 = LINE('',#43737,#9171) ;
#6700 = LINE('',#43742,#9172) ;
#6701 = LINE('',#43747,#9173) ;
#6702 = LINE('',#43751,#9174) ;
#6703 = LINE('',#43764,#9175) ;
#6704 = LINE('',#43770,#9176) ;
#6705 = LINE('',#43776,#9177) ;
#6706 = LINE('',#43782,#9178) ;
#6707 = LINE('',#43788,#9179) ;
#6708 = LINE('',#43794,#9180) ;
#6709 = LINE('',#43799,#9181) ;
#6710 = LINE('',#43803,#9182) ;
#6711 = LINE('',#43808,#9183) ;
#6712 = LINE('',#43810,#9184) ;
#6713 = LINE('',#43812,#9185) ;
#6714 = LINE('',#43813,#9186) ;
#6715 = LINE('',#43815,#9187) ;
#6716 = LINE('',#43817,#9188) ;
#6717 = LINE('',#43819,#9189) ;
#6718 = LINE('',#43820,#9190) ;
#6719 = LINE('',#43823,#9191) ;
#6720 = LINE('',#43825,#9192) ;
#6721 = LINE('',#43826,#9193) ;
#6722 = LINE('',#43828,#9194) ;
#6723 = LINE('',#43830,#9195) ;
#6724 = LINE('',#43832,#9196) ;
#6725 = LINE('',#43838,#9197) ;
#6726 = LINE('',#43844,#9198) ;
#6727 = LINE('',#43849,#9199) ;
#6728 = LINE('',#43853,#9200) ;
#6729 = LINE('',#43858,#9201) ;
#6730 = LINE('',#43860,#9202) ;
#6731 = LINE('',#43862,#9203) ;
#6732 = LINE('',#43863,#9204) ;
#6733 = LINE('',#43865,#9205) ;
#6734 = LINE('',#43867,#9206) ;
#6735 = LINE('',#43869,#9207) ;
#6736 = LINE('',#43870,#9208) ;
#6737 = LINE('',#43873,#9209) ;
#6738 = LINE('',#43875,#9210) ;
#6739 = LINE('',#43876,#9211) ;
#6740 = LINE('',#43878,#9212) ;
#6741 = LINE('',#43880,#9213) ;
#6742 = LINE('',#43882,#9214) ;
#6743 = LINE('',#43888,#9215) ;
#6744 = LINE('',#43894,#9216) ;
#6745 = LINE('',#43900,#9217) ;
#6746 = LINE('',#43906,#9218) ;
#6747 = LINE('',#43912,#9219) ;
#6748 = LINE('',#43914,#9220) ;
#6749 = LINE('',#43916,#9221) ;
#6750 = LINE('',#43918,#9222) ;
#6751 = LINE('',#43919,#9223) ;
#6752 = LINE('',#43926,#9224) ;
#6753 = LINE('',#43931,#9225) ;
#6754 = LINE('',#43937,#9226) ;
#6755 = LINE('',#43939,#9227) ;
#6756 = LINE('',#43941,#9228) ;
#6757 = LINE('',#43942,#9229) ;
#6758 = LINE('',#43945,#9230) ;
#6759 = LINE('',#43947,#9231) ;
#6760 = LINE('',#43948,#9232) ;
#6761 = LINE('',#43951,#9233) ;
#6762 = LINE('',#43953,#9234) ;
#6763 = LINE('',#43954,#9235) ;
#6764 = LINE('',#43956,#9236) ;
#6765 = LINE('',#43957,#9237) ;
#6766 = LINE('',#43961,#9238) ;
#6767 = LINE('',#43963,#9239) ;
#6768 = LINE('',#43965,#9240) ;
#6769 = LINE('',#43966,#9241) ;
#6770 = LINE('',#43969,#9242) ;
#6771 = LINE('',#43971,#9243) ;
#6772 = LINE('',#43972,#9244) ;
#6773 = LINE('',#43975,#9245) ;
#6774 = LINE('',#43977,#9246) ;
#6775 = LINE('',#43978,#9247) ;
#6776 = LINE('',#43981,#9248) ;
#6777 = LINE('',#43983,#9249) ;
#6778 = LINE('',#43985,#9250) ;
#6779 = LINE('',#43986,#9251) ;
#6780 = LINE('',#43991,#9252) ;
#6781 = LINE('',#43993,#9253) ;
#6782 = LINE('',#43995,#9254) ;
#6783 = LINE('',#43996,#9255) ;
#6784 = LINE('',#44003,#9256) ;
#6785 = LINE('',#44005,#9257) ;
#6786 = LINE('',#44007,#9258) ;
#6787 = LINE('',#44008,#9259) ;
#6788 = LINE('',#44013,#9260) ;
#6789 = LINE('',#44015,#9261) ;
#6790 = LINE('',#44017,#9262) ;
#6791 = LINE('',#44018,#9263) ;
#6792 = LINE('',#44020,#9264) ;
#6793 = LINE('',#44022,#9265) ;
#6794 = LINE('',#44023,#9266) ;
#6795 = LINE('',#44027,#9267) ;
#6796 = LINE('',#44029,#9268) ;
#6797 = LINE('',#44030,#9269) ;
#6798 = LINE('',#44032,#9270) ;
#6799 = LINE('',#44034,#9271) ;
#6800 = LINE('',#44036,#9272) ;
#6801 = LINE('',#44037,#9273) ;
#6802 = LINE('',#44039,#9274) ;
#6803 = LINE('',#44042,#9275) ;
#6804 = LINE('',#44046,#9276) ;
#6805 = LINE('',#44047,#9277) ;
#6806 = LINE('',#44050,#9278) ;
#6807 = LINE('',#44052,#9279) ;
#6808 = LINE('',#44056,#9280) ;
#6809 = LINE('',#44058,#9281) ;
#6810 = LINE('',#44059,#9282) ;
#6811 = LINE('',#44063,#9283) ;
#6812 = LINE('',#44065,#9284) ;
#6813 = LINE('',#44067,#9285) ;
#6814 = LINE('',#44068,#9286) ;
#6815 = LINE('',#44072,#9287) ;
#6816 = LINE('',#44074,#9288) ;
#6817 = LINE('',#44076,#9289) ;
#6818 = LINE('',#44077,#9290) ;
#6819 = LINE('',#44081,#9291) ;
#6820 = LINE('',#44083,#9292) ;
#6821 = LINE('',#44085,#9293) ;
#6822 = LINE('',#44086,#9294) ;
#6823 = LINE('',#44089,#9295) ;
#6824 = LINE('',#44091,#9296) ;
#6825 = LINE('',#44092,#9297) ;
#6826 = LINE('',#44096,#9298) ;
#6827 = LINE('',#44098,#9299) ;
#6828 = LINE('',#44100,#9300) ;
#6829 = LINE('',#44104,#9301) ;
#6830 = LINE('',#44106,#9302) ;
#6831 = LINE('',#44107,#9303) ;
#6832 = LINE('',#44112,#9304) ;
#6833 = LINE('',#44114,#9305) ;
#6834 = LINE('',#44116,#9306) ;
#6835 = LINE('',#44118,#9307) ;
#6836 = LINE('',#44120,#9308) ;
#6837 = LINE('',#44121,#9309) ;
#6838 = LINE('',#44123,#9310) ;
#6839 = LINE('',#44124,#9311) ;
#6840 = LINE('',#44126,#9312) ;
#6841 = LINE('',#44128,#9313) ;
#6842 = LINE('',#44130,#9314) ;
#6843 = LINE('',#44132,#9315) ;
#6844 = LINE('',#44134,#9316) ;
#6845 = LINE('',#44136,#9317) ;
#6846 = LINE('',#44137,#9318) ;
#6847 = LINE('',#44140,#9319) ;
#6848 = LINE('',#44142,#9320) ;
#6849 = LINE('',#44143,#9321) ;
#6850 = LINE('',#44145,#9322) ;
#6851 = LINE('',#44147,#9323) ;
#6852 = LINE('',#44148,#9324) ;
#6853 = LINE('',#44149,#9325) ;
#6854 = LINE('',#44154,#9326) ;
#6855 = LINE('',#44155,#9327) ;
#6856 = LINE('',#44158,#9328) ;
#6857 = LINE('',#44159,#9329) ;
#6858 = LINE('',#44162,#9330) ;
#6859 = LINE('',#44163,#9331) ;
#6860 = LINE('',#44166,#9332) ;
#6861 = LINE('',#44168,#9333) ;
#6862 = LINE('',#44169,#9334) ;
#6863 = LINE('',#44172,#9335) ;
#6864 = LINE('',#44173,#9336) ;
#6865 = LINE('',#44176,#9337) ;
#6866 = LINE('',#44178,#9338) ;
#6867 = LINE('',#44179,#9339) ;
#6868 = LINE('',#44182,#9340) ;
#6869 = LINE('',#44183,#9341) ;
#6870 = LINE('',#44185,#9342) ;
#6871 = LINE('',#44187,#9343) ;
#6872 = LINE('',#44188,#9344) ;
#6873 = LINE('',#44191,#9345) ;
#6874 = LINE('',#44192,#9346) ;
#6875 = LINE('',#44201,#9347) ;
#6876 = LINE('',#44202,#9348) ;
#6877 = LINE('',#44204,#9349) ;
#6878 = LINE('',#44205,#9350) ;
#6879 = LINE('',#44208,#9351) ;
#6880 = LINE('',#44210,#9352) ;
#6881 = LINE('',#44211,#9353) ;
#6882 = LINE('',#44213,#9354) ;
#6883 = LINE('',#44214,#9355) ;
#6884 = LINE('',#44216,#9356) ;
#6885 = LINE('',#44219,#9357) ;
#6886 = LINE('',#44222,#9358) ;
#6887 = LINE('',#44235,#9359) ;
#6888 = LINE('',#44237,#9360) ;
#6889 = LINE('',#44239,#9361) ;
#6890 = LINE('',#44241,#9362) ;
#6891 = LINE('',#44244,#9363) ;
#6892 = LINE('',#44246,#9364) ;
#6893 = LINE('',#44247,#9365) ;
#6894 = LINE('',#44251,#9366) ;
#6895 = LINE('',#44253,#9367) ;
#6896 = LINE('',#44255,#9368) ;
#6897 = LINE('',#44256,#9369) ;
#6898 = LINE('',#44260,#9370) ;
#6899 = LINE('',#44262,#9371) ;
#6900 = LINE('',#44264,#9372) ;
#6901 = LINE('',#44265,#9373) ;
#6902 = LINE('',#44267,#9374) ;
#6903 = LINE('',#44268,#9375) ;
#6904 = LINE('',#44272,#9376) ;
#6905 = LINE('',#44273,#9377) ;
#6906 = LINE('',#44274,#9378) ;
#6907 = LINE('',#44276,#9379) ;
#6908 = LINE('',#44277,#9380) ;
#6909 = LINE('',#44279,#9381) ;
#6910 = LINE('',#44281,#9382) ;
#6911 = LINE('',#44285,#9383) ;
#6912 = LINE('',#44287,#9384) ;
#6913 = LINE('',#44289,#9385) ;
#6914 = LINE('',#44290,#9386) ;
#6915 = LINE('',#44292,#9387) ;
#6916 = LINE('',#44293,#9388) ;
#6917 = LINE('',#44295,#9389) ;
#6918 = LINE('',#44297,#9390) ;
#6919 = LINE('',#44301,#9391) ;
#6920 = LINE('',#44303,#9392) ;
#6921 = LINE('',#44305,#9393) ;
#6922 = LINE('',#44306,#9394) ;
#6923 = LINE('',#44308,#9395) ;
#6924 = LINE('',#44309,#9396) ;
#6925 = LINE('',#44311,#9397) ;
#6926 = LINE('',#44313,#9398) ;
#6927 = LINE('',#44325,#9399) ;
#6928 = LINE('',#44328,#9400) ;
#6929 = LINE('',#44338,#9401) ;
#6930 = LINE('',#44340,#9402) ;
#6931 = LINE('',#44344,#9403) ;
#6932 = LINE('',#44349,#9404) ;
#6933 = LINE('',#44351,#9405) ;
#6934 = LINE('',#44353,#9406) ;
#6935 = LINE('',#44356,#9407) ;
#6936 = LINE('',#44358,#9408) ;
#6937 = LINE('',#44359,#9409) ;
#6938 = LINE('',#44361,#9410) ;
#6939 = LINE('',#44362,#9411) ;
#6940 = LINE('',#44366,#9412) ;
#6941 = LINE('',#44368,#9413) ;
#6942 = LINE('',#44371,#9414) ;
#6943 = LINE('',#44372,#9415) ;
#6944 = LINE('',#44375,#9416) ;
#6945 = LINE('',#44377,#9417) ;
#6946 = LINE('',#44378,#9418) ;
#6947 = LINE('',#44382,#9419) ;
#6948 = LINE('',#44384,#9420) ;
#6949 = LINE('',#44386,#9421) ;
#6950 = LINE('',#44387,#9422) ;
#6951 = LINE('',#44391,#9423) ;
#6952 = LINE('',#44393,#9424) ;
#6953 = LINE('',#44395,#9425) ;
#6954 = LINE('',#44396,#9426) ;
#6955 = LINE('',#44398,#9427) ;
#6956 = LINE('',#44399,#9428) ;
#6957 = LINE('',#44400,#9429) ;
#6958 = LINE('',#44402,#9430) ;
#6959 = LINE('',#44404,#9431) ;
#6960 = LINE('',#44406,#9432) ;
#6961 = LINE('',#44413,#9433) ;
#6962 = LINE('',#44416,#9434) ;
#6963 = LINE('',#44419,#9435) ;
#6964 = LINE('',#44421,#9436) ;
#6965 = LINE('',#44422,#9437) ;
#6966 = LINE('',#44425,#9438) ;
#6967 = LINE('',#44426,#9439) ;
#6968 = LINE('',#44429,#9440) ;
#6969 = LINE('',#44430,#9441) ;
#6970 = LINE('',#44432,#9442) ;
#6971 = LINE('',#44437,#9443) ;
#6972 = LINE('',#44439,#9444) ;
#6973 = LINE('',#44441,#9445) ;
#6974 = LINE('',#44442,#9446) ;
#6975 = LINE('',#44447,#9447) ;
#6976 = LINE('',#44448,#9448) ;
#6977 = LINE('',#44451,#9449) ;
#6978 = LINE('',#44452,#9450) ;
#6979 = LINE('',#44456,#9451) ;
#6980 = LINE('',#44458,#9452) ;
#6981 = LINE('',#44464,#9453) ;
#6982 = LINE('',#44469,#9454) ;
#6983 = LINE('',#44471,#9455) ;
#6984 = LINE('',#44472,#9456) ;
#6985 = LINE('',#44477,#9457) ;
#6986 = LINE('',#44479,#9458) ;
#6987 = LINE('',#44481,#9459) ;
#6988 = LINE('',#44482,#9460) ;
#6989 = LINE('',#44485,#9461) ;
#6990 = LINE('',#44487,#9462) ;
#6991 = LINE('',#44488,#9463) ;
#6992 = LINE('',#44497,#9464) ;
#6993 = LINE('',#44500,#9465) ;
#6994 = LINE('',#44503,#9466) ;
#6995 = LINE('',#44505,#9467) ;
#6996 = LINE('',#44506,#9468) ;
#6997 = LINE('',#44509,#9469) ;
#6998 = LINE('',#44512,#9470) ;
#6999 = LINE('',#44517,#9471) ;
#7000 = LINE('',#44519,#9472) ;
#7001 = LINE('',#44521,#9473) ;
#7002 = LINE('',#44522,#9474) ;
#7003 = LINE('',#44525,#9475) ;
#7004 = LINE('',#44527,#9476) ;
#7005 = LINE('',#44528,#9477) ;
#7006 = LINE('',#44537,#9478) ;
#7007 = LINE('',#44539,#9479) ;
#7008 = LINE('',#44544,#9480) ;
#7009 = LINE('',#44547,#9481) ;
#7010 = LINE('',#44549,#9482) ;
#7011 = LINE('',#44550,#9483) ;
#7012 = LINE('',#44552,#9484) ;
#7013 = LINE('',#44557,#9485) ;
#7014 = LINE('',#44559,#9486) ;
#7015 = LINE('',#44561,#9487) ;
#7016 = LINE('',#44562,#9488) ;
#7017 = LINE('',#44567,#9489) ;
#7018 = LINE('',#44570,#9490) ;
#7019 = LINE('',#44572,#9491) ;
#7020 = LINE('',#44577,#9492) ;
#7021 = LINE('',#44579,#9493) ;
#7022 = LINE('',#44584,#9494) ;
#7023 = LINE('',#44587,#9495) ;
#7024 = LINE('',#44589,#9496) ;
#7025 = LINE('',#44590,#9497) ;
#7026 = LINE('',#44592,#9498) ;
#7027 = LINE('',#44597,#9499) ;
#7028 = LINE('',#44599,#9500) ;
#7029 = LINE('',#44601,#9501) ;
#7030 = LINE('',#44602,#9502) ;
#7031 = LINE('',#44611,#9503) ;
#7032 = LINE('',#44615,#9504) ;
#7033 = LINE('',#44618,#9505) ;
#7034 = LINE('',#44620,#9506) ;
#7035 = LINE('',#44625,#9507) ;
#7036 = LINE('',#44627,#9508) ;
#7037 = LINE('',#44629,#9509) ;
#7038 = LINE('',#44630,#9510) ;
#7039 = LINE('',#44639,#9511) ;
#7040 = LINE('',#44643,#9512) ;
#7041 = LINE('',#44646,#9513) ;
#7042 = LINE('',#44648,#9514) ;
#7043 = LINE('',#44653,#9515) ;
#7044 = LINE('',#44655,#9516) ;
#7045 = LINE('',#44657,#9517) ;
#7046 = LINE('',#44658,#9518) ;
#7047 = LINE('',#44667,#9519) ;
#7048 = LINE('',#44669,#9520) ;
#7049 = LINE('',#44671,#9521) ;
#7050 = LINE('',#44672,#9522) ;
#7051 = LINE('',#44675,#9523) ;
#7052 = LINE('',#44677,#9524) ;
#7053 = LINE('',#44678,#9525) ;
#7054 = LINE('',#44681,#9526) ;
#7055 = LINE('',#44683,#9527) ;
#7056 = LINE('',#44684,#9528) ;
#7057 = LINE('',#44686,#9529) ;
#7058 = LINE('',#44687,#9530) ;
#7059 = LINE('',#44693,#9531) ;
#7060 = LINE('',#44695,#9532) ;
#7061 = LINE('',#44697,#9533) ;
#7062 = LINE('',#44698,#9534) ;
#7063 = LINE('',#44702,#9535) ;
#7064 = LINE('',#44704,#9536) ;
#7065 = LINE('',#44706,#9537) ;
#7066 = LINE('',#44707,#9538) ;
#7067 = LINE('',#44709,#9539) ;
#7068 = LINE('',#44710,#9540) ;
#7069 = LINE('',#44712,#9541) ;
#7070 = LINE('',#44714,#9542) ;
#7071 = LINE('',#44719,#9543) ;
#7072 = LINE('',#44721,#9544) ;
#7073 = LINE('',#44723,#9545) ;
#7074 = LINE('',#44724,#9546) ;
#7075 = LINE('',#44727,#9547) ;
#7076 = LINE('',#44729,#9548) ;
#7077 = LINE('',#44730,#9549) ;
#7078 = LINE('',#44733,#9550) ;
#7079 = LINE('',#44735,#9551) ;
#7080 = LINE('',#44736,#9552) ;
#7081 = LINE('',#44739,#9553) ;
#7082 = LINE('',#44741,#9554) ;
#7083 = LINE('',#44743,#9555) ;
#7084 = LINE('',#44745,#9556) ;
#7085 = LINE('',#44747,#9557) ;
#7086 = LINE('',#44749,#9558) ;
#7087 = LINE('',#44751,#9559) ;
#7088 = LINE('',#44753,#9560) ;
#7089 = LINE('',#44754,#9561) ;
#7090 = LINE('',#44757,#9562) ;
#7091 = LINE('',#44758,#9563) ;
#7092 = LINE('',#44761,#9564) ;
#7093 = LINE('',#44762,#9565) ;
#7094 = LINE('',#44765,#9566) ;
#7095 = LINE('',#44767,#9567) ;
#7096 = LINE('',#44769,#9568) ;
#7097 = LINE('',#44771,#9569) ;
#7098 = LINE('',#44773,#9570) ;
#7099 = LINE('',#44775,#9571) ;
#7100 = LINE('',#44776,#9572) ;
#7101 = LINE('',#44778,#9573) ;
#7102 = LINE('',#44779,#9574) ;
#7103 = LINE('',#44782,#9575) ;
#7104 = LINE('',#44784,#9576) ;
#7105 = LINE('',#44786,#9577) ;
#7106 = LINE('',#44788,#9578) ;
#7107 = LINE('',#44793,#9579) ;
#7108 = LINE('',#44797,#9580) ;
#7109 = LINE('',#44800,#9581) ;
#7110 = LINE('',#44801,#9582) ;
#7111 = LINE('',#44808,#9583) ;
#7112 = LINE('',#44811,#9584) ;
#7113 = LINE('',#44813,#9585) ;
#7114 = LINE('',#44814,#9586) ;
#7115 = LINE('',#44819,#9587) ;
#7116 = LINE('',#44823,#9588) ;
#7117 = LINE('',#44827,#9589) ;
#7118 = LINE('',#44831,#9590) ;
#7119 = LINE('',#44834,#9591) ;
#7120 = LINE('',#44836,#9592) ;
#7121 = LINE('',#44838,#9593) ;
#7122 = LINE('',#44840,#9594) ;
#7123 = LINE('',#44846,#9595) ;
#7124 = LINE('',#44848,#9596) ;
#7125 = LINE('',#44850,#9597) ;
#7126 = LINE('',#44851,#9598) ;
#7127 = LINE('',#44855,#9599) ;
#7128 = LINE('',#44857,#9600) ;
#7129 = LINE('',#44859,#9601) ;
#7130 = LINE('',#44860,#9602) ;
#7131 = LINE('',#44862,#9603) ;
#7132 = LINE('',#44863,#9604) ;
#7133 = LINE('',#44865,#9605) ;
#7134 = LINE('',#44867,#9606) ;
#7135 = LINE('',#44910,#9607) ;
#7136 = LINE('',#44955,#9608) ;
#7137 = LINE('',#44961,#9609) ;
#7138 = LINE('',#45004,#9610) ;
#7139 = LINE('',#45049,#9611) ;
#7140 = LINE('',#45055,#9612) ;
#7141 = LINE('',#45071,#9613) ;
#7142 = LINE('',#45077,#9614) ;
#7143 = LINE('',#45083,#9615) ;
#7144 = LINE('',#45089,#9616) ;
#7145 = LINE('',#45094,#9617) ;
#7146 = LINE('',#45098,#9618) ;
#7147 = LINE('',#45101,#9619) ;
#7148 = LINE('',#45104,#9620) ;
#7149 = LINE('',#45106,#9621) ;
#7150 = LINE('',#45117,#9622) ;
#7151 = LINE('',#45119,#9623) ;
#7152 = LINE('',#45123,#9624) ;
#7153 = LINE('',#45127,#9625) ;
#7154 = LINE('',#45129,#9626) ;
#7155 = LINE('',#45131,#9627) ;
#7156 = LINE('',#45134,#9628) ;
#7157 = LINE('',#45138,#9629) ;
#7158 = LINE('',#45141,#9630) ;
#7159 = LINE('',#45142,#9631) ;
#7160 = LINE('',#45145,#9632) ;
#7161 = LINE('',#45147,#9633) ;
#7162 = LINE('',#45149,#9634) ;
#7163 = LINE('',#45151,#9635) ;
#7164 = LINE('',#45153,#9636) ;
#7165 = LINE('',#45155,#9637) ;
#7166 = LINE('',#45157,#9638) ;
#7167 = LINE('',#45159,#9639) ;
#7168 = LINE('',#45161,#9640) ;
#7169 = LINE('',#45163,#9641) ;
#7170 = LINE('',#45164,#9642) ;
#7171 = LINE('',#45170,#9643) ;
#7172 = LINE('',#45173,#9644) ;
#7173 = LINE('',#45174,#9645) ;
#7174 = LINE('',#45177,#9646) ;
#7175 = LINE('',#45179,#9647) ;
#7176 = LINE('',#45181,#9648) ;
#7177 = LINE('',#45183,#9649) ;
#7178 = LINE('',#45185,#9650) ;
#7179 = LINE('',#45187,#9651) ;
#7180 = LINE('',#45189,#9652) ;
#7181 = LINE('',#45191,#9653) ;
#7182 = LINE('',#45193,#9654) ;
#7183 = LINE('',#45195,#9655) ;
#7184 = LINE('',#45196,#9656) ;
#7185 = LINE('',#45198,#9657) ;
#7186 = LINE('',#45200,#9658) ;
#7187 = LINE('',#45201,#9659) ;
#7188 = LINE('',#45211,#9660) ;
#7189 = LINE('',#45217,#9661) ;
#7190 = LINE('',#45222,#9662) ;
#7191 = LINE('',#45226,#9663) ;
#7192 = LINE('',#45231,#9664) ;
#7193 = LINE('',#45235,#9665) ;
#7194 = LINE('',#45239,#9666) ;
#7195 = LINE('',#45241,#9667) ;
#7196 = LINE('',#45243,#9668) ;
#7197 = LINE('',#45245,#9669) ;
#7198 = LINE('',#45246,#9670) ;
#7199 = LINE('',#45249,#9671) ;
#7200 = LINE('',#45250,#9672) ;
#7201 = LINE('',#45253,#9673) ;
#7202 = LINE('',#45254,#9674) ;
#7203 = LINE('',#45257,#9675) ;
#7204 = LINE('',#45259,#9676) ;
#7205 = LINE('',#45261,#9677) ;
#7206 = LINE('',#45263,#9678) ;
#7207 = LINE('',#45264,#9679) ;
#7208 = LINE('',#45267,#9680) ;
#7209 = LINE('',#45268,#9681) ;
#7210 = LINE('',#45271,#9682) ;
#7211 = LINE('',#45272,#9683) ;
#7212 = LINE('',#45275,#9684) ;
#7213 = LINE('',#45276,#9685) ;
#7214 = LINE('',#45279,#9686) ;
#7215 = LINE('',#45280,#9687) ;
#7216 = LINE('',#45282,#9688) ;
#7217 = LINE('',#45285,#9689) ;
#7218 = LINE('',#45286,#9690) ;
#7219 = LINE('',#45289,#9691) ;
#7220 = LINE('',#45290,#9692) ;
#7221 = LINE('',#45292,#9693) ;
#7222 = LINE('',#45301,#9694) ;
#7223 = LINE('',#45302,#9695) ;
#7224 = LINE('',#45303,#9696) ;
#7225 = LINE('',#45307,#9697) ;
#7226 = LINE('',#45312,#9698) ;
#7227 = LINE('',#45320,#9699) ;
#7228 = LINE('',#45327,#9700) ;
#7229 = LINE('',#45334,#9701) ;
#7230 = LINE('',#45339,#9702) ;
#7231 = LINE('',#45345,#9703) ;
#7232 = LINE('',#45346,#9704) ;
#7233 = LINE('',#45347,#9705) ;
#7234 = LINE('',#45351,#9706) ;
#7235 = LINE('',#45352,#9707) ;
#7236 = LINE('',#45353,#9708) ;
#7237 = LINE('',#45355,#9709) ;
#7238 = LINE('',#45357,#9710) ;
#7239 = LINE('',#45359,#9711) ;
#7240 = LINE('',#45361,#9712) ;
#7241 = LINE('',#45363,#9713) ;
#7242 = LINE('',#45364,#9714) ;
#7243 = LINE('',#45368,#9715) ;
#7244 = LINE('',#45369,#9716) ;
#7245 = LINE('',#45370,#9717) ;
#7246 = LINE('',#45374,#9718) ;
#7247 = LINE('',#45375,#9719) ;
#7248 = LINE('',#45376,#9720) ;
#7249 = LINE('',#45378,#9721) ;
#7250 = LINE('',#45380,#9722) ;
#7251 = LINE('',#45383,#9723) ;
#7252 = LINE('',#45384,#9724) ;
#7253 = LINE('',#45387,#9725) ;
#7254 = LINE('',#45388,#9726) ;
#7255 = LINE('',#45390,#9727) ;
#7256 = LINE('',#45394,#9728) ;
#7257 = LINE('',#45396,#9729) ;
#7258 = LINE('',#45397,#9730) ;
#7259 = LINE('',#45400,#9731) ;
#7260 = LINE('',#45402,#9732) ;
#7261 = LINE('',#45403,#9733) ;
#7262 = LINE('',#45405,#9734) ;
#7263 = LINE('',#45406,#9735) ;
#7264 = LINE('',#45409,#9736) ;
#7265 = LINE('',#45416,#9737) ;
#7266 = LINE('',#45422,#9738) ;
#7267 = LINE('',#45424,#9739) ;
#7268 = LINE('',#45426,#9740) ;
#7269 = LINE('',#45427,#9741) ;
#7270 = LINE('',#45431,#9742) ;
#7271 = LINE('',#45433,#9743) ;
#7272 = LINE('',#45435,#9744) ;
#7273 = LINE('',#45436,#9745) ;
#7274 = LINE('',#45439,#9746) ;
#7275 = LINE('',#45440,#9747) ;
#7276 = LINE('',#45442,#9748) ;
#7277 = LINE('',#45443,#9749) ;
#7278 = LINE('',#45446,#9750) ;
#7279 = LINE('',#45447,#9751) ;
#7280 = LINE('',#45450,#9752) ;
#7281 = LINE('',#45451,#9753) ;
#7282 = LINE('',#45453,#9754) ;
#7283 = LINE('',#45455,#9755) ;
#7284 = LINE('',#45461,#9756) ;
#7285 = LINE('',#45465,#9757) ;
#7286 = LINE('',#45467,#9758) ;
#7287 = LINE('',#45472,#9759) ;
#7288 = LINE('',#45476,#9760) ;
#7289 = LINE('',#45478,#9761) ;
#7290 = LINE('',#45483,#9762) ;
#7291 = LINE('',#45487,#9763) ;
#7292 = LINE('',#45492,#9764) ;
#7293 = LINE('',#45496,#9765) ;
#7294 = LINE('',#45499,#9766) ;
#7295 = LINE('',#45503,#9767) ;
#7296 = LINE('',#45507,#9768) ;
#7297 = LINE('',#45509,#9769) ;
#7298 = LINE('',#45514,#9770) ;
#7299 = LINE('',#45518,#9771) ;
#7300 = LINE('',#45522,#9772) ;
#7301 = LINE('',#45525,#9773) ;
#7302 = LINE('',#45528,#9774) ;
#7303 = LINE('',#45531,#9775) ;
#7304 = LINE('',#45534,#9776) ;
#7305 = LINE('',#45536,#9777) ;
#7306 = LINE('',#45540,#9778) ;
#7307 = LINE('',#45543,#9779) ;
#7308 = LINE('',#45546,#9780) ;
#7309 = LINE('',#45549,#9781) ;
#7310 = LINE('',#45552,#9782) ;
#7311 = LINE('',#45555,#9783) ;
#7312 = LINE('',#45558,#9784) ;
#7313 = LINE('',#45560,#9785) ;
#7314 = LINE('',#45562,#9786) ;
#7315 = LINE('',#45566,#9787) ;
#7316 = LINE('',#45571,#9788) ;
#7317 = LINE('',#45574,#9789) ;
#7318 = LINE('',#45576,#9790) ;
#7319 = LINE('',#45579,#9791) ;
#7320 = LINE('',#45582,#9792) ;
#7321 = LINE('',#45586,#9793) ;
#7322 = LINE('',#45587,#9794) ;
#7323 = LINE('',#45590,#9795) ;
#7324 = LINE('',#45594,#9796) ;
#7325 = LINE('',#45595,#9797) ;
#7326 = LINE('',#45598,#9798) ;
#7327 = LINE('',#45601,#9799) ;
#7328 = LINE('',#45604,#9800) ;
#7329 = LINE('',#45606,#9801) ;
#7330 = LINE('',#45608,#9802) ;
#7331 = LINE('',#45610,#9803) ;
#7332 = LINE('',#45611,#9804) ;
#7333 = LINE('',#45614,#9805) ;
#7334 = LINE('',#45616,#9806) ;
#7335 = LINE('',#45618,#9807) ;
#7336 = LINE('',#45620,#9808) ;
#7337 = LINE('',#45621,#9809) ;
#7338 = LINE('',#45624,#9810) ;
#7339 = LINE('',#45626,#9811) ;
#7340 = LINE('',#45627,#9812) ;
#7341 = LINE('',#45630,#9813) ;
#7342 = LINE('',#45631,#9814) ;
#7343 = LINE('',#45633,#9815) ;
#7344 = LINE('',#45634,#9816) ;
#7345 = LINE('',#45637,#9817) ;
#7346 = LINE('',#45638,#9818) ;
#7347 = LINE('',#45641,#9819) ;
#7348 = LINE('',#45642,#9820) ;
#7349 = LINE('',#45645,#9821) ;
#7350 = LINE('',#45647,#9822) ;
#7351 = LINE('',#45649,#9823) ;
#7352 = LINE('',#45651,#9824) ;
#7353 = LINE('',#45652,#9825) ;
#7354 = LINE('',#45655,#9826) ;
#7355 = LINE('',#45657,#9827) ;
#7356 = LINE('',#45658,#9828) ;
#7357 = LINE('',#45661,#9829) ;
#7358 = LINE('',#45663,#9830) ;
#7359 = LINE('',#45665,#9831) ;
#7360 = LINE('',#45667,#9832) ;
#7361 = LINE('',#45668,#9833) ;
#7362 = LINE('',#45671,#9834) ;
#7363 = LINE('',#45673,#9835) ;
#7364 = LINE('',#45674,#9836) ;
#7365 = LINE('',#45677,#9837) ;
#7366 = LINE('',#45679,#9838) ;
#7367 = LINE('',#45680,#9839) ;
#7368 = LINE('',#45683,#9840) ;
#7369 = LINE('',#45685,#9841) ;
#7370 = LINE('',#45687,#9842) ;
#7371 = LINE('',#45689,#9843) ;
#7372 = LINE('',#45690,#9844) ;
#7373 = LINE('',#45694,#9845) ;
#7374 = LINE('',#45700,#9846) ;
#7375 = LINE('',#45704,#9847) ;
#7376 = LINE('',#45709,#9848) ;
#7377 = LINE('',#45715,#9849) ;
#7378 = LINE('',#45717,#9850) ;
#7379 = LINE('',#45718,#9851) ;
#7380 = LINE('',#45719,#9852) ;
#7381 = LINE('',#45721,#9853) ;
#7382 = LINE('',#45722,#9854) ;
#7383 = LINE('',#45723,#9855) ;
#7384 = LINE('',#45725,#9856) ;
#7385 = LINE('',#45726,#9857) ;
#7386 = LINE('',#45729,#9858) ;
#7387 = LINE('',#45731,#9859) ;
#7388 = LINE('',#45732,#9860) ;
#7389 = LINE('',#45734,#9861) ;
#7390 = LINE('',#45736,#9862) ;
#7391 = LINE('',#45741,#9863) ;
#7392 = LINE('',#45746,#9864) ;
#7393 = LINE('',#45748,#9865) ;
#7394 = LINE('',#45751,#9866) ;
#7395 = LINE('',#45753,#9867) ;
#7396 = LINE('',#45758,#9868) ;
#7397 = LINE('',#45759,#9869) ;
#7398 = LINE('',#45762,#9870) ;
#7399 = LINE('',#45763,#9871) ;
#7400 = LINE('',#45765,#9872) ;
#7401 = LINE('',#45768,#9873) ;
#7402 = LINE('',#45772,#9874) ;
#7403 = LINE('',#45773,#9875) ;
#7404 = LINE('',#45775,#9876) ;
#7405 = LINE('',#45781,#9877) ;
#7406 = LINE('',#45790,#9878) ;
#7407 = LINE('',#45797,#9879) ;
#7408 = LINE('',#45803,#9880) ;
#7409 = LINE('',#45813,#9881) ;
#7410 = LINE('',#45816,#9882) ;
#7411 = LINE('',#45819,#9883) ;
#7412 = LINE('',#45821,#9884) ;
#7413 = LINE('',#45823,#9885) ;
#7414 = LINE('',#45825,#9886) ;
#7415 = LINE('',#45826,#9887) ;
#7416 = LINE('',#45829,#9888) ;
#7417 = LINE('',#45831,#9889) ;
#7418 = LINE('',#45832,#9890) ;
#7419 = LINE('',#45835,#9891) ;
#7420 = LINE('',#45836,#9892) ;
#7421 = LINE('',#45838,#9893) ;
#7422 = LINE('',#45839,#9894) ;
#7423 = LINE('',#45844,#9895) ;
#7424 = LINE('',#45848,#9896) ;
#7425 = LINE('',#45852,#9897) ;
#7426 = LINE('',#45855,#9898) ;
#7427 = LINE('',#45858,#9899) ;
#7428 = LINE('',#45859,#9900) ;
#7429 = LINE('',#45860,#9901) ;
#7430 = LINE('',#45863,#9902) ;
#7431 = LINE('',#45865,#9903) ;
#7432 = LINE('',#45867,#9904) ;
#7433 = LINE('',#45868,#9905) ;
#7434 = LINE('',#45871,#9906) ;
#7435 = LINE('',#45873,#9907) ;
#7436 = LINE('',#45874,#9908) ;
#7437 = LINE('',#45876,#9909) ;
#7438 = LINE('',#45877,#9910) ;
#7439 = LINE('',#45880,#9911) ;
#7440 = LINE('',#45882,#9912) ;
#7441 = LINE('',#45889,#9913) ;
#7442 = LINE('',#45898,#9914) ;
#7443 = LINE('',#45905,#9915) ;
#7444 = LINE('',#45911,#9916) ;
#7445 = LINE('',#45920,#9917) ;
#7446 = LINE('',#45926,#9918) ;
#7447 = LINE('',#45934,#9919) ;
#7448 = LINE('',#45940,#9920) ;
#7449 = LINE('',#45948,#9921) ;
#7450 = LINE('',#45964,#9922) ;
#7451 = LINE('',#45969,#9923) ;
#7452 = LINE('',#45973,#9924) ;
#7453 = LINE('',#45977,#9925) ;
#7454 = LINE('',#45981,#9926) ;
#7455 = LINE('',#45984,#9927) ;
#7456 = LINE('',#45988,#9928) ;
#7457 = LINE('',#45993,#9929) ;
#7458 = LINE('',#45997,#9930) ;
#7459 = LINE('',#46001,#9931) ;
#7460 = LINE('',#46005,#9932) ;
#7461 = LINE('',#46009,#9933) ;
#7462 = LINE('',#46013,#9934) ;
#7463 = LINE('',#46017,#9935) ;
#7464 = LINE('',#46021,#9936) ;
#7465 = LINE('',#46025,#9937) ;
#7466 = LINE('',#46029,#9938) ;
#7467 = LINE('',#46033,#9939) ;
#7468 = LINE('',#46037,#9940) ;
#7469 = LINE('',#46041,#9941) ;
#7470 = LINE('',#46045,#9942) ;
#7471 = LINE('',#46047,#9943) ;
#7472 = LINE('',#46048,#9944) ;
#7473 = LINE('',#46051,#9945) ;
#7474 = LINE('',#46052,#9946) ;
#7475 = LINE('',#46055,#9947) ;
#7476 = LINE('',#46056,#9948) ;
#7477 = LINE('',#46059,#9949) ;
#7478 = LINE('',#46061,#9950) ;
#7479 = LINE('',#46062,#9951) ;
#7480 = LINE('',#46064,#9952) ;
#7481 = LINE('',#46067,#9953) ;
#7482 = LINE('',#46068,#9954) ;
#7483 = LINE('',#46071,#9955) ;
#7484 = LINE('',#46072,#9956) ;
#7485 = LINE('',#46075,#9957) ;
#7486 = LINE('',#46079,#9958) ;
#7487 = LINE('',#46081,#9959) ;
#7488 = LINE('',#46082,#9960) ;
#7489 = LINE('',#46085,#9961) ;
#7490 = LINE('',#46086,#9962) ;
#7491 = LINE('',#46089,#9963) ;
#7492 = LINE('',#46090,#9964) ;
#7493 = LINE('',#46093,#9965) ;
#7494 = LINE('',#46095,#9966) ;
#7495 = LINE('',#46096,#9967) ;
#7496 = LINE('',#46098,#9968) ;
#7497 = LINE('',#46101,#9969) ;
#7498 = LINE('',#46102,#9970) ;
#7499 = LINE('',#46105,#9971) ;
#7500 = LINE('',#46106,#9972) ;
#7501 = LINE('',#46108,#9973) ;
#7502 = LINE('',#46113,#9974) ;
#7503 = LINE('',#46115,#9975) ;
#7504 = LINE('',#46116,#9976) ;
#7505 = LINE('',#46119,#9977) ;
#7506 = LINE('',#46120,#9978) ;
#7507 = LINE('',#46123,#9979) ;
#7508 = LINE('',#46124,#9980) ;
#7509 = LINE('',#46127,#9981) ;
#7510 = LINE('',#46129,#9982) ;
#7511 = LINE('',#46130,#9983) ;
#7512 = LINE('',#46132,#9984) ;
#7513 = LINE('',#46135,#9985) ;
#7514 = LINE('',#46136,#9986) ;
#7515 = LINE('',#46139,#9987) ;
#7516 = LINE('',#46140,#9988) ;
#7517 = LINE('',#46143,#9989) ;
#7518 = LINE('',#46147,#9990) ;
#7519 = LINE('',#46149,#9991) ;
#7520 = LINE('',#46150,#9992) ;
#7521 = LINE('',#46153,#9993) ;
#7522 = LINE('',#46154,#9994) ;
#7523 = LINE('',#46157,#9995) ;
#7524 = LINE('',#46158,#9996) ;
#7525 = LINE('',#46161,#9997) ;
#7526 = LINE('',#46163,#9998) ;
#7527 = LINE('',#46164,#9999) ;
#7528 = LINE('',#46166,#10000) ;
#7529 = LINE('',#46169,#10001) ;
#7530 = LINE('',#46170,#10002) ;
#7531 = LINE('',#46173,#10003) ;
#7532 = LINE('',#46174,#10004) ;
#7533 = LINE('',#46176,#10005) ;
#7534 = LINE('',#46181,#10006) ;
#7535 = LINE('',#46190,#10007) ;
#7536 = LINE('',#46196,#10008) ;
#7537 = LINE('',#46216,#10009) ;
#7538 = LINE('',#46221,#10010) ;
#7539 = LINE('',#46223,#10011) ;
#7540 = LINE('',#46225,#10012) ;
#7541 = LINE('',#46226,#10013) ;
#7542 = LINE('',#46229,#10014) ;
#7543 = LINE('',#46231,#10015) ;
#7544 = LINE('',#46232,#10016) ;
#7545 = LINE('',#46236,#10017) ;
#7546 = LINE('',#46238,#10018) ;
#7547 = LINE('',#46239,#10019) ;
#7548 = LINE('',#46240,#10020) ;
#7549 = LINE('',#46244,#10021) ;
#7550 = LINE('',#46245,#10022) ;
#7551 = LINE('',#46246,#10023) ;
#7552 = LINE('',#46248,#10024) ;
#7553 = LINE('',#46251,#10025) ;
#7554 = LINE('',#46252,#10026) ;
#7555 = LINE('',#46254,#10027) ;
#7556 = LINE('',#46259,#10028) ;
#7557 = LINE('',#46264,#10029) ;
#7558 = LINE('',#46266,#10030) ;
#7559 = LINE('',#46268,#10031) ;
#7560 = LINE('',#46269,#10032) ;
#7561 = LINE('',#46272,#10033) ;
#7562 = LINE('',#46274,#10034) ;
#7563 = LINE('',#46275,#10035) ;
#7564 = LINE('',#46278,#10036) ;
#7565 = LINE('',#46279,#10037) ;
#7566 = LINE('',#46282,#10038) ;
#7567 = LINE('',#46283,#10039) ;
#7568 = LINE('',#46285,#10040) ;
#7569 = LINE('',#46290,#10041) ;
#7570 = LINE('',#46296,#10042) ;
#7571 = LINE('',#46302,#10043) ;
#7572 = LINE('',#46308,#10044) ;
#7573 = LINE('',#46314,#10045) ;
#7574 = LINE('',#46318,#10046) ;
#7575 = LINE('',#46322,#10047) ;
#7576 = LINE('',#46326,#10048) ;
#7577 = LINE('',#46328,#10049) ;
#7578 = LINE('',#46330,#10050) ;
#7579 = LINE('',#46332,#10051) ;
#7580 = LINE('',#46334,#10052) ;
#7581 = LINE('',#46336,#10053) ;
#7582 = LINE('',#46338,#10054) ;
#7583 = LINE('',#46346,#10055) ;
#7584 = LINE('',#46348,#10056) ;
#7585 = LINE('',#46350,#10057) ;
#7586 = LINE('',#46352,#10058) ;
#7587 = LINE('',#46354,#10059) ;
#7588 = LINE('',#46356,#10060) ;
#7589 = LINE('',#46357,#10061) ;
#7590 = LINE('',#46360,#10062) ;
#7591 = LINE('',#46361,#10063) ;
#7592 = LINE('',#46367,#10064) ;
#7593 = LINE('',#46369,#10065) ;
#7594 = LINE('',#46371,#10066) ;
#7595 = LINE('',#46373,#10067) ;
#7596 = LINE('',#46374,#10068) ;
#7597 = LINE('',#46376,#10069) ;
#7598 = LINE('',#46377,#10070) ;
#7599 = LINE('',#46379,#10071) ;
#7600 = LINE('',#46381,#10072) ;
#7601 = LINE('',#46382,#10073) ;
#7602 = LINE('',#46384,#10074) ;
#7603 = LINE('',#46387,#10075) ;
#7604 = LINE('',#46389,#10076) ;
#7605 = LINE('',#46391,#10077) ;
#7606 = LINE('',#46392,#10078) ;
#7607 = LINE('',#46394,#10079) ;
#7608 = LINE('',#46396,#10080) ;
#7609 = LINE('',#46398,#10081) ;
#7610 = LINE('',#46401,#10082) ;
#7611 = LINE('',#46404,#10083) ;
#7612 = LINE('',#46408,#10084) ;
#7613 = LINE('',#46410,#10085) ;
#7614 = LINE('',#46412,#10086) ;
#7615 = LINE('',#46413,#10087) ;
#7616 = LINE('',#46417,#10088) ;
#7617 = LINE('',#46418,#10089) ;
#7618 = LINE('',#46420,#10090) ;
#7619 = LINE('',#46422,#10091) ;
#7620 = LINE('',#46428,#10092) ;
#7621 = LINE('',#46430,#10093) ;
#7622 = LINE('',#46432,#10094) ;
#7623 = LINE('',#46433,#10095) ;
#7624 = LINE('',#46436,#10096) ;
#7625 = LINE('',#46438,#10097) ;
#7626 = LINE('',#46439,#10098) ;
#7627 = LINE('',#46443,#10099) ;
#7628 = LINE('',#46445,#10100) ;
#7629 = LINE('',#46446,#10101) ;
#7630 = LINE('',#46447,#10102) ;
#7631 = LINE('',#46451,#10103) ;
#7632 = LINE('',#46452,#10104) ;
#7633 = LINE('',#46454,#10105) ;
#7634 = LINE('',#46455,#10106) ;
#7635 = LINE('',#46458,#10107) ;
#7636 = LINE('',#46459,#10108) ;
#7637 = LINE('',#46460,#10109) ;
#7638 = LINE('',#46463,#10110) ;
#7639 = LINE('',#46464,#10111) ;
#7640 = LINE('',#46470,#10112) ;
#7641 = LINE('',#46475,#10113) ;
#7642 = LINE('',#46477,#10114) ;
#7643 = LINE('',#46479,#10115) ;
#7644 = LINE('',#46480,#10116) ;
#7645 = LINE('',#46484,#10117) ;
#7646 = LINE('',#46486,#10118) ;
#7647 = LINE('',#46488,#10119) ;
#7648 = LINE('',#46489,#10120) ;
#7649 = LINE('',#46491,#10121) ;
#7650 = LINE('',#46492,#10122) ;
#7651 = LINE('',#46495,#10123) ;
#7652 = LINE('',#46497,#10124) ;
#7653 = LINE('',#46498,#10125) ;
#7654 = LINE('',#46501,#10126) ;
#7655 = LINE('',#46502,#10127) ;
#7656 = LINE('',#46503,#10128) ;
#7657 = LINE('',#46508,#10129) ;
#7658 = LINE('',#46513,#10130) ;
#7659 = LINE('',#46515,#10131) ;
#7660 = LINE('',#46517,#10132) ;
#7661 = LINE('',#46518,#10133) ;
#7662 = LINE('',#46522,#10134) ;
#7663 = LINE('',#46523,#10135) ;
#7664 = LINE('',#46524,#10136) ;
#7665 = LINE('',#46528,#10137) ;
#7666 = LINE('',#46529,#10138) ;
#7667 = LINE('',#46530,#10139) ;
#7668 = LINE('',#46533,#10140) ;
#7669 = LINE('',#46535,#10141) ;
#7670 = LINE('',#46536,#10142) ;
#7671 = LINE('',#46539,#10143) ;
#7672 = LINE('',#46541,#10144) ;
#7673 = LINE('',#46542,#10145) ;
#7674 = LINE('',#46547,#10146) ;
#7675 = LINE('',#46550,#10147) ;
#7676 = LINE('',#46551,#10148) ;
#7677 = LINE('',#46553,#10149) ;
#7678 = LINE('',#46554,#10150) ;
#7679 = LINE('',#46561,#10151) ;
#7680 = LINE('',#46563,#10152) ;
#7681 = LINE('',#46565,#10153) ;
#7682 = LINE('',#46566,#10154) ;
#7683 = LINE('',#46569,#10155) ;
#7684 = LINE('',#46571,#10156) ;
#7685 = LINE('',#46572,#10157) ;
#7686 = LINE('',#46575,#10158) ;
#7687 = LINE('',#46576,#10159) ;
#7688 = LINE('',#46579,#10160) ;
#7689 = LINE('',#46580,#10161) ;
#7690 = LINE('',#46583,#10162) ;
#7691 = LINE('',#46585,#10163) ;
#7692 = LINE('',#46587,#10164) ;
#7693 = LINE('',#46589,#10165) ;
#7694 = LINE('',#46591,#10166) ;
#7695 = LINE('',#46593,#10167) ;
#7696 = LINE('',#46595,#10168) ;
#7697 = LINE('',#46597,#10169) ;
#7698 = LINE('',#46599,#10170) ;
#7699 = LINE('',#46601,#10171) ;
#7700 = LINE('',#46603,#10172) ;
#7701 = LINE('',#46605,#10173) ;
#7702 = LINE('',#46607,#10174) ;
#7703 = LINE('',#46609,#10175) ;
#7704 = LINE('',#46611,#10176) ;
#7705 = LINE('',#46613,#10177) ;
#7706 = LINE('',#46615,#10178) ;
#7707 = LINE('',#46617,#10179) ;
#7708 = LINE('',#46619,#10180) ;
#7709 = LINE('',#46621,#10181) ;
#7710 = LINE('',#46623,#10182) ;
#7711 = LINE('',#46625,#10183) ;
#7712 = LINE('',#46627,#10184) ;
#7713 = LINE('',#46629,#10185) ;
#7714 = LINE('',#46631,#10186) ;
#7715 = LINE('',#46633,#10187) ;
#7716 = LINE('',#46635,#10188) ;
#7717 = LINE('',#46637,#10189) ;
#7718 = LINE('',#46639,#10190) ;
#7719 = LINE('',#46641,#10191) ;
#7720 = LINE('',#46643,#10192) ;
#7721 = LINE('',#46645,#10193) ;
#7722 = LINE('',#46647,#10194) ;
#7723 = LINE('',#46649,#10195) ;
#7724 = LINE('',#46651,#10196) ;
#7725 = LINE('',#46653,#10197) ;
#7726 = LINE('',#46654,#10198) ;
#7727 = LINE('',#46658,#10199) ;
#7728 = LINE('',#46660,#10200) ;
#7729 = LINE('',#46662,#10201) ;
#7730 = LINE('',#46663,#10202) ;
#7731 = LINE('',#46665,#10203) ;
#7732 = LINE('',#46666,#10204) ;
#7733 = LINE('',#46668,#10205) ;
#7734 = LINE('',#46670,#10206) ;
#7735 = LINE('',#46673,#10207) ;
#7736 = LINE('',#46675,#10208) ;
#7737 = LINE('',#46676,#10209) ;
#7738 = LINE('',#46678,#10210) ;
#7739 = LINE('',#46680,#10211) ;
#7740 = LINE('',#46681,#10212) ;
#7741 = LINE('',#46683,#10213) ;
#7742 = LINE('',#46685,#10214) ;
#7743 = LINE('',#46686,#10215) ;
#7744 = LINE('',#46688,#10216) ;
#7745 = LINE('',#46690,#10217) ;
#7746 = LINE('',#46691,#10218) ;
#7747 = LINE('',#46693,#10219) ;
#7748 = LINE('',#46695,#10220) ;
#7749 = LINE('',#46696,#10221) ;
#7750 = LINE('',#46698,#10222) ;
#7751 = LINE('',#46700,#10223) ;
#7752 = LINE('',#46701,#10224) ;
#7753 = LINE('',#46703,#10225) ;
#7754 = LINE('',#46705,#10226) ;
#7755 = LINE('',#46706,#10227) ;
#7756 = LINE('',#46708,#10228) ;
#7757 = LINE('',#46710,#10229) ;
#7758 = LINE('',#46711,#10230) ;
#7759 = LINE('',#46714,#10231) ;
#7760 = LINE('',#46716,#10232) ;
#7761 = LINE('',#46717,#10233) ;
#7762 = LINE('',#46719,#10234) ;
#7763 = LINE('',#46721,#10235) ;
#7764 = LINE('',#46725,#10236) ;
#7765 = LINE('',#46727,#10237) ;
#7766 = LINE('',#46728,#10238) ;
#7767 = LINE('',#46730,#10239) ;
#7768 = LINE('',#46732,#10240) ;
#7769 = LINE('',#46736,#10241) ;
#7770 = LINE('',#46738,#10242) ;
#7771 = LINE('',#46739,#10243) ;
#7772 = LINE('',#46741,#10244) ;
#7773 = LINE('',#46743,#10245) ;
#7774 = LINE('',#46747,#10246) ;
#7775 = LINE('',#46749,#10247) ;
#7776 = LINE('',#46750,#10248) ;
#7777 = LINE('',#46752,#10249) ;
#7778 = LINE('',#46754,#10250) ;
#7779 = LINE('',#46758,#10251) ;
#7780 = LINE('',#46760,#10252) ;
#7781 = LINE('',#46761,#10253) ;
#7782 = LINE('',#46763,#10254) ;
#7783 = LINE('',#46765,#10255) ;
#7784 = LINE('',#46769,#10256) ;
#7785 = LINE('',#46771,#10257) ;
#7786 = LINE('',#46772,#10258) ;
#7787 = LINE('',#46774,#10259) ;
#7788 = LINE('',#46776,#10260) ;
#7789 = LINE('',#46780,#10261) ;
#7790 = LINE('',#46782,#10262) ;
#7791 = LINE('',#46783,#10263) ;
#7792 = LINE('',#46785,#10264) ;
#7793 = LINE('',#46787,#10265) ;
#7794 = LINE('',#46791,#10266) ;
#7795 = LINE('',#46793,#10267) ;
#7796 = LINE('',#46794,#10268) ;
#7797 = LINE('',#46796,#10269) ;
#7798 = LINE('',#46798,#10270) ;
#7799 = LINE('',#46805,#10271) ;
#7800 = LINE('',#46811,#10272) ;
#7801 = LINE('',#46817,#10273) ;
#7802 = LINE('',#46823,#10274) ;
#7803 = LINE('',#46828,#10275) ;
#7804 = LINE('',#46832,#10276) ;
#7805 = LINE('',#46929,#10277) ;
#7806 = LINE('',#46931,#10278) ;
#7807 = LINE('',#46933,#10279) ;
#7808 = LINE('',#46934,#10280) ;
#7809 = LINE('',#46944,#10281) ;
#7810 = LINE('',#46950,#10282) ;
#7811 = LINE('',#46952,#10283) ;
#7812 = LINE('',#46954,#10284) ;
#7813 = LINE('',#46955,#10285) ;
#7814 = LINE('',#46957,#10286) ;
#7815 = LINE('',#46958,#10287) ;
#7816 = LINE('',#46960,#10288) ;
#7817 = LINE('',#46962,#10289) ;
#7818 = LINE('',#46966,#10290) ;
#7819 = LINE('',#46974,#10291) ;
#7820 = LINE('',#46978,#10292) ;
#7821 = LINE('',#46984,#10293) ;
#7822 = LINE('',#46999,#10294) ;
#7823 = LINE('',#47001,#10295) ;
#7824 = LINE('',#47007,#10296) ;
#7825 = LINE('',#47013,#10297) ;
#7826 = LINE('',#47019,#10298) ;
#7827 = LINE('',#47025,#10299) ;
#7828 = LINE('',#47031,#10300) ;
#7829 = LINE('',#47037,#10301) ;
#7830 = LINE('',#47043,#10302) ;
#7831 = LINE('',#47049,#10303) ;
#7832 = LINE('',#47054,#10304) ;
#7833 = LINE('',#47056,#10305) ;
#7834 = LINE('',#47058,#10306) ;
#7835 = LINE('',#47059,#10307) ;
#7836 = LINE('',#47072,#10308) ;
#7837 = LINE('',#47077,#10309) ;
#7838 = LINE('',#47079,#10310) ;
#7839 = LINE('',#47080,#10311) ;
#7840 = LINE('',#47083,#10312) ;
#7841 = LINE('',#47085,#10313) ;
#7842 = LINE('',#47086,#10314) ;
#7843 = LINE('',#47091,#10315) ;
#7844 = LINE('',#47100,#10316) ;
#7845 = LINE('',#47105,#10317) ;
#7846 = LINE('',#47110,#10318) ;
#7847 = LINE('',#47112,#10319) ;
#7848 = LINE('',#47114,#10320) ;
#7849 = LINE('',#47115,#10321) ;
#7850 = LINE('',#47118,#10322) ;
#7851 = LINE('',#47120,#10323) ;
#7852 = LINE('',#47122,#10324) ;
#7853 = LINE('',#47123,#10325) ;
#7854 = LINE('',#47127,#10326) ;
#7855 = LINE('',#47129,#10327) ;
#7856 = LINE('',#47131,#10328) ;
#7857 = LINE('',#47132,#10329) ;
#7858 = LINE('',#47134,#10330) ;
#7859 = LINE('',#47136,#10331) ;
#7860 = LINE('',#47137,#10332) ;
#7861 = LINE('',#47139,#10333) ;
#7862 = LINE('',#47140,#10334) ;
#7863 = LINE('',#47142,#10335) ;
#7864 = LINE('',#47144,#10336) ;
#7865 = LINE('',#47148,#10337) ;
#7866 = LINE('',#47149,#10338) ;
#7867 = LINE('',#47152,#10339) ;
#7868 = LINE('',#47153,#10340) ;
#7869 = LINE('',#47155,#10341) ;
#7870 = LINE('',#47159,#10342) ;
#7871 = LINE('',#47161,#10343) ;
#7872 = LINE('',#47162,#10344) ;
#7873 = LINE('',#47165,#10345) ;
#7874 = LINE('',#47166,#10346) ;
#7875 = LINE('',#47169,#10347) ;
#7876 = LINE('',#47170,#10348) ;
#7877 = LINE('',#47172,#10349) ;
#7878 = LINE('',#47179,#10350) ;
#7879 = LINE('',#47193,#10351) ;
#7880 = LINE('',#47199,#10352) ;
#7881 = LINE('',#47220,#10353) ;
#7882 = LINE('',#47252,#10354) ;
#7883 = LINE('',#47277,#10355) ;
#7884 = LINE('',#47283,#10356) ;
#7885 = LINE('',#47294,#10357) ;
#7886 = LINE('',#47299,#10358) ;
#7887 = LINE('',#47303,#10359) ;
#7888 = LINE('',#47309,#10360) ;
#7889 = LINE('',#47316,#10361) ;
#7890 = LINE('',#47333,#10362) ;
#7891 = LINE('',#47403,#10363) ;
#7892 = LINE('',#47441,#10364) ;
#7893 = LINE('',#47471,#10365) ;
#7894 = LINE('',#47481,#10366) ;
#7895 = LINE('',#47483,#10367) ;
#7896 = LINE('',#47484,#10368) ;
#7897 = LINE('',#47491,#10369) ;
#7898 = LINE('',#47498,#10370) ;
#7899 = LINE('',#47507,#10371) ;
#7900 = LINE('',#47516,#10372) ;
#7901 = LINE('',#47525,#10373) ;
#7902 = LINE('',#47569,#10374) ;
#7903 = LINE('',#47576,#10375) ;
#7904 = LINE('',#47582,#10376) ;
#7905 = LINE('',#47588,#10377) ;
#7906 = LINE('',#47627,#10378) ;
#7907 = LINE('',#47633,#10379) ;
#7908 = LINE('',#47637,#10380) ;
#7909 = LINE('',#48665,#10381) ;
#7910 = LINE('',#48670,#10382) ;
#7911 = LINE('',#48675,#10383) ;
#7912 = LINE('',#48680,#10384) ;
#7913 = LINE('',#48685,#10385) ;
#7914 = LINE('',#48690,#10386) ;
#7915 = LINE('',#48695,#10387) ;
#7916 = LINE('',#48700,#10388) ;
#7917 = LINE('',#48705,#10389) ;
#7918 = LINE('',#48710,#10390) ;
#7919 = LINE('',#48715,#10391) ;
#7920 = LINE('',#48720,#10392) ;
#7921 = LINE('',#48725,#10393) ;
#7922 = LINE('',#48730,#10394) ;
#7923 = LINE('',#48735,#10395) ;
#7924 = LINE('',#48740,#10396) ;
#7925 = LINE('',#48745,#10397) ;
#7926 = LINE('',#48750,#10398) ;
#7927 = LINE('',#48755,#10399) ;
#7928 = LINE('',#48760,#10400) ;
#7929 = LINE('',#48765,#10401) ;
#7930 = LINE('',#48770,#10402) ;
#7931 = LINE('',#48775,#10403) ;
#7932 = LINE('',#48780,#10404) ;
#7933 = LINE('',#48785,#10405) ;
#7934 = LINE('',#48790,#10406) ;
#7935 = LINE('',#48795,#10407) ;
#7936 = LINE('',#48800,#10408) ;
#7937 = LINE('',#48805,#10409) ;
#7938 = LINE('',#48810,#10410) ;
#7939 = LINE('',#48815,#10411) ;
#7940 = LINE('',#48820,#10412) ;
#7941 = LINE('',#48825,#10413) ;
#7942 = LINE('',#48830,#10414) ;
#7943 = LINE('',#48835,#10415) ;
#7944 = LINE('',#48840,#10416) ;
#7945 = LINE('',#48845,#10417) ;
#7946 = LINE('',#48850,#10418) ;
#7947 = LINE('',#48855,#10419) ;
#7948 = LINE('',#48860,#10420) ;
#7949 = LINE('',#48865,#10421) ;
#7950 = LINE('',#48870,#10422) ;
#7951 = LINE('',#48875,#10423) ;
#7952 = LINE('',#48880,#10424) ;
#7953 = LINE('',#48885,#10425) ;
#7954 = LINE('',#48890,#10426) ;
#7955 = LINE('',#48895,#10427) ;
#7956 = LINE('',#48900,#10428) ;
#7957 = LINE('',#48905,#10429) ;
#7958 = LINE('',#48910,#10430) ;
#7959 = LINE('',#48915,#10431) ;
#7960 = LINE('',#48920,#10432) ;
#7961 = LINE('',#48925,#10433) ;
#7962 = LINE('',#48930,#10434) ;
#7963 = LINE('',#48935,#10435) ;
#7964 = LINE('',#48940,#10436) ;
#7965 = LINE('',#48945,#10437) ;
#7966 = LINE('',#48950,#10438) ;
#7967 = LINE('',#48955,#10439) ;
#7968 = LINE('',#48960,#10440) ;
#7969 = LINE('',#48965,#10441) ;
#7970 = LINE('',#48970,#10442) ;
#7971 = LINE('',#48975,#10443) ;
#7972 = LINE('',#48980,#10444) ;
#7973 = LINE('',#48985,#10445) ;
#7974 = LINE('',#48990,#10446) ;
#7975 = LINE('',#48995,#10447) ;
#7976 = LINE('',#49000,#10448) ;
#7977 = LINE('',#49005,#10449) ;
#7978 = LINE('',#49010,#10450) ;
#7979 = LINE('',#49015,#10451) ;
#7980 = LINE('',#49020,#10452) ;
#7981 = LINE('',#49025,#10453) ;
#7982 = LINE('',#49030,#10454) ;
#7983 = LINE('',#49035,#10455) ;
#7984 = LINE('',#49040,#10456) ;
#7985 = LINE('',#49045,#10457) ;
#7986 = LINE('',#49050,#10458) ;
#7987 = LINE('',#49055,#10459) ;
#7988 = LINE('',#49060,#10460) ;
#7989 = LINE('',#49065,#10461) ;
#7990 = LINE('',#49070,#10462) ;
#7991 = LINE('',#49075,#10463) ;
#7992 = LINE('',#49080,#10464) ;
#7993 = LINE('',#49085,#10465) ;
#7994 = LINE('',#49090,#10466) ;
#7995 = LINE('',#49095,#10467) ;
#7996 = LINE('',#49100,#10468) ;
#7997 = LINE('',#49105,#10469) ;
#7998 = LINE('',#49110,#10470) ;
#7999 = LINE('',#49115,#10471) ;
#8000 = LINE('',#49120,#10472) ;
#8001 = LINE('',#49125,#10473) ;
#8002 = LINE('',#49130,#10474) ;
#8003 = LINE('',#49135,#10475) ;
#8004 = LINE('',#49140,#10476) ;
#8005 = LINE('',#49145,#10477) ;
#8006 = LINE('',#49150,#10478) ;
#8007 = LINE('',#49155,#10479) ;
#8008 = LINE('',#49160,#10480) ;
#8009 = LINE('',#49165,#10481) ;
#8010 = LINE('',#49170,#10482) ;
#8011 = LINE('',#49175,#10483) ;
#8012 = LINE('',#49180,#10484) ;
#8013 = LINE('',#49185,#10485) ;
#8014 = LINE('',#49190,#10486) ;
#8015 = LINE('',#49195,#10487) ;
#8016 = LINE('',#49200,#10488) ;
#8017 = LINE('',#49205,#10489) ;
#8018 = LINE('',#49210,#10490) ;
#8019 = LINE('',#49215,#10491) ;
#8020 = LINE('',#49220,#10492) ;
#8021 = LINE('',#49225,#10493) ;
#8022 = LINE('',#49230,#10494) ;
#8023 = LINE('',#49235,#10495) ;
#8024 = LINE('',#49240,#10496) ;
#8025 = LINE('',#49245,#10497) ;
#8026 = LINE('',#49250,#10498) ;
#8027 = LINE('',#49255,#10499) ;
#8028 = LINE('',#49260,#10500) ;
#8029 = LINE('',#49265,#10501) ;
#8030 = LINE('',#49270,#10502) ;
#8031 = LINE('',#49275,#10503) ;
#8032 = LINE('',#49280,#10504) ;
#8033 = LINE('',#49285,#10505) ;
#8034 = LINE('',#49290,#10506) ;
#8035 = LINE('',#49297,#10507) ;
#8036 = LINE('',#49318,#10508) ;
#8037 = LINE('',#49345,#10509) ;
#8038 = LINE('',#49351,#10510) ;
#8039 = LINE('',#49435,#10511) ;
#8040 = LINE('',#49486,#10512) ;
#8041 = LINE('',#49492,#10513) ;
#8042 = LINE('',#49496,#10514) ;
#8043 = LINE('',#49509,#10515) ;
#8044 = LINE('',#49515,#10516) ;
#8045 = LINE('',#49517,#10517) ;
#8046 = LINE('',#49519,#10518) ;
#8047 = LINE('',#49520,#10519) ;
#8048 = LINE('',#49524,#10520) ;
#8049 = LINE('',#49525,#10521) ;
#8050 = LINE('',#49527,#10522) ;
#8051 = LINE('',#49528,#10523) ;
#8052 = LINE('',#49532,#10524) ;
#8053 = LINE('',#49534,#10525) ;
#8054 = LINE('',#49535,#10526) ;
#8055 = LINE('',#49536,#10527) ;
#8056 = LINE('',#49538,#10528) ;
#8057 = LINE('',#49539,#10529) ;
#8058 = LINE('',#49542,#10530) ;
#8059 = LINE('',#49550,#10531) ;
#8060 = LINE('',#49554,#10532) ;
#8061 = LINE('',#49575,#10533) ;
#8062 = LINE('',#49636,#10534) ;
#8063 = LINE('',#49678,#10535) ;
#8064 = LINE('',#49720,#10536) ;
#8065 = LINE('',#49724,#10537) ;
#8066 = LINE('',#49726,#10538) ;
#8067 = LINE('',#49733,#10539) ;
#8068 = LINE('',#49735,#10540) ;
#8069 = LINE('',#49737,#10541) ;
#8070 = LINE('',#49741,#10542) ;
#8071 = LINE('',#49743,#10543) ;
#8072 = LINE('',#49745,#10544) ;
#8073 = LINE('',#49749,#10545) ;
#8074 = LINE('',#49760,#10546) ;
#8075 = LINE('',#49766,#10547) ;
#8076 = LINE('',#49772,#10548) ;
#8077 = LINE('',#49780,#10549) ;
#8078 = LINE('',#49784,#10550) ;
#8079 = LINE('',#49788,#10551) ;
#8080 = LINE('',#49790,#10552) ;
#8081 = LINE('',#49792,#10553) ;
#8082 = LINE('',#49794,#10554) ;
#8083 = LINE('',#49795,#10555) ;
#8084 = LINE('',#49798,#10556) ;
#8085 = LINE('',#49799,#10557) ;
#8086 = LINE('',#49802,#10558) ;
#8087 = LINE('',#49803,#10559) ;
#8088 = LINE('',#49807,#10560) ;
#8089 = LINE('',#49808,#10561) ;
#8090 = LINE('',#49809,#10562) ;
#8091 = LINE('',#49811,#10563) ;
#8092 = LINE('',#49813,#10564) ;
#8093 = LINE('',#49818,#10565) ;
#8094 = LINE('',#49820,#10566) ;
#8095 = LINE('',#49822,#10567) ;
#8096 = LINE('',#49823,#10568) ;
#8097 = LINE('',#49827,#10569) ;
#8098 = LINE('',#49829,#10570) ;
#8099 = LINE('',#49831,#10571) ;
#8100 = LINE('',#49832,#10572) ;
#8101 = LINE('',#49834,#10573) ;
#8102 = LINE('',#49835,#10574) ;
#8103 = LINE('',#49837,#10575) ;
#8104 = LINE('',#49839,#10576) ;
#8105 = LINE('',#49845,#10577) ;
#8106 = LINE('',#49847,#10578) ;
#8107 = LINE('',#49849,#10579) ;
#8108 = LINE('',#49851,#10580) ;
#8109 = LINE('',#49853,#10581) ;
#8110 = LINE('',#49854,#10582) ;
#8111 = LINE('',#49859,#10583) ;
#8112 = LINE('',#49860,#10584) ;
#8113 = LINE('',#49863,#10585) ;
#8114 = LINE('',#49864,#10586) ;
#8115 = LINE('',#49867,#10587) ;
#8116 = LINE('',#49869,#10588) ;
#8117 = LINE('',#49870,#10589) ;
#8118 = LINE('',#49872,#10590) ;
#8119 = LINE('',#49875,#10591) ;
#8120 = LINE('',#49876,#10592) ;
#8121 = LINE('',#49885,#10593) ;
#8122 = LINE('',#49890,#10594) ;
#8123 = LINE('',#49904,#10595) ;
#8124 = LINE('',#49910,#10596) ;
#8125 = LINE('',#49912,#10597) ;
#8126 = LINE('',#49914,#10598) ;
#8127 = LINE('',#49915,#10599) ;
#8128 = LINE('',#49919,#10600) ;
#8129 = LINE('',#49921,#10601) ;
#8130 = LINE('',#49923,#10602) ;
#8131 = LINE('',#49924,#10603) ;
#8132 = LINE('',#49927,#10604) ;
#8133 = LINE('',#49928,#10605) ;
#8134 = LINE('',#49930,#10606) ;
#8135 = LINE('',#49931,#10607) ;
#8136 = LINE('',#49934,#10608) ;
#8137 = LINE('',#49935,#10609) ;
#8138 = LINE('',#49938,#10610) ;
#8139 = LINE('',#49939,#10611) ;
#8140 = LINE('',#49941,#10612) ;
#8141 = LINE('',#49943,#10613) ;
#8142 = LINE('',#49950,#10614) ;
#8143 = LINE('',#49955,#10615) ;
#8144 = LINE('',#49957,#10616) ;
#8145 = LINE('',#49959,#10617) ;
#8146 = LINE('',#49960,#10618) ;
#8147 = LINE('',#49964,#10619) ;
#8148 = LINE('',#49966,#10620) ;
#8149 = LINE('',#49968,#10621) ;
#8150 = LINE('',#49969,#10622) ;
#8151 = LINE('',#49972,#10623) ;
#8152 = LINE('',#49973,#10624) ;
#8153 = LINE('',#49975,#10625) ;
#8154 = LINE('',#49976,#10626) ;
#8155 = LINE('',#49979,#10627) ;
#8156 = LINE('',#49980,#10628) ;
#8157 = LINE('',#49983,#10629) ;
#8158 = LINE('',#49984,#10630) ;
#8159 = LINE('',#49986,#10631) ;
#8160 = LINE('',#49988,#10632) ;
#8161 = LINE('',#49995,#10633) ;
#8162 = LINE('',#50001,#10634) ;
#8163 = LINE('',#50003,#10635) ;
#8164 = LINE('',#50005,#10636) ;
#8165 = LINE('',#50006,#10637) ;
#8166 = LINE('',#50010,#10638) ;
#8167 = LINE('',#50012,#10639) ;
#8168 = LINE('',#50014,#10640) ;
#8169 = LINE('',#50015,#10641) ;
#8170 = LINE('',#50018,#10642) ;
#8171 = LINE('',#50019,#10643) ;
#8172 = LINE('',#50021,#10644) ;
#8173 = LINE('',#50022,#10645) ;
#8174 = LINE('',#50025,#10646) ;
#8175 = LINE('',#50026,#10647) ;
#8176 = LINE('',#50029,#10648) ;
#8177 = LINE('',#50030,#10649) ;
#8178 = LINE('',#50032,#10650) ;
#8179 = LINE('',#50034,#10651) ;
#8180 = LINE('',#50041,#10652) ;
#8181 = LINE('',#50046,#10653) ;
#8182 = LINE('',#50048,#10654) ;
#8183 = LINE('',#50050,#10655) ;
#8184 = LINE('',#50051,#10656) ;
#8185 = LINE('',#50055,#10657) ;
#8186 = LINE('',#50057,#10658) ;
#8187 = LINE('',#50059,#10659) ;
#8188 = LINE('',#50060,#10660) ;
#8189 = LINE('',#50063,#10661) ;
#8190 = LINE('',#50064,#10662) ;
#8191 = LINE('',#50066,#10663) ;
#8192 = LINE('',#50067,#10664) ;
#8193 = LINE('',#50070,#10665) ;
#8194 = LINE('',#50071,#10666) ;
#8195 = LINE('',#50074,#10667) ;
#8196 = LINE('',#50075,#10668) ;
#8197 = LINE('',#50077,#10669) ;
#8198 = LINE('',#50079,#10670) ;
#8199 = LINE('',#50090,#10671) ;
#8200 = LINE('',#50094,#10672) ;
#8201 = LINE('',#50106,#10673) ;
#8202 = LINE('',#50110,#10674) ;
#8203 = LINE('',#50146,#10675) ;
#8204 = LINE('',#50234,#10676) ;
#8205 = LINE('',#50239,#10677) ;
#8206 = LINE('',#50244,#10678) ;
#8207 = LINE('',#50248,#10679) ;
#8208 = LINE('',#50251,#10680) ;
#8209 = LINE('',#50254,#10681) ;
#8210 = LINE('',#50257,#10682) ;
#8211 = LINE('',#50260,#10683) ;
#8212 = LINE('',#50264,#10684) ;
#8213 = LINE('',#50295,#10685) ;
#8214 = LINE('',#50299,#10686) ;
#8215 = LINE('',#50304,#10687) ;
#8216 = VECTOR('',#32401,0.62) ;
#8217 = VECTOR('',#32406,1.) ;
#8218 = VECTOR('',#32407,1.) ;
#8219 = VECTOR('',#32408,1.) ;
#8220 = VECTOR('',#32409,1.) ;
#8221 = VECTOR('',#32410,1.) ;
#8222 = VECTOR('',#32411,1.) ;
#8223 = VECTOR('',#32412,1.) ;
#8224 = VECTOR('',#32413,1.) ;
#8225 = VECTOR('',#32416,1.) ;
#8226 = VECTOR('',#32417,1.) ;
#8227 = VECTOR('',#32418,1.) ;
#8228 = VECTOR('',#32421,1.) ;
#8229 = VECTOR('',#32422,1.) ;
#8230 = VECTOR('',#32423,1.) ;
#8231 = VECTOR('',#32426,1.) ;
#8232 = VECTOR('',#32427,1.) ;
#8233 = VECTOR('',#32432,1.) ;
#8234 = VECTOR('',#32435,1.) ;
#8235 = VECTOR('',#32436,1.) ;
#8236 = VECTOR('',#32439,1.) ;
#8237 = VECTOR('',#32440,1.) ;
#8238 = VECTOR('',#32441,1.) ;
#8239 = VECTOR('',#32448,55.) ;
#8240 = VECTOR('',#32451,1.) ;
#8241 = VECTOR('',#32454,1.) ;
#8242 = VECTOR('',#32463,0.62) ;
#8243 = VECTOR('',#32468,1.) ;
#8244 = VECTOR('',#32469,1.) ;
#8245 = VECTOR('',#32470,1.) ;
#8246 = VECTOR('',#32471,1.) ;
#8247 = VECTOR('',#32472,1.) ;
#8248 = VECTOR('',#32473,1.) ;
#8249 = VECTOR('',#32474,1.) ;
#8250 = VECTOR('',#32477,1.) ;
#8251 = VECTOR('',#32478,1.) ;
#8252 = VECTOR('',#32479,1.) ;
#8253 = VECTOR('',#32482,1.) ;
#8254 = VECTOR('',#32483,1.) ;
#8255 = VECTOR('',#32484,1.) ;
#8256 = VECTOR('',#32487,1.) ;
#8257 = VECTOR('',#32488,1.) ;
#8258 = VECTOR('',#32491,1.) ;
#8259 = VECTOR('',#32494,1.) ;
#8260 = VECTOR('',#32495,1.) ;
#8261 = VECTOR('',#32498,1.) ;
#8262 = VECTOR('',#32499,1.) ;
#8263 = VECTOR('',#32506,1.) ;
#8264 = VECTOR('',#32507,1.) ;
#8265 = VECTOR('',#32508,1.) ;
#8266 = VECTOR('',#32511,1.) ;
#8267 = VECTOR('',#32512,1.) ;
#8268 = VECTOR('',#32515,1.) ;
#8269 = VECTOR('',#32516,1.) ;
#8270 = VECTOR('',#32519,1.) ;
#8271 = VECTOR('',#32520,1.) ;
#8272 = VECTOR('',#32521,1.) ;
#8273 = VECTOR('',#32526,1.) ;
#8274 = VECTOR('',#32531,1.) ;
#8275 = VECTOR('',#32532,1.) ;
#8276 = VECTOR('',#32537,1.) ;
#8277 = VECTOR('',#32538,1.) ;
#8278 = VECTOR('',#32541,1.) ;
#8279 = VECTOR('',#32550,1.) ;
#8280 = VECTOR('',#32551,1.) ;
#8281 = VECTOR('',#32552,1.) ;
#8282 = VECTOR('',#32555,1.) ;
#8283 = VECTOR('',#32556,1.) ;
#8284 = VECTOR('',#32559,1.) ;
#8285 = VECTOR('',#32560,1.) ;
#8286 = VECTOR('',#32563,1.) ;
#8287 = VECTOR('',#32564,1.) ;
#8288 = VECTOR('',#32565,1.) ;
#8289 = VECTOR('',#32570,1.) ;
#8290 = VECTOR('',#32575,1.) ;
#8291 = VECTOR('',#32576,1.) ;
#8292 = VECTOR('',#32581,1.) ;
#8293 = VECTOR('',#32582,1.) ;
#8294 = VECTOR('',#32585,1.) ;
#8295 = VECTOR('',#32594,1.) ;
#8296 = VECTOR('',#32595,1.) ;
#8297 = VECTOR('',#32596,1.) ;
#8298 = VECTOR('',#32599,1.) ;
#8299 = VECTOR('',#32600,1.) ;
#8300 = VECTOR('',#32603,1.) ;
#8301 = VECTOR('',#32604,1.) ;
#8302 = VECTOR('',#32607,1.) ;
#8303 = VECTOR('',#32608,1.) ;
#8304 = VECTOR('',#32609,1.) ;
#8305 = VECTOR('',#32614,1.) ;
#8306 = VECTOR('',#32619,1.) ;
#8307 = VECTOR('',#32620,1.) ;
#8308 = VECTOR('',#32625,1.) ;
#8309 = VECTOR('',#32626,1.) ;
#8310 = VECTOR('',#32629,1.) ;
#8311 = VECTOR('',#32638,1.) ;
#8312 = VECTOR('',#32639,1.) ;
#8313 = VECTOR('',#32640,1.) ;
#8314 = VECTOR('',#32643,1.) ;
#8315 = VECTOR('',#32644,1.) ;
#8316 = VECTOR('',#32647,1.) ;
#8317 = VECTOR('',#32648,1.) ;
#8318 = VECTOR('',#32651,1.) ;
#8319 = VECTOR('',#32652,1.) ;
#8320 = VECTOR('',#32653,1.) ;
#8321 = VECTOR('',#32658,1.) ;
#8322 = VECTOR('',#32663,1.) ;
#8323 = VECTOR('',#32664,1.) ;
#8324 = VECTOR('',#32669,1.) ;
#8325 = VECTOR('',#32670,1.) ;
#8326 = VECTOR('',#32673,1.) ;
#8327 = VECTOR('',#32682,53.4) ;
#8328 = VECTOR('',#32689,53.4) ;
#8329 = VECTOR('',#32700,32.15) ;
#8330 = VECTOR('',#32703,32.75) ;
#8331 = VECTOR('',#32712,1.) ;
#8332 = VECTOR('',#32713,1.) ;
#8333 = VECTOR('',#32714,1.) ;
#8334 = VECTOR('',#32715,1.) ;
#8335 = VECTOR('',#32718,1.) ;
#8336 = VECTOR('',#32719,1.) ;
#8337 = VECTOR('',#32720,1.) ;
#8338 = VECTOR('',#32723,1.) ;
#8339 = VECTOR('',#32724,1.) ;
#8340 = VECTOR('',#32725,1.) ;
#8341 = VECTOR('',#32728,1.) ;
#8342 = VECTOR('',#32729,1.) ;
#8343 = VECTOR('',#32730,1.) ;
#8344 = VECTOR('',#32731,1.) ;
#8345 = VECTOR('',#32732,1.) ;
#8346 = VECTOR('',#32735,1.) ;
#8347 = VECTOR('',#32736,1.) ;
#8348 = VECTOR('',#32737,1.) ;
#8349 = VECTOR('',#32738,1.) ;
#8350 = VECTOR('',#32739,1.) ;
#8351 = VECTOR('',#32742,1.) ;
#8352 = VECTOR('',#32743,1.) ;
#8353 = VECTOR('',#32746,1.) ;
#8354 = VECTOR('',#32749,1.) ;
#8355 = VECTOR('',#32754,55.05) ;
#8356 = VECTOR('',#32765,55.5) ;
#8357 = VECTOR('',#32774,1.) ;
#8358 = VECTOR('',#32775,1.) ;
#8359 = VECTOR('',#32776,1.) ;
#8360 = VECTOR('',#32777,1.) ;
#8361 = VECTOR('',#32780,1.) ;
#8362 = VECTOR('',#32781,1.) ;
#8363 = VECTOR('',#32782,1.) ;
#8364 = VECTOR('',#32783,1.) ;
#8365 = VECTOR('',#32786,1.) ;
#8366 = VECTOR('',#32787,1.) ;
#8367 = VECTOR('',#32802,1.) ;
#8368 = VECTOR('',#32803,1.) ;
#8369 = VECTOR('',#32804,1.) ;
#8370 = VECTOR('',#32805,1.) ;
#8371 = VECTOR('',#32808,1.) ;
#8372 = VECTOR('',#32809,1.) ;
#8373 = VECTOR('',#32810,1.) ;
#8374 = VECTOR('',#32811,1.) ;
#8375 = VECTOR('',#32814,1.) ;
#8376 = VECTOR('',#32815,1.) ;
#8377 = VECTOR('',#32816,1.) ;
#8378 = VECTOR('',#32817,1.) ;
#8379 = VECTOR('',#32820,1.) ;
#8380 = VECTOR('',#32821,1.) ;
#8381 = VECTOR('',#32822,1.) ;
#8382 = VECTOR('',#32823,1.) ;
#8383 = VECTOR('',#32826,1.) ;
#8384 = VECTOR('',#32827,1.) ;
#8385 = VECTOR('',#32828,1.) ;
#8386 = VECTOR('',#32829,1.) ;
#8387 = VECTOR('',#32832,1.) ;
#8388 = VECTOR('',#32833,1.) ;
#8389 = VECTOR('',#32834,1.) ;
#8390 = VECTOR('',#32835,1.) ;
#8391 = VECTOR('',#32838,1.) ;
#8392 = VECTOR('',#32839,1.) ;
#8393 = VECTOR('',#32840,1.) ;
#8394 = VECTOR('',#32841,1.) ;
#8395 = VECTOR('',#32844,1.) ;
#8396 = VECTOR('',#32845,1.) ;
#8397 = VECTOR('',#32846,1.) ;
#8398 = VECTOR('',#32847,1.) ;
#8399 = VECTOR('',#32850,1.) ;
#8400 = VECTOR('',#32851,1.) ;
#8401 = VECTOR('',#32852,1.) ;
#8402 = VECTOR('',#32853,1.) ;
#8403 = VECTOR('',#32856,1.) ;
#8404 = VECTOR('',#32857,1.) ;
#8405 = VECTOR('',#32858,1.) ;
#8406 = VECTOR('',#32859,1.) ;
#8407 = VECTOR('',#32862,1.) ;
#8408 = VECTOR('',#32863,1.) ;
#8409 = VECTOR('',#32864,1.) ;
#8410 = VECTOR('',#32865,1.) ;
#8411 = VECTOR('',#32868,1.) ;
#8412 = VECTOR('',#32869,1.) ;
#8413 = VECTOR('',#32870,1.) ;
#8414 = VECTOR('',#32871,1.) ;
#8415 = VECTOR('',#32874,1.) ;
#8416 = VECTOR('',#32875,1.) ;
#8417 = VECTOR('',#32876,1.) ;
#8418 = VECTOR('',#32879,1.) ;
#8419 = VECTOR('',#32880,1.) ;
#8420 = VECTOR('',#32881,1.) ;
#8421 = VECTOR('',#32886,1.) ;
#8422 = VECTOR('',#32893,1.) ;
#8423 = VECTOR('',#32900,1.) ;
#8424 = VECTOR('',#32905,1.) ;
#8425 = VECTOR('',#32906,1.) ;
#8426 = VECTOR('',#32907,1.) ;
#8427 = VECTOR('',#32910,1.) ;
#8428 = VECTOR('',#32911,1.) ;
#8429 = VECTOR('',#32912,1.) ;
#8430 = VECTOR('',#32915,1.) ;
#8431 = VECTOR('',#32916,1.) ;
#8432 = VECTOR('',#32917,1.) ;
#8433 = VECTOR('',#32920,1.) ;
#8434 = VECTOR('',#32921,1.) ;
#8435 = VECTOR('',#32922,1.) ;
#8436 = VECTOR('',#32925,1.) ;
#8437 = VECTOR('',#32926,1.) ;
#8438 = VECTOR('',#32927,1.) ;
#8439 = VECTOR('',#32930,1.) ;
#8440 = VECTOR('',#32931,1.) ;
#8441 = VECTOR('',#32932,1.) ;
#8442 = VECTOR('',#32935,1.) ;
#8443 = VECTOR('',#32936,1.) ;
#8444 = VECTOR('',#32937,1.) ;
#8445 = VECTOR('',#32940,1.) ;
#8446 = VECTOR('',#32941,1.) ;
#8447 = VECTOR('',#32942,1.) ;
#8448 = VECTOR('',#32945,1.) ;
#8449 = VECTOR('',#32946,1.) ;
#8450 = VECTOR('',#32949,1.) ;
#8451 = VECTOR('',#32950,1.) ;
#8452 = VECTOR('',#32953,1.) ;
#8453 = VECTOR('',#32954,1.) ;
#8454 = VECTOR('',#32957,1.) ;
#8455 = VECTOR('',#32958,1.) ;
#8456 = VECTOR('',#32959,1.) ;
#8457 = VECTOR('',#32962,1.) ;
#8458 = VECTOR('',#32963,1.) ;
#8459 = VECTOR('',#32966,1.) ;
#8460 = VECTOR('',#32967,1.) ;
#8461 = VECTOR('',#32970,1.) ;
#8462 = VECTOR('',#32971,1.) ;
#8463 = VECTOR('',#32974,1.) ;
#8464 = VECTOR('',#32975,1.) ;
#8465 = VECTOR('',#32978,1.) ;
#8466 = VECTOR('',#32979,1.) ;
#8467 = VECTOR('',#32982,1.) ;
#8468 = VECTOR('',#32983,1.) ;
#8469 = VECTOR('',#32986,1.) ;
#8470 = VECTOR('',#32987,1.) ;
#8471 = VECTOR('',#32988,1.) ;
#8472 = VECTOR('',#32991,1.) ;
#8473 = VECTOR('',#32992,1.) ;
#8474 = VECTOR('',#32995,1.) ;
#8475 = VECTOR('',#32996,1.) ;
#8476 = VECTOR('',#32999,1.) ;
#8477 = VECTOR('',#33000,1.) ;
#8478 = VECTOR('',#33003,1.) ;
#8479 = VECTOR('',#33004,1.) ;
#8480 = VECTOR('',#33007,1.) ;
#8481 = VECTOR('',#33008,1.) ;
#8482 = VECTOR('',#33011,1.) ;
#8483 = VECTOR('',#33012,1.) ;
#8484 = VECTOR('',#33015,1.) ;
#8485 = VECTOR('',#33016,1.) ;
#8486 = VECTOR('',#33017,1.) ;
#8487 = VECTOR('',#33020,1.) ;
#8488 = VECTOR('',#33021,1.) ;
#8489 = VECTOR('',#33024,1.) ;
#8490 = VECTOR('',#33025,1.) ;
#8491 = VECTOR('',#33028,1.) ;
#8492 = VECTOR('',#33029,1.) ;
#8493 = VECTOR('',#33034,1.) ;
#8494 = VECTOR('',#33035,1.) ;
#8495 = VECTOR('',#33038,1.) ;
#8496 = VECTOR('',#33039,1.) ;
#8497 = VECTOR('',#33042,1.) ;
#8498 = VECTOR('',#33043,1.) ;
#8499 = VECTOR('',#33044,1.) ;
#8500 = VECTOR('',#33047,1.) ;
#8501 = VECTOR('',#33048,1.) ;
#8502 = VECTOR('',#33051,1.) ;
#8503 = VECTOR('',#33052,1.) ;
#8504 = VECTOR('',#33053,1.) ;
#8505 = VECTOR('',#33056,1.) ;
#8506 = VECTOR('',#33059,1.) ;
#8507 = VECTOR('',#33062,1.) ;
#8508 = VECTOR('',#33063,1.) ;
#8509 = VECTOR('',#33064,1.) ;
#8510 = VECTOR('',#33065,1.) ;
#8511 = VECTOR('',#33066,1.) ;
#8512 = VECTOR('',#33067,1.) ;
#8513 = VECTOR('',#33068,1.) ;
#8514 = VECTOR('',#33069,1.) ;
#8515 = VECTOR('',#33070,1.) ;
#8516 = VECTOR('',#33071,1.) ;
#8517 = VECTOR('',#33074,1.) ;
#8518 = VECTOR('',#33077,1.) ;
#8519 = VECTOR('',#33078,1.) ;
#8520 = VECTOR('',#33079,1.) ;
#8521 = VECTOR('',#33080,1.) ;
#8522 = VECTOR('',#33081,1.) ;
#8523 = VECTOR('',#33082,1.) ;
#8524 = VECTOR('',#33083,1.) ;
#8525 = VECTOR('',#33084,1.) ;
#8526 = VECTOR('',#33085,1.) ;
#8527 = VECTOR('',#33086,1.) ;
#8528 = VECTOR('',#33087,1.) ;
#8529 = VECTOR('',#33088,1.) ;
#8530 = VECTOR('',#33089,1.) ;
#8531 = VECTOR('',#33090,1.) ;
#8532 = VECTOR('',#33091,1.) ;
#8533 = VECTOR('',#33092,1.) ;
#8534 = VECTOR('',#33093,1.) ;
#8535 = VECTOR('',#33094,1.) ;
#8536 = VECTOR('',#33095,1.) ;
#8537 = VECTOR('',#33098,1.) ;
#8538 = VECTOR('',#33099,1.) ;
#8539 = VECTOR('',#33100,1.) ;
#8540 = VECTOR('',#33103,1.) ;
#8541 = VECTOR('',#33104,1.) ;
#8542 = VECTOR('',#33105,1.) ;
#8543 = VECTOR('',#33106,1.) ;
#8544 = VECTOR('',#33109,1.) ;
#8545 = VECTOR('',#33110,1.) ;
#8546 = VECTOR('',#33113,1.) ;
#8547 = VECTOR('',#33116,1.) ;
#8548 = VECTOR('',#33117,1.) ;
#8549 = VECTOR('',#33118,1.) ;
#8550 = VECTOR('',#33119,1.) ;
#8551 = VECTOR('',#33120,1.) ;
#8552 = VECTOR('',#33121,1.) ;
#8553 = VECTOR('',#33122,1.) ;
#8554 = VECTOR('',#33123,1.) ;
#8555 = VECTOR('',#33124,1.) ;
#8556 = VECTOR('',#33125,1.) ;
#8557 = VECTOR('',#33126,1.) ;
#8558 = VECTOR('',#33127,1.) ;
#8559 = VECTOR('',#33128,1.) ;
#8560 = VECTOR('',#33129,1.) ;
#8561 = VECTOR('',#33130,1.) ;
#8562 = VECTOR('',#33131,1.) ;
#8563 = VECTOR('',#33132,1.) ;
#8564 = VECTOR('',#33133,1.) ;
#8565 = VECTOR('',#33134,1.) ;
#8566 = VECTOR('',#33135,1.) ;
#8567 = VECTOR('',#33136,1.) ;
#8568 = VECTOR('',#33137,1.) ;
#8569 = VECTOR('',#33138,1.) ;
#8570 = VECTOR('',#33139,1.) ;
#8571 = VECTOR('',#33140,1.) ;
#8572 = VECTOR('',#33143,1.) ;
#8573 = VECTOR('',#33144,1.) ;
#8574 = VECTOR('',#33145,1.) ;
#8575 = VECTOR('',#33146,1.) ;
#8576 = VECTOR('',#33147,1.) ;
#8577 = VECTOR('',#33148,1.) ;
#8578 = VECTOR('',#33149,1.) ;
#8579 = VECTOR('',#33150,1.) ;
#8580 = VECTOR('',#33151,1.) ;
#8581 = VECTOR('',#33152,1.) ;
#8582 = VECTOR('',#33155,1.) ;
#8583 = VECTOR('',#33156,1.) ;
#8584 = VECTOR('',#33157,1.) ;
#8585 = VECTOR('',#33160,1.) ;
#8586 = VECTOR('',#33161,1.) ;
#8587 = VECTOR('',#33162,1.) ;
#8588 = VECTOR('',#33165,1.) ;
#8589 = VECTOR('',#33166,1.) ;
#8590 = VECTOR('',#33167,1.) ;
#8591 = VECTOR('',#33168,1.) ;
#8592 = VECTOR('',#33169,1.) ;
#8593 = VECTOR('',#33170,1.) ;
#8594 = VECTOR('',#33173,1.) ;
#8595 = VECTOR('',#33174,1.) ;
#8596 = VECTOR('',#33175,1.) ;
#8597 = VECTOR('',#33178,1.) ;
#8598 = VECTOR('',#33179,1.) ;
#8599 = VECTOR('',#33180,1.) ;
#8600 = VECTOR('',#33181,1.) ;
#8601 = VECTOR('',#33182,1.) ;
#8602 = VECTOR('',#33183,1.) ;
#8603 = VECTOR('',#33184,1.) ;
#8604 = VECTOR('',#33185,1.) ;
#8605 = VECTOR('',#33186,1.) ;
#8606 = VECTOR('',#33187,1.) ;
#8607 = VECTOR('',#33188,1.) ;
#8608 = VECTOR('',#33189,1.) ;
#8609 = VECTOR('',#33190,1.) ;
#8610 = VECTOR('',#33191,1.) ;
#8611 = VECTOR('',#33192,1.) ;
#8612 = VECTOR('',#33193,1.) ;
#8613 = VECTOR('',#33194,1.) ;
#8614 = VECTOR('',#33195,1.) ;
#8615 = VECTOR('',#33196,1.) ;
#8616 = VECTOR('',#33197,1.) ;
#8617 = VECTOR('',#33198,1.) ;
#8618 = VECTOR('',#33199,1.) ;
#8619 = VECTOR('',#33200,1.) ;
#8620 = VECTOR('',#33201,1.) ;
#8621 = VECTOR('',#33202,1.) ;
#8622 = VECTOR('',#33203,1.) ;
#8623 = VECTOR('',#33204,1.) ;
#8624 = VECTOR('',#33207,1.) ;
#8625 = VECTOR('',#33208,1.) ;
#8626 = VECTOR('',#33209,1.) ;
#8627 = VECTOR('',#33210,1.) ;
#8628 = VECTOR('',#33213,1.) ;
#8629 = VECTOR('',#33214,1.) ;
#8630 = VECTOR('',#33215,1.) ;
#8631 = VECTOR('',#33216,1.) ;
#8632 = VECTOR('',#33217,1.) ;
#8633 = VECTOR('',#33218,1.) ;
#8634 = VECTOR('',#33219,1.) ;
#8635 = VECTOR('',#33220,1.) ;
#8636 = VECTOR('',#33221,1.) ;
#8637 = VECTOR('',#33222,1.) ;
#8638 = VECTOR('',#33223,1.) ;
#8639 = VECTOR('',#33224,1.) ;
#8640 = VECTOR('',#33225,1.) ;
#8641 = VECTOR('',#33226,1.) ;
#8642 = VECTOR('',#33227,1.) ;
#8643 = VECTOR('',#33228,1.) ;
#8644 = VECTOR('',#33229,1.) ;
#8645 = VECTOR('',#33230,1.) ;
#8646 = VECTOR('',#33231,1.) ;
#8647 = VECTOR('',#33232,1.) ;
#8648 = VECTOR('',#33233,1.) ;
#8649 = VECTOR('',#33234,1.) ;
#8650 = VECTOR('',#33235,1.) ;
#8651 = VECTOR('',#33236,1.) ;
#8652 = VECTOR('',#33237,1.) ;
#8653 = VECTOR('',#33238,1.) ;
#8654 = VECTOR('',#33239,1.) ;
#8655 = VECTOR('',#33240,1.) ;
#8656 = VECTOR('',#33241,1.) ;
#8657 = VECTOR('',#33242,1.) ;
#8658 = VECTOR('',#33243,1.) ;
#8659 = VECTOR('',#33244,1.) ;
#8660 = VECTOR('',#33245,1.) ;
#8661 = VECTOR('',#33246,1.) ;
#8662 = VECTOR('',#33247,1.) ;
#8663 = VECTOR('',#33248,1.) ;
#8664 = VECTOR('',#33249,1.) ;
#8665 = VECTOR('',#33250,1.) ;
#8666 = VECTOR('',#33251,1.) ;
#8667 = VECTOR('',#33254,1.) ;
#8668 = VECTOR('',#33255,1.) ;
#8669 = VECTOR('',#33256,1.) ;
#8670 = VECTOR('',#33261,1.) ;
#8671 = VECTOR('',#33264,1.) ;
#8672 = VECTOR('',#33265,1.) ;
#8673 = VECTOR('',#33268,1.) ;
#8674 = VECTOR('',#33269,1.) ;
#8675 = VECTOR('',#33272,1.) ;
#8676 = VECTOR('',#33273,1.) ;
#8677 = VECTOR('',#33274,1.) ;
#8678 = VECTOR('',#33277,1.) ;
#8679 = VECTOR('',#33278,1.) ;
#8680 = VECTOR('',#33281,1.) ;
#8681 = VECTOR('',#33282,1.) ;
#8682 = VECTOR('',#33287,1.) ;
#8683 = VECTOR('',#33288,1.) ;
#8684 = VECTOR('',#33291,1.) ;
#8685 = VECTOR('',#33292,1.) ;
#8686 = VECTOR('',#33295,1.) ;
#8687 = VECTOR('',#33296,1.) ;
#8688 = VECTOR('',#33299,1.) ;
#8689 = VECTOR('',#33300,1.) ;
#8690 = VECTOR('',#33301,1.) ;
#8691 = VECTOR('',#33304,1.) ;
#8692 = VECTOR('',#33305,1.) ;
#8693 = VECTOR('',#33308,1.) ;
#8694 = VECTOR('',#33309,1.) ;
#8695 = VECTOR('',#33312,1.) ;
#8696 = VECTOR('',#33313,1.) ;
#8697 = VECTOR('',#33316,1.) ;
#8698 = VECTOR('',#33317,1.) ;
#8699 = VECTOR('',#33320,1.) ;
#8700 = VECTOR('',#33321,1.) ;
#8701 = VECTOR('',#33324,1.) ;
#8702 = VECTOR('',#33325,1.) ;
#8703 = VECTOR('',#33328,1.) ;
#8704 = VECTOR('',#33329,1.) ;
#8705 = VECTOR('',#33330,1.) ;
#8706 = VECTOR('',#33333,1.) ;
#8707 = VECTOR('',#33334,1.) ;
#8708 = VECTOR('',#33337,1.) ;
#8709 = VECTOR('',#33338,1.) ;
#8710 = VECTOR('',#33341,1.) ;
#8711 = VECTOR('',#33342,1.) ;
#8712 = VECTOR('',#33345,1.) ;
#8713 = VECTOR('',#33346,1.) ;
#8714 = VECTOR('',#33349,1.) ;
#8715 = VECTOR('',#33350,1.) ;
#8716 = VECTOR('',#33353,1.) ;
#8717 = VECTOR('',#33354,1.) ;
#8718 = VECTOR('',#33357,1.) ;
#8719 = VECTOR('',#33358,1.) ;
#8720 = VECTOR('',#33359,1.) ;
#8721 = VECTOR('',#33362,1.) ;
#8722 = VECTOR('',#33363,1.) ;
#8723 = VECTOR('',#33366,1.) ;
#8724 = VECTOR('',#33367,1.) ;
#8725 = VECTOR('',#33370,1.) ;
#8726 = VECTOR('',#33371,1.) ;
#8727 = VECTOR('',#33372,1.) ;
#8728 = VECTOR('',#33373,1.) ;
#8729 = VECTOR('',#33374,1.) ;
#8730 = VECTOR('',#33375,1.) ;
#8731 = VECTOR('',#33376,1.) ;
#8732 = VECTOR('',#33377,1.) ;
#8733 = VECTOR('',#33378,1.) ;
#8734 = VECTOR('',#33379,1.) ;
#8735 = VECTOR('',#33382,1.) ;
#8736 = VECTOR('',#33383,1.) ;
#8737 = VECTOR('',#33384,1.) ;
#8738 = VECTOR('',#33387,1.) ;
#8739 = VECTOR('',#33392,1.) ;
#8740 = VECTOR('',#33393,1.) ;
#8741 = VECTOR('',#33394,1.) ;
#8742 = VECTOR('',#33395,1.) ;
#8743 = VECTOR('',#33396,1.) ;
#8744 = VECTOR('',#33399,1.) ;
#8745 = VECTOR('',#33400,1.) ;
#8746 = VECTOR('',#33401,1.) ;
#8747 = VECTOR('',#33402,1.) ;
#8748 = VECTOR('',#33403,1.) ;
#8749 = VECTOR('',#33404,1.) ;
#8750 = VECTOR('',#33405,1.) ;
#8751 = VECTOR('',#33406,1.) ;
#8752 = VECTOR('',#33407,1.) ;
#8753 = VECTOR('',#33408,1.) ;
#8754 = VECTOR('',#33409,1.) ;
#8755 = VECTOR('',#33410,1.) ;
#8756 = VECTOR('',#33411,1.) ;
#8757 = VECTOR('',#33412,1.) ;
#8758 = VECTOR('',#33413,1.) ;
#8759 = VECTOR('',#33414,1.) ;
#8760 = VECTOR('',#33415,1.) ;
#8761 = VECTOR('',#33416,1.) ;
#8762 = VECTOR('',#33417,1.) ;
#8763 = VECTOR('',#33418,1.) ;
#8764 = VECTOR('',#33421,1.) ;
#8765 = VECTOR('',#33422,1.) ;
#8766 = VECTOR('',#33423,1.) ;
#8767 = VECTOR('',#33424,1.) ;
#8768 = VECTOR('',#33425,1.) ;
#8769 = VECTOR('',#33426,1.) ;
#8770 = VECTOR('',#33427,1.) ;
#8771 = VECTOR('',#33428,1.) ;
#8772 = VECTOR('',#33429,1.) ;
#8773 = VECTOR('',#33430,1.) ;
#8774 = VECTOR('',#33431,1.) ;
#8775 = VECTOR('',#33432,1.) ;
#8776 = VECTOR('',#33433,1.) ;
#8777 = VECTOR('',#33434,1.) ;
#8778 = VECTOR('',#33435,1.) ;
#8779 = VECTOR('',#33436,1.) ;
#8780 = VECTOR('',#33437,1.) ;
#8781 = VECTOR('',#33438,1.) ;
#8782 = VECTOR('',#33439,1.) ;
#8783 = VECTOR('',#33440,1.) ;
#8784 = VECTOR('',#33441,1.) ;
#8785 = VECTOR('',#33442,1.) ;
#8786 = VECTOR('',#33443,1.) ;
#8787 = VECTOR('',#33444,1.) ;
#8788 = VECTOR('',#33445,1.) ;
#8789 = VECTOR('',#33446,1.) ;
#8790 = VECTOR('',#33447,1.) ;
#8791 = VECTOR('',#33448,1.) ;
#8792 = VECTOR('',#33451,1.) ;
#8793 = VECTOR('',#33454,1.) ;
#8794 = VECTOR('',#33455,1.) ;
#8795 = VECTOR('',#33456,1.) ;
#8796 = VECTOR('',#33457,1.) ;
#8797 = VECTOR('',#33460,1.) ;
#8798 = VECTOR('',#33461,1.) ;
#8799 = VECTOR('',#33462,1.) ;
#8800 = VECTOR('',#33465,1.) ;
#8801 = VECTOR('',#33466,1.) ;
#8802 = VECTOR('',#33467,1.) ;
#8803 = VECTOR('',#33468,1.) ;
#8804 = VECTOR('',#33469,1.) ;
#8805 = VECTOR('',#33470,1.) ;
#8806 = VECTOR('',#33473,1.) ;
#8807 = VECTOR('',#33474,1.) ;
#8808 = VECTOR('',#33475,1.) ;
#8809 = VECTOR('',#33476,1.) ;
#8810 = VECTOR('',#33477,1.) ;
#8811 = VECTOR('',#33478,1.) ;
#8812 = VECTOR('',#33479,1.) ;
#8813 = VECTOR('',#33480,1.) ;
#8814 = VECTOR('',#33481,1.) ;
#8815 = VECTOR('',#33482,1.) ;
#8816 = VECTOR('',#33483,1.) ;
#8817 = VECTOR('',#33484,1.) ;
#8818 = VECTOR('',#33485,1.) ;
#8819 = VECTOR('',#33486,1.) ;
#8820 = VECTOR('',#33487,1.) ;
#8821 = VECTOR('',#33488,1.) ;
#8822 = VECTOR('',#33489,1.) ;
#8823 = VECTOR('',#33490,1.) ;
#8824 = VECTOR('',#33493,1.) ;
#8825 = VECTOR('',#33494,1.) ;
#8826 = VECTOR('',#33495,1.) ;
#8827 = VECTOR('',#33496,1.) ;
#8828 = VECTOR('',#33497,1.) ;
#8829 = VECTOR('',#33500,1.) ;
#8830 = VECTOR('',#33501,1.) ;
#8831 = VECTOR('',#33502,1.) ;
#8832 = VECTOR('',#33503,1.) ;
#8833 = VECTOR('',#33504,1.) ;
#8834 = VECTOR('',#33505,1.) ;
#8835 = VECTOR('',#33506,1.) ;
#8836 = VECTOR('',#33507,1.) ;
#8837 = VECTOR('',#33508,1.) ;
#8838 = VECTOR('',#33509,1.) ;
#8839 = VECTOR('',#33510,1.) ;
#8840 = VECTOR('',#33511,1.) ;
#8841 = VECTOR('',#33514,1.) ;
#8842 = VECTOR('',#33515,1.) ;
#8843 = VECTOR('',#33516,1.) ;
#8844 = VECTOR('',#33517,1.) ;
#8845 = VECTOR('',#33518,1.) ;
#8846 = VECTOR('',#33519,1.) ;
#8847 = VECTOR('',#33520,1.) ;
#8848 = VECTOR('',#33521,1.) ;
#8849 = VECTOR('',#33522,1.) ;
#8850 = VECTOR('',#33523,1.) ;
#8851 = VECTOR('',#33524,1.) ;
#8852 = VECTOR('',#33525,1.) ;
#8853 = VECTOR('',#33526,1.) ;
#8854 = VECTOR('',#33527,1.) ;
#8855 = VECTOR('',#33528,1.) ;
#8856 = VECTOR('',#33529,1.) ;
#8857 = VECTOR('',#33530,1.) ;
#8858 = VECTOR('',#33531,1.) ;
#8859 = VECTOR('',#33532,1.) ;
#8860 = VECTOR('',#33533,1.) ;
#8861 = VECTOR('',#33534,1.) ;
#8862 = VECTOR('',#33535,1.) ;
#8863 = VECTOR('',#33536,1.) ;
#8864 = VECTOR('',#33537,1.) ;
#8865 = VECTOR('',#33538,1.) ;
#8866 = VECTOR('',#33539,1.) ;
#8867 = VECTOR('',#33540,1.) ;
#8868 = VECTOR('',#33541,1.) ;
#8869 = VECTOR('',#33542,1.) ;
#8870 = VECTOR('',#33543,1.) ;
#8871 = VECTOR('',#33544,1.) ;
#8872 = VECTOR('',#33545,1.) ;
#8873 = VECTOR('',#33546,1.) ;
#8874 = VECTOR('',#33547,1.) ;
#8875 = VECTOR('',#33548,1.) ;
#8876 = VECTOR('',#33549,1.) ;
#8877 = VECTOR('',#33550,1.) ;
#8878 = VECTOR('',#33551,1.) ;
#8879 = VECTOR('',#33552,1.) ;
#8880 = VECTOR('',#33555,1.) ;
#8881 = VECTOR('',#33556,1.) ;
#8882 = VECTOR('',#33559,1.) ;
#8883 = VECTOR('',#33560,1.) ;
#8884 = VECTOR('',#33563,1.) ;
#8885 = VECTOR('',#33564,1.) ;
#8886 = VECTOR('',#33565,1.) ;
#8887 = VECTOR('',#33568,1.) ;
#8888 = VECTOR('',#33569,1.) ;
#8889 = VECTOR('',#33570,1.) ;
#8890 = VECTOR('',#33571,1.) ;
#8891 = VECTOR('',#33572,1.) ;
#8892 = VECTOR('',#33573,1.) ;
#8893 = VECTOR('',#33576,1.) ;
#8894 = VECTOR('',#33579,1.) ;
#8895 = VECTOR('',#33582,1.) ;
#8896 = VECTOR('',#33585,1.) ;
#8897 = VECTOR('',#33586,1.) ;
#8898 = VECTOR('',#33589,1.) ;
#8899 = VECTOR('',#33590,1.) ;
#8900 = VECTOR('',#33593,1.) ;
#8901 = VECTOR('',#33594,1.) ;
#8902 = VECTOR('',#33597,1.) ;
#8903 = VECTOR('',#33598,1.) ;
#8904 = VECTOR('',#33601,1.) ;
#8905 = VECTOR('',#33602,1.) ;
#8906 = VECTOR('',#33605,1.) ;
#8907 = VECTOR('',#33606,1.) ;
#8908 = VECTOR('',#33609,1.) ;
#8909 = VECTOR('',#33610,1.) ;
#8910 = VECTOR('',#33613,1.) ;
#8911 = VECTOR('',#33614,1.) ;
#8912 = VECTOR('',#33617,1.) ;
#8913 = VECTOR('',#33618,1.) ;
#8914 = VECTOR('',#33621,1.) ;
#8915 = VECTOR('',#33622,1.) ;
#8916 = VECTOR('',#33625,1.) ;
#8917 = VECTOR('',#33628,1.) ;
#8918 = VECTOR('',#33631,1.) ;
#8919 = VECTOR('',#33632,1.) ;
#8920 = VECTOR('',#33635,1.) ;
#8921 = VECTOR('',#33638,1.) ;
#8922 = VECTOR('',#33641,1.) ;
#8923 = VECTOR('',#33646,1.) ;
#8924 = VECTOR('',#33649,1.) ;
#8925 = VECTOR('',#33652,1.) ;
#8926 = VECTOR('',#33655,1.) ;
#8927 = VECTOR('',#33658,1.) ;
#8928 = VECTOR('',#33661,1.) ;
#8929 = VECTOR('',#33664,1.) ;
#8930 = VECTOR('',#33667,1.) ;
#8931 = VECTOR('',#33670,1.) ;
#8932 = VECTOR('',#33673,1.) ;
#8933 = VECTOR('',#33674,1.) ;
#8934 = VECTOR('',#33677,1.) ;
#8935 = VECTOR('',#33680,1.) ;
#8936 = VECTOR('',#33683,1.) ;
#8937 = VECTOR('',#33684,1.) ;
#8938 = VECTOR('',#33687,1.) ;
#8939 = VECTOR('',#33690,1.) ;
#8940 = VECTOR('',#33693,1.) ;
#8941 = VECTOR('',#33698,1.) ;
#8942 = VECTOR('',#33699,1.) ;
#8943 = VECTOR('',#33702,1.) ;
#8944 = VECTOR('',#33703,1.) ;
#8945 = VECTOR('',#33706,1.) ;
#8946 = VECTOR('',#33707,1.) ;
#8947 = VECTOR('',#33710,1.) ;
#8948 = VECTOR('',#33711,1.) ;
#8949 = VECTOR('',#33714,1.) ;
#8950 = VECTOR('',#33715,1.) ;
#8951 = VECTOR('',#33718,1.) ;
#8952 = VECTOR('',#33721,1.) ;
#8953 = VECTOR('',#33726,1.) ;
#8954 = VECTOR('',#33729,1.) ;
#8955 = VECTOR('',#33734,1.) ;
#8956 = VECTOR('',#33739,1.) ;
#8957 = VECTOR('',#33744,1.) ;
#8958 = VECTOR('',#33749,1.) ;
#8959 = VECTOR('',#33752,1.) ;
#8960 = VECTOR('',#33755,1.) ;
#8961 = VECTOR('',#33758,1.) ;
#8962 = VECTOR('',#33759,1.) ;
#8963 = VECTOR('',#33762,1.) ;
#8964 = VECTOR('',#33763,1.) ;
#8965 = VECTOR('',#33766,1.) ;
#8966 = VECTOR('',#33769,1.) ;
#8967 = VECTOR('',#33772,1.) ;
#8968 = VECTOR('',#33777,1.) ;
#8969 = VECTOR('',#33780,1.) ;
#8970 = VECTOR('',#33781,1.) ;
#8971 = VECTOR('',#33784,1.) ;
#8972 = VECTOR('',#33785,1.) ;
#8973 = VECTOR('',#33788,1.) ;
#8974 = VECTOR('',#33791,1.) ;
#8975 = VECTOR('',#33792,1.) ;
#8976 = VECTOR('',#33795,1.) ;
#8977 = VECTOR('',#33796,1.) ;
#8978 = VECTOR('',#33799,1.) ;
#8979 = VECTOR('',#33804,1.) ;
#8980 = VECTOR('',#33807,1.) ;
#8981 = VECTOR('',#33812,1.) ;
#8982 = VECTOR('',#33817,1.) ;
#8983 = VECTOR('',#33820,1.) ;
#8984 = VECTOR('',#33823,1.) ;
#8985 = VECTOR('',#33826,1.) ;
#8986 = VECTOR('',#33831,1.) ;
#8987 = VECTOR('',#33836,1.) ;
#8988 = VECTOR('',#33839,1.) ;
#8989 = VECTOR('',#33840,1.) ;
#8990 = VECTOR('',#33843,1.) ;
#8991 = VECTOR('',#33846,1.) ;
#8992 = VECTOR('',#33847,1.) ;
#8993 = VECTOR('',#33850,1.) ;
#8994 = VECTOR('',#33853,1.) ;
#8995 = VECTOR('',#33856,1.) ;
#8996 = VECTOR('',#33859,1.) ;
#8997 = VECTOR('',#33864,1.) ;
#8998 = VECTOR('',#33865,1.) ;
#8999 = VECTOR('',#33868,1.) ;
#9000 = VECTOR('',#33869,1.) ;
#9001 = VECTOR('',#33872,1.) ;
#9002 = VECTOR('',#33873,1.) ;
#9003 = VECTOR('',#33876,1.) ;
#9004 = VECTOR('',#33877,1.) ;
#9005 = VECTOR('',#33880,1.) ;
#9006 = VECTOR('',#33881,1.) ;
#9007 = VECTOR('',#33884,1.) ;
#9008 = VECTOR('',#33887,1.) ;
#9009 = VECTOR('',#33894,1.) ;
#9010 = VECTOR('',#33897,1.) ;
#9011 = VECTOR('',#33902,1.) ;
#9012 = VECTOR('',#33905,1.) ;
#9013 = VECTOR('',#33910,1.) ;
#9014 = VECTOR('',#33915,1.) ;
#9015 = VECTOR('',#33920,1.) ;
#9016 = VECTOR('',#33925,1.) ;
#9017 = VECTOR('',#33928,1.) ;
#9018 = VECTOR('',#33929,1.) ;
#9019 = VECTOR('',#33932,1.) ;
#9020 = VECTOR('',#33933,1.) ;
#9021 = VECTOR('',#33936,1.) ;
#9022 = VECTOR('',#33937,1.) ;
#9023 = VECTOR('',#33940,1.) ;
#9024 = VECTOR('',#33941,1.) ;
#9025 = VECTOR('',#33944,1.) ;
#9026 = VECTOR('',#33947,1.) ;
#9027 = VECTOR('',#33948,1.) ;
#9028 = VECTOR('',#33951,1.) ;
#9029 = VECTOR('',#33954,1.) ;
#9030 = VECTOR('',#33955,1.) ;
#9031 = VECTOR('',#33958,1.) ;
#9032 = VECTOR('',#33961,1.) ;
#9033 = VECTOR('',#33964,1.) ;
#9034 = VECTOR('',#33969,1.) ;
#9035 = VECTOR('',#33974,1.) ;
#9036 = VECTOR('',#33977,1.) ;
#9037 = VECTOR('',#33982,1.) ;
#9038 = VECTOR('',#33985,1.) ;
#9039 = VECTOR('',#33990,1.) ;
#9040 = VECTOR('',#33995,1.) ;
#9041 = VECTOR('',#34000,1.) ;
#9042 = VECTOR('',#34003,1.) ;
#9043 = VECTOR('',#34006,1.) ;
#9044 = VECTOR('',#34009,1.) ;
#9045 = VECTOR('',#34012,1.) ;
#9046 = VECTOR('',#34015,1.) ;
#9047 = VECTOR('',#34018,1.) ;
#9048 = VECTOR('',#34019,1.) ;
#9049 = VECTOR('',#34022,1.) ;
#9050 = VECTOR('',#34027,1.) ;
#9051 = VECTOR('',#34030,1.) ;
#9052 = VECTOR('',#34031,1.) ;
#9053 = VECTOR('',#34034,1.) ;
#9054 = VECTOR('',#34035,1.) ;
#9055 = VECTOR('',#34038,1.) ;
#9056 = VECTOR('',#34039,1.) ;
#9057 = VECTOR('',#34042,1.) ;
#9058 = VECTOR('',#34043,1.) ;
#9059 = VECTOR('',#34046,1.) ;
#9060 = VECTOR('',#34047,1.) ;
#9061 = VECTOR('',#34050,1.) ;
#9062 = VECTOR('',#34051,1.) ;
#9063 = VECTOR('',#34058,1.) ;
#9064 = VECTOR('',#34061,1.) ;
#9065 = VECTOR('',#34068,1.) ;
#9066 = VECTOR('',#34073,1.) ;
#9067 = VECTOR('',#34078,1.) ;
#9068 = VECTOR('',#34081,1.) ;
#9069 = VECTOR('',#34086,1.) ;
#9070 = VECTOR('',#34091,1.) ;
#9071 = VECTOR('',#34094,1.) ;
#9072 = VECTOR('',#34097,1.) ;
#9073 = VECTOR('',#34100,1.) ;
#9074 = VECTOR('',#34103,1.) ;
#9075 = VECTOR('',#34106,1.) ;
#9076 = VECTOR('',#34111,1.) ;
#9077 = VECTOR('',#34112,1.) ;
#9078 = VECTOR('',#34115,1.) ;
#9079 = VECTOR('',#34116,1.) ;
#9080 = VECTOR('',#34119,1.) ;
#9081 = VECTOR('',#34120,1.) ;
#9082 = VECTOR('',#34123,1.) ;
#9083 = VECTOR('',#34124,1.) ;
#9084 = VECTOR('',#34127,1.) ;
#9085 = VECTOR('',#34128,1.) ;
#9086 = VECTOR('',#34135,1.) ;
#9087 = VECTOR('',#34144,1.) ;
#9088 = VECTOR('',#34147,1.) ;
#9089 = VECTOR('',#34152,1.) ;
#9090 = VECTOR('',#34155,1.) ;
#9091 = VECTOR('',#34160,1.) ;
#9092 = VECTOR('',#34163,1.) ;
#9093 = VECTOR('',#34166,1.) ;
#9094 = VECTOR('',#34167,1.) ;
#9095 = VECTOR('',#34170,1.) ;
#9096 = VECTOR('',#34171,1.) ;
#9097 = VECTOR('',#34174,1.) ;
#9098 = VECTOR('',#34175,1.) ;
#9099 = VECTOR('',#34178,1.) ;
#9100 = VECTOR('',#34181,1.) ;
#9101 = VECTOR('',#34182,1.) ;
#9102 = VECTOR('',#34187,1.) ;
#9103 = VECTOR('',#34190,1.) ;
#9104 = VECTOR('',#34195,1.) ;
#9105 = VECTOR('',#34202,1.) ;
#9106 = VECTOR('',#34207,1.) ;
#9107 = VECTOR('',#34210,1.) ;
#9108 = VECTOR('',#34213,1.) ;
#9109 = VECTOR('',#34218,1.) ;
#9110 = VECTOR('',#34221,1.) ;
#9111 = VECTOR('',#34224,1.) ;
#9112 = VECTOR('',#34229,1.) ;
#9113 = VECTOR('',#34232,1.) ;
#9114 = VECTOR('',#34235,1.) ;
#9115 = VECTOR('',#34236,1.) ;
#9116 = VECTOR('',#34239,1.) ;
#9117 = VECTOR('',#34240,1.) ;
#9118 = VECTOR('',#34243,1.) ;
#9119 = VECTOR('',#34244,1.) ;
#9120 = VECTOR('',#34247,1.) ;
#9121 = VECTOR('',#34250,1.) ;
#9122 = VECTOR('',#34255,1.) ;
#9123 = VECTOR('',#34260,1.) ;
#9124 = VECTOR('',#34267,1.) ;
#9125 = VECTOR('',#34270,1.) ;
#9126 = VECTOR('',#34275,1.) ;
#9127 = VECTOR('',#34280,1.) ;
#9128 = VECTOR('',#34281,1.) ;
#9129 = VECTOR('',#34286,1.) ;
#9130 = VECTOR('',#34287,1.) ;
#9131 = VECTOR('',#34292,1.) ;
#9132 = VECTOR('',#34297,1.) ;
#9133 = VECTOR('',#34302,1.) ;
#9134 = VECTOR('',#34305,1.) ;
#9135 = VECTOR('',#34308,1.) ;
#9136 = VECTOR('',#34311,1.) ;
#9137 = VECTOR('',#34314,1.) ;
#9138 = VECTOR('',#34317,1.) ;
#9139 = VECTOR('',#34322,1.) ;
#9140 = VECTOR('',#34327,1.) ;
#9141 = VECTOR('',#34330,1.) ;
#9142 = VECTOR('',#34337,1.) ;
#9143 = VECTOR('',#34340,1.) ;
#9144 = VECTOR('',#34343,1.) ;
#9145 = VECTOR('',#34350,1.) ;
#9146 = VECTOR('',#34353,1.) ;
#9147 = VECTOR('',#34592,2.) ;
#9148 = VECTOR('',#34599,2.) ;
#9149 = VECTOR('',#34606,2.) ;
#9150 = VECTOR('',#34613,2.) ;
#9151 = VECTOR('',#34620,2.) ;
#9152 = VECTOR('',#34627,2.) ;
#9153 = VECTOR('',#34634,2.) ;
#9154 = VECTOR('',#34641,2.) ;
#9155 = VECTOR('',#34646,2.) ;
#9156 = VECTOR('',#34651,2.) ;
#9157 = VECTOR('',#34656,2.) ;
#9158 = VECTOR('',#34661,2.) ;
#9159 = VECTOR('',#34666,2.) ;
#9160 = VECTOR('',#34671,2.) ;
#9161 = VECTOR('',#34676,2.) ;
#9162 = VECTOR('',#34681,2.) ;
#9163 = VECTOR('',#34686,2.) ;
#9164 = VECTOR('',#34691,2.) ;
#9165 = VECTOR('',#34696,2.) ;
#9166 = VECTOR('',#34701,2.) ;
#9167 = VECTOR('',#34706,2.) ;
#9168 = VECTOR('',#34713,2.) ;
#9169 = VECTOR('',#34720,2.) ;
#9170 = VECTOR('',#34727,2.) ;
#9171 = VECTOR('',#34734,2.) ;
#9172 = VECTOR('',#34741,2.) ;
#9173 = VECTOR('',#34748,2.) ;
#9174 = VECTOR('',#34755,2.) ;
#9175 = VECTOR('',#34776,0.65) ;
#9176 = VECTOR('',#34783,0.65) ;
#9177 = VECTOR('',#34790,0.65) ;
#9178 = VECTOR('',#34797,0.65) ;
#9179 = VECTOR('',#34804,0.65) ;
#9180 = VECTOR('',#34811,0.65) ;
#9181 = VECTOR('',#34816,1.) ;
#9182 = VECTOR('',#34819,1.) ;
#9183 = VECTOR('',#34824,1.) ;
#9184 = VECTOR('',#34825,1.) ;
#9185 = VECTOR('',#34826,1.) ;
#9186 = VECTOR('',#34827,1.) ;
#9187 = VECTOR('',#34830,1.) ;
#9188 = VECTOR('',#34831,1.) ;
#9189 = VECTOR('',#34832,1.) ;
#9190 = VECTOR('',#34833,1.) ;
#9191 = VECTOR('',#34836,1.) ;
#9192 = VECTOR('',#34837,1.) ;
#9193 = VECTOR('',#34838,1.) ;
#9194 = VECTOR('',#34841,1.) ;
#9195 = VECTOR('',#34844,1.) ;
#9196 = VECTOR('',#34847,1.) ;
#9197 = VECTOR('',#34854,0.65) ;
#9198 = VECTOR('',#34861,0.65) ;
#9199 = VECTOR('',#34866,1.) ;
#9200 = VECTOR('',#34869,1.) ;
#9201 = VECTOR('',#34874,1.) ;
#9202 = VECTOR('',#34875,1.) ;
#9203 = VECTOR('',#34876,1.) ;
#9204 = VECTOR('',#34877,1.) ;
#9205 = VECTOR('',#34880,1.) ;
#9206 = VECTOR('',#34881,1.) ;
#9207 = VECTOR('',#34882,1.) ;
#9208 = VECTOR('',#34883,1.) ;
#9209 = VECTOR('',#34886,1.) ;
#9210 = VECTOR('',#34887,1.) ;
#9211 = VECTOR('',#34888,1.) ;
#9212 = VECTOR('',#34891,1.) ;
#9213 = VECTOR('',#34894,1.) ;
#9214 = VECTOR('',#34897,1.) ;
#9215 = VECTOR('',#34904,1.28) ;
#9216 = VECTOR('',#34911,1.28) ;
#9217 = VECTOR('',#34918,1.2) ;
#9218 = VECTOR('',#34925,1.5) ;
#9219 = VECTOR('',#34932,1.) ;
#9220 = VECTOR('',#34933,1.) ;
#9221 = VECTOR('',#34934,1.) ;
#9222 = VECTOR('',#34935,1.) ;
#9223 = VECTOR('',#34936,1.) ;
#9224 = VECTOR('',#34943,1.2) ;
#9225 = VECTOR('',#34950,1.5) ;
#9226 = VECTOR('',#34957,1.) ;
#9227 = VECTOR('',#34958,1.) ;
#9228 = VECTOR('',#34959,1.) ;
#9229 = VECTOR('',#34960,1.) ;
#9230 = VECTOR('',#34963,1.) ;
#9231 = VECTOR('',#34964,1.) ;
#9232 = VECTOR('',#34965,1.) ;
#9233 = VECTOR('',#34968,1.) ;
#9234 = VECTOR('',#34969,1.) ;
#9235 = VECTOR('',#34970,1.) ;
#9236 = VECTOR('',#34973,1.) ;
#9237 = VECTOR('',#34974,1.) ;
#9238 = VECTOR('',#34977,1.) ;
#9239 = VECTOR('',#34978,1.) ;
#9240 = VECTOR('',#34979,1.) ;
#9241 = VECTOR('',#34980,1.) ;
#9242 = VECTOR('',#34983,1.) ;
#9243 = VECTOR('',#34984,1.) ;
#9244 = VECTOR('',#34985,1.) ;
#9245 = VECTOR('',#34988,1.) ;
#9246 = VECTOR('',#34989,1.) ;
#9247 = VECTOR('',#34990,1.) ;
#9248 = VECTOR('',#34993,1.) ;
#9249 = VECTOR('',#34994,1.) ;
#9250 = VECTOR('',#34995,1.) ;
#9251 = VECTOR('',#34996,1.) ;
#9252 = VECTOR('',#35001,1.) ;
#9253 = VECTOR('',#35002,1.) ;
#9254 = VECTOR('',#35003,1.) ;
#9255 = VECTOR('',#35004,1.) ;
#9256 = VECTOR('',#35011,1.) ;
#9257 = VECTOR('',#35012,1.) ;
#9258 = VECTOR('',#35013,1.) ;
#9259 = VECTOR('',#35014,1.) ;
#9260 = VECTOR('',#35019,1.) ;
#9261 = VECTOR('',#35020,1.) ;
#9262 = VECTOR('',#35021,1.) ;
#9263 = VECTOR('',#35022,1.) ;
#9264 = VECTOR('',#35023,1.) ;
#9265 = VECTOR('',#35024,1.) ;
#9266 = VECTOR('',#35025,1.) ;
#9267 = VECTOR('',#35028,1.) ;
#9268 = VECTOR('',#35029,1.) ;
#9269 = VECTOR('',#35030,1.) ;
#9270 = VECTOR('',#35031,1.) ;
#9271 = VECTOR('',#35032,1.) ;
#9272 = VECTOR('',#35033,1.) ;
#9273 = VECTOR('',#35034,1.) ;
#9274 = VECTOR('',#35037,1.) ;
#9275 = VECTOR('',#35040,1.) ;
#9276 = VECTOR('',#35043,1.) ;
#9277 = VECTOR('',#35044,1.) ;
#9278 = VECTOR('',#35047,1.) ;
#9279 = VECTOR('',#35048,1.) ;
#9280 = VECTOR('',#35053,1.) ;
#9281 = VECTOR('',#35054,1.) ;
#9282 = VECTOR('',#35055,1.) ;
#9283 = VECTOR('',#35058,1.) ;
#9284 = VECTOR('',#35059,1.) ;
#9285 = VECTOR('',#35060,1.) ;
#9286 = VECTOR('',#35061,1.) ;
#9287 = VECTOR('',#35064,1.) ;
#9288 = VECTOR('',#35065,1.) ;
#9289 = VECTOR('',#35066,1.) ;
#9290 = VECTOR('',#35067,1.) ;
#9291 = VECTOR('',#35070,1.) ;
#9292 = VECTOR('',#35071,1.) ;
#9293 = VECTOR('',#35072,1.) ;
#9294 = VECTOR('',#35073,1.) ;
#9295 = VECTOR('',#35076,1.) ;
#9296 = VECTOR('',#35077,1.) ;
#9297 = VECTOR('',#35078,1.) ;
#9298 = VECTOR('',#35081,1.) ;
#9299 = VECTOR('',#35082,1.) ;
#9300 = VECTOR('',#35083,1.) ;
#9301 = VECTOR('',#35088,1.) ;
#9302 = VECTOR('',#35089,1.) ;
#9303 = VECTOR('',#35090,1.) ;
#9304 = VECTOR('',#35095,1.) ;
#9305 = VECTOR('',#35096,1.) ;
#9306 = VECTOR('',#35097,1.) ;
#9307 = VECTOR('',#35098,1.) ;
#9308 = VECTOR('',#35099,1.) ;
#9309 = VECTOR('',#35100,1.) ;
#9310 = VECTOR('',#35101,1.) ;
#9311 = VECTOR('',#35102,1.) ;
#9312 = VECTOR('',#35103,1.) ;
#9313 = VECTOR('',#35104,1.) ;
#9314 = VECTOR('',#35105,1.) ;
#9315 = VECTOR('',#35106,1.) ;
#9316 = VECTOR('',#35107,1.) ;
#9317 = VECTOR('',#35108,1.) ;
#9318 = VECTOR('',#35109,1.) ;
#9319 = VECTOR('',#35110,1.) ;
#9320 = VECTOR('',#35111,1.) ;
#9321 = VECTOR('',#35112,1.) ;
#9322 = VECTOR('',#35113,1.) ;
#9323 = VECTOR('',#35114,1.) ;
#9324 = VECTOR('',#35115,1.) ;
#9325 = VECTOR('',#35116,1.) ;
#9326 = VECTOR('',#35121,1.) ;
#9327 = VECTOR('',#35122,1.) ;
#9328 = VECTOR('',#35125,1.) ;
#9329 = VECTOR('',#35126,1.) ;
#9330 = VECTOR('',#35129,1.) ;
#9331 = VECTOR('',#35130,1.) ;
#9332 = VECTOR('',#35133,1.) ;
#9333 = VECTOR('',#35134,1.) ;
#9334 = VECTOR('',#35135,1.) ;
#9335 = VECTOR('',#35138,1.) ;
#9336 = VECTOR('',#35139,1.) ;
#9337 = VECTOR('',#35142,1.) ;
#9338 = VECTOR('',#35143,1.) ;
#9339 = VECTOR('',#35144,1.) ;
#9340 = VECTOR('',#35147,1.) ;
#9341 = VECTOR('',#35148,1.) ;
#9342 = VECTOR('',#35151,1.) ;
#9343 = VECTOR('',#35152,1.) ;
#9344 = VECTOR('',#35153,1.) ;
#9345 = VECTOR('',#35156,1.) ;
#9346 = VECTOR('',#35157,1.) ;
#9347 = VECTOR('',#35168,1.) ;
#9348 = VECTOR('',#35169,1.) ;
#9349 = VECTOR('',#35170,1.) ;
#9350 = VECTOR('',#35171,1.) ;
#9351 = VECTOR('',#35174,1.) ;
#9352 = VECTOR('',#35175,1.) ;
#9353 = VECTOR('',#35176,1.) ;
#9354 = VECTOR('',#35179,1.) ;
#9355 = VECTOR('',#35180,1.) ;
#9356 = VECTOR('',#35183,1.) ;
#9357 = VECTOR('',#35188,1.) ;
#9358 = VECTOR('',#35193,1.) ;
#9359 = VECTOR('',#35210,3.) ;
#9360 = VECTOR('',#35213,3.) ;
#9361 = VECTOR('',#35216,2.6) ;
#9362 = VECTOR('',#35219,2.6) ;
#9363 = VECTOR('',#35222,1.) ;
#9364 = VECTOR('',#35223,1.) ;
#9365 = VECTOR('',#35224,1.) ;
#9366 = VECTOR('',#35227,1.) ;
#9367 = VECTOR('',#35228,1.) ;
#9368 = VECTOR('',#35229,1.) ;
#9369 = VECTOR('',#35230,1.) ;
#9370 = VECTOR('',#35233,1.) ;
#9371 = VECTOR('',#35234,1.) ;
#9372 = VECTOR('',#35235,1.) ;
#9373 = VECTOR('',#35236,1.) ;
#9374 = VECTOR('',#35239,1.) ;
#9375 = VECTOR('',#35240,1.) ;
#9376 = VECTOR('',#35243,1.) ;
#9377 = VECTOR('',#35244,1.) ;
#9378 = VECTOR('',#35245,1.) ;
#9379 = VECTOR('',#35248,1.) ;
#9380 = VECTOR('',#35249,1.) ;
#9381 = VECTOR('',#35252,1.) ;
#9382 = VECTOR('',#35255,1.) ;
#9383 = VECTOR('',#35258,1.) ;
#9384 = VECTOR('',#35259,1.) ;
#9385 = VECTOR('',#35260,1.) ;
#9386 = VECTOR('',#35261,1.) ;
#9387 = VECTOR('',#35264,1.) ;
#9388 = VECTOR('',#35265,1.) ;
#9389 = VECTOR('',#35268,1.) ;
#9390 = VECTOR('',#35271,1.) ;
#9391 = VECTOR('',#35274,1.) ;
#9392 = VECTOR('',#35275,1.) ;
#9393 = VECTOR('',#35276,1.) ;
#9394 = VECTOR('',#35277,1.) ;
#9395 = VECTOR('',#35280,1.) ;
#9396 = VECTOR('',#35281,1.) ;
#9397 = VECTOR('',#35284,1.) ;
#9398 = VECTOR('',#35287,1.) ;
#9399 = VECTOR('',#35302,1.5) ;
#9400 = VECTOR('',#35307,1.2) ;
#9401 = VECTOR('',#35320,1.5) ;
#9402 = VECTOR('',#35323,1.2) ;
#9403 = VECTOR('',#35326,1.) ;
#9404 = VECTOR('',#35335,1.) ;
#9405 = VECTOR('',#35338,1.) ;
#9406 = VECTOR('',#35341,1.) ;
#9407 = VECTOR('',#35344,1.) ;
#9408 = VECTOR('',#35345,1.) ;
#9409 = VECTOR('',#35346,1.) ;
#9410 = VECTOR('',#35349,1.) ;
#9411 = VECTOR('',#35350,1.) ;
#9412 = VECTOR('',#35357,1.) ;
#9413 = VECTOR('',#35360,1.) ;
#9414 = VECTOR('',#35363,1.) ;
#9415 = VECTOR('',#35364,1.) ;
#9416 = VECTOR('',#35367,1.) ;
#9417 = VECTOR('',#35368,1.) ;
#9418 = VECTOR('',#35369,1.) ;
#9419 = VECTOR('',#35372,1.) ;
#9420 = VECTOR('',#35373,1.) ;
#9421 = VECTOR('',#35374,1.) ;
#9422 = VECTOR('',#35375,1.) ;
#9423 = VECTOR('',#35378,1.) ;
#9424 = VECTOR('',#35379,1.) ;
#9425 = VECTOR('',#35380,1.) ;
#9426 = VECTOR('',#35381,1.) ;
#9427 = VECTOR('',#35384,1.) ;
#9428 = VECTOR('',#35385,1.) ;
#9429 = VECTOR('',#35386,1.) ;
#9430 = VECTOR('',#35389,1.) ;
#9431 = VECTOR('',#35392,1.) ;
#9432 = VECTOR('',#35395,1.) ;
#9433 = VECTOR('',#35402,1.) ;
#9434 = VECTOR('',#35405,1.) ;
#9435 = VECTOR('',#35408,1.) ;
#9436 = VECTOR('',#35409,1.) ;
#9437 = VECTOR('',#35410,1.) ;
#9438 = VECTOR('',#35413,1.) ;
#9439 = VECTOR('',#35414,1.) ;
#9440 = VECTOR('',#35417,1.) ;
#9441 = VECTOR('',#35418,1.) ;
#9442 = VECTOR('',#35421,1.) ;
#9443 = VECTOR('',#35426,1.) ;
#9444 = VECTOR('',#35427,1.) ;
#9445 = VECTOR('',#35428,1.) ;
#9446 = VECTOR('',#35429,1.) ;
#9447 = VECTOR('',#35434,1.) ;
#9448 = VECTOR('',#35435,1.) ;
#9449 = VECTOR('',#35438,1.) ;
#9450 = VECTOR('',#35439,1.) ;
#9451 = VECTOR('',#35444,1.) ;
#9452 = VECTOR('',#35447,1.) ;
#9453 = VECTOR('',#35454,1.) ;
#9454 = VECTOR('',#35459,1.) ;
#9455 = VECTOR('',#35462,1.) ;
#9456 = VECTOR('',#35463,1.) ;
#9457 = VECTOR('',#35468,1.) ;
#9458 = VECTOR('',#35469,1.) ;
#9459 = VECTOR('',#35470,1.) ;
#9460 = VECTOR('',#35471,1.) ;
#9461 = VECTOR('',#35474,1.) ;
#9462 = VECTOR('',#35475,1.) ;
#9463 = VECTOR('',#35476,1.) ;
#9464 = VECTOR('',#35489,1.) ;
#9465 = VECTOR('',#35492,1.) ;
#9466 = VECTOR('',#35495,1.) ;
#9467 = VECTOR('',#35496,1.) ;
#9468 = VECTOR('',#35497,1.) ;
#9469 = VECTOR('',#35500,1.) ;
#9470 = VECTOR('',#35505,1.) ;
#9471 = VECTOR('',#35510,1.) ;
#9472 = VECTOR('',#35511,1.) ;
#9473 = VECTOR('',#35512,1.) ;
#9474 = VECTOR('',#35513,1.) ;
#9475 = VECTOR('',#35516,1.) ;
#9476 = VECTOR('',#35517,1.) ;
#9477 = VECTOR('',#35518,1.) ;
#9478 = VECTOR('',#35531,1.) ;
#9479 = VECTOR('',#35532,1.) ;
#9480 = VECTOR('',#35537,1.) ;
#9481 = VECTOR('',#35540,1.) ;
#9482 = VECTOR('',#35543,1.) ;
#9483 = VECTOR('',#35544,1.) ;
#9484 = VECTOR('',#35547,1.) ;
#9485 = VECTOR('',#35552,1.) ;
#9486 = VECTOR('',#35553,1.) ;
#9487 = VECTOR('',#35554,1.) ;
#9488 = VECTOR('',#35555,1.) ;
#9489 = VECTOR('',#35560,1.) ;
#9490 = VECTOR('',#35565,1.) ;
#9491 = VECTOR('',#35568,1.) ;
#9492 = VECTOR('',#35573,1.) ;
#9493 = VECTOR('',#35574,1.) ;
#9494 = VECTOR('',#35579,1.) ;
#9495 = VECTOR('',#35582,1.) ;
#9496 = VECTOR('',#35585,1.) ;
#9497 = VECTOR('',#35586,1.) ;
#9498 = VECTOR('',#35589,1.) ;
#9499 = VECTOR('',#35594,1.) ;
#9500 = VECTOR('',#35595,1.) ;
#9501 = VECTOR('',#35596,1.) ;
#9502 = VECTOR('',#35597,1.) ;
#9503 = VECTOR('',#35610,1.) ;
#9504 = VECTOR('',#35613,1.) ;
#9505 = VECTOR('',#35618,1.) ;
#9506 = VECTOR('',#35621,1.) ;
#9507 = VECTOR('',#35626,1.) ;
#9508 = VECTOR('',#35627,1.) ;
#9509 = VECTOR('',#35628,1.) ;
#9510 = VECTOR('',#35629,1.) ;
#9511 = VECTOR('',#35642,1.) ;
#9512 = VECTOR('',#35645,1.) ;
#9513 = VECTOR('',#35650,1.) ;
#9514 = VECTOR('',#35653,1.) ;
#9515 = VECTOR('',#35658,1.) ;
#9516 = VECTOR('',#35659,1.) ;
#9517 = VECTOR('',#35660,1.) ;
#9518 = VECTOR('',#35661,1.) ;
#9519 = VECTOR('',#35674,1.) ;
#9520 = VECTOR('',#35675,1.) ;
#9521 = VECTOR('',#35676,1.) ;
#9522 = VECTOR('',#35677,1.) ;
#9523 = VECTOR('',#35680,1.) ;
#9524 = VECTOR('',#35681,1.) ;
#9525 = VECTOR('',#35682,1.) ;
#9526 = VECTOR('',#35685,1.) ;
#9527 = VECTOR('',#35686,1.) ;
#9528 = VECTOR('',#35687,1.) ;
#9529 = VECTOR('',#35690,1.) ;
#9530 = VECTOR('',#35691,1.) ;
#9531 = VECTOR('',#35698,1.) ;
#9532 = VECTOR('',#35699,1.) ;
#9533 = VECTOR('',#35700,1.) ;
#9534 = VECTOR('',#35701,1.) ;
#9535 = VECTOR('',#35704,1.) ;
#9536 = VECTOR('',#35705,1.) ;
#9537 = VECTOR('',#35706,1.) ;
#9538 = VECTOR('',#35707,1.) ;
#9539 = VECTOR('',#35710,1.) ;
#9540 = VECTOR('',#35711,1.) ;
#9541 = VECTOR('',#35714,1.) ;
#9542 = VECTOR('',#35717,1.) ;
#9543 = VECTOR('',#35722,1.) ;
#9544 = VECTOR('',#35723,1.) ;
#9545 = VECTOR('',#35724,1.) ;
#9546 = VECTOR('',#35725,1.) ;
#9547 = VECTOR('',#35728,1.) ;
#9548 = VECTOR('',#35729,1.) ;
#9549 = VECTOR('',#35730,1.) ;
#9550 = VECTOR('',#35733,1.) ;
#9551 = VECTOR('',#35734,1.) ;
#9552 = VECTOR('',#35735,1.) ;
#9553 = VECTOR('',#35738,1.) ;
#9554 = VECTOR('',#35739,1.) ;
#9555 = VECTOR('',#35740,1.) ;
#9556 = VECTOR('',#35741,1.) ;
#9557 = VECTOR('',#35742,1.) ;
#9558 = VECTOR('',#35743,1.) ;
#9559 = VECTOR('',#35744,1.) ;
#9560 = VECTOR('',#35745,1.) ;
#9561 = VECTOR('',#35746,1.) ;
#9562 = VECTOR('',#35749,1.) ;
#9563 = VECTOR('',#35750,1.) ;
#9564 = VECTOR('',#35753,1.) ;
#9565 = VECTOR('',#35754,1.) ;
#9566 = VECTOR('',#35757,1.) ;
#9567 = VECTOR('',#35758,1.) ;
#9568 = VECTOR('',#35759,1.) ;
#9569 = VECTOR('',#35760,1.) ;
#9570 = VECTOR('',#35761,1.) ;
#9571 = VECTOR('',#35762,1.) ;
#9572 = VECTOR('',#35763,1.) ;
#9573 = VECTOR('',#35766,1.) ;
#9574 = VECTOR('',#35767,1.) ;
#9575 = VECTOR('',#35772,1.) ;
#9576 = VECTOR('',#35775,1.) ;
#9577 = VECTOR('',#35778,1.) ;
#9578 = VECTOR('',#35781,1.) ;
#9579 = VECTOR('',#35786,1.) ;
#9580 = VECTOR('',#35789,1.) ;
#9581 = VECTOR('',#35794,1.) ;
#9582 = VECTOR('',#35795,1.) ;
#9583 = VECTOR('',#35804,1.) ;
#9584 = VECTOR('',#35807,1.) ;
#9585 = VECTOR('',#35808,1.) ;
#9586 = VECTOR('',#35809,1.) ;
#9587 = VECTOR('',#35814,1.) ;
#9588 = VECTOR('',#35817,1.) ;
#9589 = VECTOR('',#35820,1.) ;
#9590 = VECTOR('',#35823,1.) ;
#9591 = VECTOR('',#35828,1.) ;
#9592 = VECTOR('',#35831,1.) ;
#9593 = VECTOR('',#35834,1.) ;
#9594 = VECTOR('',#35837,1.) ;
#9595 = VECTOR('',#35844,1.) ;
#9596 = VECTOR('',#35845,1.) ;
#9597 = VECTOR('',#35846,1.) ;
#9598 = VECTOR('',#35847,1.) ;
#9599 = VECTOR('',#35850,1.) ;
#9600 = VECTOR('',#35851,1.) ;
#9601 = VECTOR('',#35852,1.) ;
#9602 = VECTOR('',#35853,1.) ;
#9603 = VECTOR('',#35856,1.) ;
#9604 = VECTOR('',#35857,1.) ;
#9605 = VECTOR('',#35860,1.) ;
#9606 = VECTOR('',#35863,1.) ;
#9607 = VECTOR('',#35870,0.35) ;
#9608 = VECTOR('',#35879,2.25) ;
#9609 = VECTOR('',#35888,1.4) ;
#9610 = VECTOR('',#35895,0.35) ;
#9611 = VECTOR('',#35904,2.) ;
#9612 = VECTOR('',#35913,1.25) ;
#9613 = VECTOR('',#35940,0.65) ;
#9614 = VECTOR('',#35947,0.65) ;
#9615 = VECTOR('',#35954,0.65) ;
#9616 = VECTOR('',#35961,0.65) ;
#9617 = VECTOR('',#35966,1.) ;
#9618 = VECTOR('',#35969,1.) ;
#9619 = VECTOR('',#35974,1.) ;
#9620 = VECTOR('',#35977,1.) ;
#9621 = VECTOR('',#35978,1.) ;
#9622 = VECTOR('',#35989,1.) ;
#9623 = VECTOR('',#35990,1.) ;
#9624 = VECTOR('',#35993,1.) ;
#9625 = VECTOR('',#35996,1.) ;
#9626 = VECTOR('',#35997,1.) ;
#9627 = VECTOR('',#35998,1.) ;
#9628 = VECTOR('',#36001,1.) ;
#9629 = VECTOR('',#36004,1.) ;
#9630 = VECTOR('',#36009,1.) ;
#9631 = VECTOR('',#36010,1.) ;
#9632 = VECTOR('',#36013,1.) ;
#9633 = VECTOR('',#36014,1.) ;
#9634 = VECTOR('',#36015,1.) ;
#9635 = VECTOR('',#36016,1.) ;
#9636 = VECTOR('',#36017,1.) ;
#9637 = VECTOR('',#36018,1.) ;
#9638 = VECTOR('',#36019,1.) ;
#9639 = VECTOR('',#36020,1.) ;
#9640 = VECTOR('',#36021,1.) ;
#9641 = VECTOR('',#36022,1.) ;
#9642 = VECTOR('',#36023,1.) ;
#9643 = VECTOR('',#36028,1.) ;
#9644 = VECTOR('',#36033,1.) ;
#9645 = VECTOR('',#36034,1.) ;
#9646 = VECTOR('',#36037,1.) ;
#9647 = VECTOR('',#36038,1.) ;
#9648 = VECTOR('',#36039,1.) ;
#9649 = VECTOR('',#36040,1.) ;
#9650 = VECTOR('',#36041,1.) ;
#9651 = VECTOR('',#36042,1.) ;
#9652 = VECTOR('',#36043,1.) ;
#9653 = VECTOR('',#36044,1.) ;
#9654 = VECTOR('',#36045,1.) ;
#9655 = VECTOR('',#36046,1.) ;
#9656 = VECTOR('',#36047,1.) ;
#9657 = VECTOR('',#36048,1.) ;
#9658 = VECTOR('',#36049,1.) ;
#9659 = VECTOR('',#36050,1.) ;
#9660 = VECTOR('',#36063,0.5) ;
#9661 = VECTOR('',#36072,1.) ;
#9662 = VECTOR('',#36077,1.) ;
#9663 = VECTOR('',#36080,1.) ;
#9664 = VECTOR('',#36085,1.) ;
#9665 = VECTOR('',#36088,1.) ;
#9666 = VECTOR('',#36093,1.) ;
#9667 = VECTOR('',#36094,1.) ;
#9668 = VECTOR('',#36095,1.) ;
#9669 = VECTOR('',#36096,1.) ;
#9670 = VECTOR('',#36097,1.) ;
#9671 = VECTOR('',#36100,1.) ;
#9672 = VECTOR('',#36101,1.) ;
#9673 = VECTOR('',#36104,1.) ;
#9674 = VECTOR('',#36105,1.) ;
#9675 = VECTOR('',#36108,1.) ;
#9676 = VECTOR('',#36109,1.) ;
#9677 = VECTOR('',#36110,1.) ;
#9678 = VECTOR('',#36111,1.) ;
#9679 = VECTOR('',#36112,1.) ;
#9680 = VECTOR('',#36115,1.) ;
#9681 = VECTOR('',#36116,1.) ;
#9682 = VECTOR('',#36119,1.) ;
#9683 = VECTOR('',#36120,1.) ;
#9684 = VECTOR('',#36123,1.) ;
#9685 = VECTOR('',#36124,1.) ;
#9686 = VECTOR('',#36127,1.) ;
#9687 = VECTOR('',#36128,1.) ;
#9688 = VECTOR('',#36131,1.) ;
#9689 = VECTOR('',#36134,1.) ;
#9690 = VECTOR('',#36135,1.) ;
#9691 = VECTOR('',#36138,1.) ;
#9692 = VECTOR('',#36139,1.) ;
#9693 = VECTOR('',#36142,1.) ;
#9694 = VECTOR('',#36153,7.) ;
#9695 = VECTOR('',#36154,1.) ;
#9696 = VECTOR('',#36155,1.) ;
#9697 = VECTOR('',#36160,2.5) ;
#9698 = VECTOR('',#36165,1.02) ;
#9699 = VECTOR('',#36176,1.51) ;
#9700 = VECTOR('',#36185,3.) ;
#9701 = VECTOR('',#36194,1.77) ;
#9702 = VECTOR('',#36201,3.5) ;
#9703 = VECTOR('',#36208,1.) ;
#9704 = VECTOR('',#36209,1.) ;
#9705 = VECTOR('',#36210,1.) ;
#9706 = VECTOR('',#36213,1.) ;
#9707 = VECTOR('',#36214,1.) ;
#9708 = VECTOR('',#36215,1.) ;
#9709 = VECTOR('',#36218,1.) ;
#9710 = VECTOR('',#36221,1.) ;
#9711 = VECTOR('',#36224,1.) ;
#9712 = VECTOR('',#36225,1.) ;
#9713 = VECTOR('',#36226,1.) ;
#9714 = VECTOR('',#36227,1.) ;
#9715 = VECTOR('',#36230,1.) ;
#9716 = VECTOR('',#36231,1.) ;
#9717 = VECTOR('',#36232,1.) ;
#9718 = VECTOR('',#36235,1.) ;
#9719 = VECTOR('',#36236,1.) ;
#9720 = VECTOR('',#36237,1.) ;
#9721 = VECTOR('',#36240,1.) ;
#9722 = VECTOR('',#36243,1.) ;
#9723 = VECTOR('',#36246,1.) ;
#9724 = VECTOR('',#36247,1.) ;
#9725 = VECTOR('',#36250,1.) ;
#9726 = VECTOR('',#36251,1.) ;
#9727 = VECTOR('',#36254,1.) ;
#9728 = VECTOR('',#36259,1.) ;
#9729 = VECTOR('',#36260,1.) ;
#9730 = VECTOR('',#36261,1.) ;
#9731 = VECTOR('',#36264,1.) ;
#9732 = VECTOR('',#36265,1.) ;
#9733 = VECTOR('',#36266,1.) ;
#9734 = VECTOR('',#36269,1.) ;
#9735 = VECTOR('',#36270,1.) ;
#9736 = VECTOR('',#36275,1.) ;
#9737 = VECTOR('',#36284,0.49) ;
#9738 = VECTOR('',#36291,1.) ;
#9739 = VECTOR('',#36292,1.) ;
#9740 = VECTOR('',#36293,1.) ;
#9741 = VECTOR('',#36294,1.) ;
#9742 = VECTOR('',#36297,1.) ;
#9743 = VECTOR('',#36298,1.) ;
#9744 = VECTOR('',#36299,1.) ;
#9745 = VECTOR('',#36300,1.) ;
#9746 = VECTOR('',#36303,1.) ;
#9747 = VECTOR('',#36304,1.) ;
#9748 = VECTOR('',#36305,1.) ;
#9749 = VECTOR('',#36306,1.) ;
#9750 = VECTOR('',#36309,1.) ;
#9751 = VECTOR('',#36310,1.) ;
#9752 = VECTOR('',#36313,1.) ;
#9753 = VECTOR('',#36314,1.) ;
#9754 = VECTOR('',#36317,1.) ;
#9755 = VECTOR('',#36320,1.) ;
#9756 = VECTOR('',#36327,1.) ;
#9757 = VECTOR('',#36330,1.) ;
#9758 = VECTOR('',#36331,1.) ;
#9759 = VECTOR('',#36336,1.) ;
#9760 = VECTOR('',#36339,1.) ;
#9761 = VECTOR('',#36340,1.) ;
#9762 = VECTOR('',#36345,1.) ;
#9763 = VECTOR('',#36348,1.) ;
#9764 = VECTOR('',#36353,1.) ;
#9765 = VECTOR('',#36356,1.) ;
#9766 = VECTOR('',#36359,1.) ;
#9767 = VECTOR('',#36362,1.) ;
#9768 = VECTOR('',#36365,1.) ;
#9769 = VECTOR('',#36366,1.) ;
#9770 = VECTOR('',#36371,1.) ;
#9771 = VECTOR('',#36374,1.) ;
#9772 = VECTOR('',#36379,1.) ;
#9773 = VECTOR('',#36382,1.) ;
#9774 = VECTOR('',#36385,1.) ;
#9775 = VECTOR('',#36388,1.) ;
#9776 = VECTOR('',#36391,1.) ;
#9777 = VECTOR('',#36392,1.) ;
#9778 = VECTOR('',#36397,1.) ;
#9779 = VECTOR('',#36400,1.) ;
#9780 = VECTOR('',#36403,1.) ;
#9781 = VECTOR('',#36406,1.) ;
#9782 = VECTOR('',#36409,1.) ;
#9783 = VECTOR('',#36412,1.) ;
#9784 = VECTOR('',#36415,1.) ;
#9785 = VECTOR('',#36416,1.) ;
#9786 = VECTOR('',#36417,1.) ;
#9787 = VECTOR('',#36422,1.) ;
#9788 = VECTOR('',#36427,1.) ;
#9789 = VECTOR('',#36430,1.) ;
#9790 = VECTOR('',#36431,1.) ;
#9791 = VECTOR('',#36434,1.) ;
#9792 = VECTOR('',#36437,1.) ;
#9793 = VECTOR('',#36440,1.) ;
#9794 = VECTOR('',#36441,1.) ;
#9795 = VECTOR('',#36444,1.) ;
#9796 = VECTOR('',#36447,1.) ;
#9797 = VECTOR('',#36448,1.) ;
#9798 = VECTOR('',#36451,1.) ;
#9799 = VECTOR('',#36454,1.) ;
#9800 = VECTOR('',#36457,1.) ;
#9801 = VECTOR('',#36458,1.) ;
#9802 = VECTOR('',#36459,1.) ;
#9803 = VECTOR('',#36460,1.) ;
#9804 = VECTOR('',#36461,1.) ;
#9805 = VECTOR('',#36464,1.) ;
#9806 = VECTOR('',#36465,1.) ;
#9807 = VECTOR('',#36466,1.) ;
#9808 = VECTOR('',#36467,1.) ;
#9809 = VECTOR('',#36468,1.) ;
#9810 = VECTOR('',#36471,1.) ;
#9811 = VECTOR('',#36472,1.) ;
#9812 = VECTOR('',#36473,1.) ;
#9813 = VECTOR('',#36476,1.) ;
#9814 = VECTOR('',#36477,1.) ;
#9815 = VECTOR('',#36478,1.) ;
#9816 = VECTOR('',#36479,1.) ;
#9817 = VECTOR('',#36482,1.) ;
#9818 = VECTOR('',#36483,1.) ;
#9819 = VECTOR('',#36486,1.) ;
#9820 = VECTOR('',#36487,1.) ;
#9821 = VECTOR('',#36490,1.) ;
#9822 = VECTOR('',#36491,1.) ;
#9823 = VECTOR('',#36492,1.) ;
#9824 = VECTOR('',#36493,1.) ;
#9825 = VECTOR('',#36494,1.) ;
#9826 = VECTOR('',#36497,1.) ;
#9827 = VECTOR('',#36498,1.) ;
#9828 = VECTOR('',#36499,1.) ;
#9829 = VECTOR('',#36502,1.) ;
#9830 = VECTOR('',#36503,1.) ;
#9831 = VECTOR('',#36504,1.) ;
#9832 = VECTOR('',#36505,1.) ;
#9833 = VECTOR('',#36506,1.) ;
#9834 = VECTOR('',#36509,1.) ;
#9835 = VECTOR('',#36510,1.) ;
#9836 = VECTOR('',#36511,1.) ;
#9837 = VECTOR('',#36514,1.) ;
#9838 = VECTOR('',#36515,1.) ;
#9839 = VECTOR('',#36516,1.) ;
#9840 = VECTOR('',#36519,1.) ;
#9841 = VECTOR('',#36520,1.) ;
#9842 = VECTOR('',#36521,1.) ;
#9843 = VECTOR('',#36522,1.) ;
#9844 = VECTOR('',#36523,1.) ;
#9845 = VECTOR('',#36528,1.) ;
#9846 = VECTOR('',#36537,1.) ;
#9847 = VECTOR('',#36542,1.) ;
#9848 = VECTOR('',#36549,1.) ;
#9849 = VECTOR('',#36558,1.) ;
#9850 = VECTOR('',#36559,1.) ;
#9851 = VECTOR('',#36560,1.) ;
#9852 = VECTOR('',#36561,1.) ;
#9853 = VECTOR('',#36562,1.) ;
#9854 = VECTOR('',#36563,1.) ;
#9855 = VECTOR('',#36564,1.) ;
#9856 = VECTOR('',#36565,1.) ;
#9857 = VECTOR('',#36566,1.) ;
#9858 = VECTOR('',#36569,1.) ;
#9859 = VECTOR('',#36570,1.) ;
#9860 = VECTOR('',#36571,1.) ;
#9861 = VECTOR('',#36574,1.) ;
#9862 = VECTOR('',#36577,1.) ;
#9863 = VECTOR('',#36586,1.) ;
#9864 = VECTOR('',#36593,1.75) ;
#9865 = VECTOR('',#36594,1.) ;
#9866 = VECTOR('',#36597,1.) ;
#9867 = VECTOR('',#36598,1.) ;
#9868 = VECTOR('',#36605,1.) ;
#9869 = VECTOR('',#36606,1.) ;
#9870 = VECTOR('',#36609,1.) ;
#9871 = VECTOR('',#36610,1.) ;
#9872 = VECTOR('',#36613,1.) ;
#9873 = VECTOR('',#36618,1.) ;
#9874 = VECTOR('',#36623,1.) ;
#9875 = VECTOR('',#36624,1.) ;
#9876 = VECTOR('',#36627,1.) ;
#9877 = VECTOR('',#36634,1.75) ;
#9878 = VECTOR('',#36647,2.2) ;
#9879 = VECTOR('',#36656,1.75) ;
#9880 = VECTOR('',#36663,2.5) ;
#9881 = VECTOR('',#36676,1.) ;
#9882 = VECTOR('',#36679,1.) ;
#9883 = VECTOR('',#36682,1.) ;
#9884 = VECTOR('',#36683,1.) ;
#9885 = VECTOR('',#36684,1.) ;
#9886 = VECTOR('',#36685,1.) ;
#9887 = VECTOR('',#36686,1.) ;
#9888 = VECTOR('',#36689,1.) ;
#9889 = VECTOR('',#36690,1.) ;
#9890 = VECTOR('',#36691,1.) ;
#9891 = VECTOR('',#36694,1.) ;
#9892 = VECTOR('',#36695,1.) ;
#9893 = VECTOR('',#36696,1.) ;
#9894 = VECTOR('',#36697,1.) ;
#9895 = VECTOR('',#36702,1.) ;
#9896 = VECTOR('',#36705,1.) ;
#9897 = VECTOR('',#36710,1.) ;
#9898 = VECTOR('',#36713,1.) ;
#9899 = VECTOR('',#36716,1.) ;
#9900 = VECTOR('',#36717,1.) ;
#9901 = VECTOR('',#36718,1.) ;
#9902 = VECTOR('',#36721,1.) ;
#9903 = VECTOR('',#36722,1.) ;
#9904 = VECTOR('',#36723,1.) ;
#9905 = VECTOR('',#36724,1.) ;
#9906 = VECTOR('',#36727,1.) ;
#9907 = VECTOR('',#36728,1.) ;
#9908 = VECTOR('',#36729,1.) ;
#9909 = VECTOR('',#36732,1.) ;
#9910 = VECTOR('',#36733,1.) ;
#9911 = VECTOR('',#36738,1.) ;
#9912 = VECTOR('',#36741,1.) ;
#9913 = VECTOR('',#36750,1.5) ;
#9914 = VECTOR('',#36763,0.8) ;
#9915 = VECTOR('',#36772,1.5) ;
#9916 = VECTOR('',#36779,4.5) ;
#9917 = VECTOR('',#36792,0.61) ;
#9918 = VECTOR('',#36799,1.1) ;
#9919 = VECTOR('',#36810,0.81) ;
#9920 = VECTOR('',#36817,1.4) ;
#9921 = VECTOR('',#36828,0.6) ;
#9922 = VECTOR('',#36851,1.6) ;
#9923 = VECTOR('',#36856,1.) ;
#9924 = VECTOR('',#36859,1.) ;
#9925 = VECTOR('',#36862,1.) ;
#9926 = VECTOR('',#36865,1.) ;
#9927 = VECTOR('',#36868,1.) ;
#9928 = VECTOR('',#36871,1.) ;
#9929 = VECTOR('',#36876,1.) ;
#9930 = VECTOR('',#36879,1.) ;
#9931 = VECTOR('',#36882,1.) ;
#9932 = VECTOR('',#36885,1.) ;
#9933 = VECTOR('',#36888,1.) ;
#9934 = VECTOR('',#36891,1.) ;
#9935 = VECTOR('',#36894,1.) ;
#9936 = VECTOR('',#36897,1.) ;
#9937 = VECTOR('',#36900,1.) ;
#9938 = VECTOR('',#36903,1.) ;
#9939 = VECTOR('',#36906,1.) ;
#9940 = VECTOR('',#36909,1.) ;
#9941 = VECTOR('',#36912,1.) ;
#9942 = VECTOR('',#36917,1.) ;
#9943 = VECTOR('',#36918,1.) ;
#9944 = VECTOR('',#36919,1.) ;
#9945 = VECTOR('',#36922,1.) ;
#9946 = VECTOR('',#36923,1.) ;
#9947 = VECTOR('',#36926,1.) ;
#9948 = VECTOR('',#36927,1.) ;
#9949 = VECTOR('',#36930,1.) ;
#9950 = VECTOR('',#36931,1.) ;
#9951 = VECTOR('',#36932,1.) ;
#9952 = VECTOR('',#36935,1.) ;
#9953 = VECTOR('',#36938,1.) ;
#9954 = VECTOR('',#36939,1.) ;
#9955 = VECTOR('',#36942,1.) ;
#9956 = VECTOR('',#36943,1.) ;
#9957 = VECTOR('',#36948,1.) ;
#9958 = VECTOR('',#36953,1.) ;
#9959 = VECTOR('',#36954,1.) ;
#9960 = VECTOR('',#36955,1.) ;
#9961 = VECTOR('',#36958,1.) ;
#9962 = VECTOR('',#36959,1.) ;
#9963 = VECTOR('',#36962,1.) ;
#9964 = VECTOR('',#36963,1.) ;
#9965 = VECTOR('',#36966,1.) ;
#9966 = VECTOR('',#36967,1.) ;
#9967 = VECTOR('',#36968,1.) ;
#9968 = VECTOR('',#36971,1.) ;
#9969 = VECTOR('',#36974,1.) ;
#9970 = VECTOR('',#36975,1.) ;
#9971 = VECTOR('',#36978,1.) ;
#9972 = VECTOR('',#36979,1.) ;
#9973 = VECTOR('',#36982,1.) ;
#9974 = VECTOR('',#36989,1.) ;
#9975 = VECTOR('',#36990,1.) ;
#9976 = VECTOR('',#36991,1.) ;
#9977 = VECTOR('',#36994,1.) ;
#9978 = VECTOR('',#36995,1.) ;
#9979 = VECTOR('',#36998,1.) ;
#9980 = VECTOR('',#36999,1.) ;
#9981 = VECTOR('',#37002,1.) ;
#9982 = VECTOR('',#37003,1.) ;
#9983 = VECTOR('',#37004,1.) ;
#9984 = VECTOR('',#37007,1.) ;
#9985 = VECTOR('',#37010,1.) ;
#9986 = VECTOR('',#37011,1.) ;
#9987 = VECTOR('',#37014,1.) ;
#9988 = VECTOR('',#37015,1.) ;
#9989 = VECTOR('',#37020,1.) ;
#9990 = VECTOR('',#37025,1.) ;
#9991 = VECTOR('',#37026,1.) ;
#9992 = VECTOR('',#37027,1.) ;
#9993 = VECTOR('',#37030,1.) ;
#9994 = VECTOR('',#37031,1.) ;
#9995 = VECTOR('',#37034,1.) ;
#9996 = VECTOR('',#37035,1.) ;
#9997 = VECTOR('',#37038,1.) ;
#9998 = VECTOR('',#37039,1.) ;
#9999 = VECTOR('',#37040,1.) ;
#10000 = VECTOR('',#37043,1.) ;
#10001 = VECTOR('',#37046,1.) ;
#10002 = VECTOR('',#37047,1.) ;
#10003 = VECTOR('',#37050,1.) ;
#10004 = VECTOR('',#37051,1.) ;
#10005 = VECTOR('',#37054,1.) ;
#10006 = VECTOR('',#37061,1.) ;
#10007 = VECTOR('',#37074,1.) ;
#10008 = VECTOR('',#37081,1.6) ;
#10009 = VECTOR('',#37116,0.26) ;
#10010 = VECTOR('',#37121,1.) ;
#10011 = VECTOR('',#37122,1.) ;
#10012 = VECTOR('',#37123,1.) ;
#10013 = VECTOR('',#37124,1.) ;
#10014 = VECTOR('',#37127,1.) ;
#10015 = VECTOR('',#37128,1.) ;
#10016 = VECTOR('',#37129,1.) ;
#10017 = VECTOR('',#37132,1.) ;
#10018 = VECTOR('',#37133,1.) ;
#10019 = VECTOR('',#37134,1.) ;
#10020 = VECTOR('',#37135,1.) ;
#10021 = VECTOR('',#37138,1.) ;
#10022 = VECTOR('',#37139,1.) ;
#10023 = VECTOR('',#37140,1.) ;
#10024 = VECTOR('',#37143,1.) ;
#10025 = VECTOR('',#37146,1.) ;
#10026 = VECTOR('',#37147,1.) ;
#10027 = VECTOR('',#37150,1.) ;
#10028 = VECTOR('',#37155,0.41) ;
#10029 = VECTOR('',#37160,1.) ;
#10030 = VECTOR('',#37161,1.) ;
#10031 = VECTOR('',#37162,1.) ;
#10032 = VECTOR('',#37163,1.) ;
#10033 = VECTOR('',#37166,1.) ;
#10034 = VECTOR('',#37167,1.) ;
#10035 = VECTOR('',#37168,1.) ;
#10036 = VECTOR('',#37171,1.) ;
#10037 = VECTOR('',#37172,1.) ;
#10038 = VECTOR('',#37175,1.) ;
#10039 = VECTOR('',#37176,1.) ;
#10040 = VECTOR('',#37179,1.) ;
#10041 = VECTOR('',#37184,0.425) ;
#10042 = VECTOR('',#37191,0.425) ;
#10043 = VECTOR('',#37198,0.425) ;
#10044 = VECTOR('',#37205,0.425) ;
#10045 = VECTOR('',#37212,1.05) ;
#10046 = VECTOR('',#37215,1.) ;
#10047 = VECTOR('',#37218,1.) ;
#10048 = VECTOR('',#37223,1.) ;
#10049 = VECTOR('',#37224,1.) ;
#10050 = VECTOR('',#37225,1.) ;
#10051 = VECTOR('',#37226,1.) ;
#10052 = VECTOR('',#37227,1.) ;
#10053 = VECTOR('',#37228,1.) ;
#10054 = VECTOR('',#37229,1.) ;
#10055 = VECTOR('',#37236,1.) ;
#10056 = VECTOR('',#37237,1.) ;
#10057 = VECTOR('',#37238,1.) ;
#10058 = VECTOR('',#37239,1.) ;
#10059 = VECTOR('',#37240,1.) ;
#10060 = VECTOR('',#37241,1.) ;
#10061 = VECTOR('',#37242,1.) ;
#10062 = VECTOR('',#37245,1.) ;
#10063 = VECTOR('',#37246,1.) ;
#10064 = VECTOR('',#37251,1.) ;
#10065 = VECTOR('',#37252,1.) ;
#10066 = VECTOR('',#37253,1.) ;
#10067 = VECTOR('',#37254,1.) ;
#10068 = VECTOR('',#37255,1.) ;
#10069 = VECTOR('',#37258,1.) ;
#10070 = VECTOR('',#37259,1.) ;
#10071 = VECTOR('',#37262,1.) ;
#10072 = VECTOR('',#37265,1.) ;
#10073 = VECTOR('',#37266,1.) ;
#10074 = VECTOR('',#37269,1.) ;
#10075 = VECTOR('',#37272,1.) ;
#10076 = VECTOR('',#37273,1.) ;
#10077 = VECTOR('',#37274,1.) ;
#10078 = VECTOR('',#37275,1.) ;
#10079 = VECTOR('',#37278,1.) ;
#10080 = VECTOR('',#37281,1.) ;
#10081 = VECTOR('',#37284,1.) ;
#10082 = VECTOR('',#37287,1.) ;
#10083 = VECTOR('',#37290,1.) ;
#10084 = VECTOR('',#37293,1.) ;
#10085 = VECTOR('',#37294,1.) ;
#10086 = VECTOR('',#37295,1.) ;
#10087 = VECTOR('',#37296,1.) ;
#10088 = VECTOR('',#37303,1.) ;
#10089 = VECTOR('',#37304,1.) ;
#10090 = VECTOR('',#37307,1.) ;
#10091 = VECTOR('',#37310,1.) ;
#10092 = VECTOR('',#37317,1.) ;
#10093 = VECTOR('',#37318,1.) ;
#10094 = VECTOR('',#37319,1.) ;
#10095 = VECTOR('',#37320,1.) ;
#10096 = VECTOR('',#37323,1.) ;
#10097 = VECTOR('',#37324,1.) ;
#10098 = VECTOR('',#37325,1.) ;
#10099 = VECTOR('',#37328,1.) ;
#10100 = VECTOR('',#37329,1.) ;
#10101 = VECTOR('',#37330,1.) ;
#10102 = VECTOR('',#37331,1.) ;
#10103 = VECTOR('',#37334,1.) ;
#10104 = VECTOR('',#37335,1.) ;
#10105 = VECTOR('',#37336,1.) ;
#10106 = VECTOR('',#37337,1.) ;
#10107 = VECTOR('',#37340,1.) ;
#10108 = VECTOR('',#37341,1.) ;
#10109 = VECTOR('',#37342,1.) ;
#10110 = VECTOR('',#37345,1.) ;
#10111 = VECTOR('',#37346,1.) ;
#10112 = VECTOR('',#37353,0.25) ;
#10113 = VECTOR('',#37358,1.) ;
#10114 = VECTOR('',#37359,1.) ;
#10115 = VECTOR('',#37360,1.) ;
#10116 = VECTOR('',#37361,1.) ;
#10117 = VECTOR('',#37364,1.) ;
#10118 = VECTOR('',#37365,1.) ;
#10119 = VECTOR('',#37366,1.) ;
#10120 = VECTOR('',#37367,1.) ;
#10121 = VECTOR('',#37370,1.) ;
#10122 = VECTOR('',#37371,1.) ;
#10123 = VECTOR('',#37374,1.) ;
#10124 = VECTOR('',#37375,1.) ;
#10125 = VECTOR('',#37376,1.) ;
#10126 = VECTOR('',#37379,1.) ;
#10127 = VECTOR('',#37380,1.) ;
#10128 = VECTOR('',#37381,1.) ;
#10129 = VECTOR('',#37386,0.3) ;
#10130 = VECTOR('',#37391,1.) ;
#10131 = VECTOR('',#37392,1.) ;
#10132 = VECTOR('',#37393,1.) ;
#10133 = VECTOR('',#37394,1.) ;
#10134 = VECTOR('',#37397,1.) ;
#10135 = VECTOR('',#37398,1.) ;
#10136 = VECTOR('',#37399,1.) ;
#10137 = VECTOR('',#37402,1.) ;
#10138 = VECTOR('',#37403,1.) ;
#10139 = VECTOR('',#37404,1.) ;
#10140 = VECTOR('',#37407,1.) ;
#10141 = VECTOR('',#37408,1.) ;
#10142 = VECTOR('',#37409,1.) ;
#10143 = VECTOR('',#37412,1.) ;
#10144 = VECTOR('',#37413,1.) ;
#10145 = VECTOR('',#37414,1.) ;
#10146 = VECTOR('',#37419,4.5) ;
#10147 = VECTOR('',#37424,1.) ;
#10148 = VECTOR('',#37425,1.) ;
#10149 = VECTOR('',#37428,1.) ;
#10150 = VECTOR('',#37429,1.) ;
#10151 = VECTOR('',#37438,1.) ;
#10152 = VECTOR('',#37439,1.) ;
#10153 = VECTOR('',#37440,1.) ;
#10154 = VECTOR('',#37441,1.) ;
#10155 = VECTOR('',#37444,1.) ;
#10156 = VECTOR('',#37445,1.) ;
#10157 = VECTOR('',#37446,1.) ;
#10158 = VECTOR('',#37449,1.) ;
#10159 = VECTOR('',#37450,1.) ;
#10160 = VECTOR('',#37453,1.) ;
#10161 = VECTOR('',#37454,1.) ;
#10162 = VECTOR('',#37457,1.) ;
#10163 = VECTOR('',#37458,1.) ;
#10164 = VECTOR('',#37459,1.) ;
#10165 = VECTOR('',#37460,1.) ;
#10166 = VECTOR('',#37461,1.) ;
#10167 = VECTOR('',#37462,1.) ;
#10168 = VECTOR('',#37463,1.) ;
#10169 = VECTOR('',#37464,1.) ;
#10170 = VECTOR('',#37465,1.) ;
#10171 = VECTOR('',#37466,1.) ;
#10172 = VECTOR('',#37467,1.) ;
#10173 = VECTOR('',#37468,1.) ;
#10174 = VECTOR('',#37469,1.) ;
#10175 = VECTOR('',#37470,1.) ;
#10176 = VECTOR('',#37471,1.) ;
#10177 = VECTOR('',#37472,1.) ;
#10178 = VECTOR('',#37473,1.) ;
#10179 = VECTOR('',#37474,1.) ;
#10180 = VECTOR('',#37475,1.) ;
#10181 = VECTOR('',#37476,1.) ;
#10182 = VECTOR('',#37477,1.) ;
#10183 = VECTOR('',#37478,1.) ;
#10184 = VECTOR('',#37479,1.) ;
#10185 = VECTOR('',#37480,1.) ;
#10186 = VECTOR('',#37481,1.) ;
#10187 = VECTOR('',#37482,1.) ;
#10188 = VECTOR('',#37483,1.) ;
#10189 = VECTOR('',#37484,1.) ;
#10190 = VECTOR('',#37485,1.) ;
#10191 = VECTOR('',#37486,1.) ;
#10192 = VECTOR('',#37487,1.) ;
#10193 = VECTOR('',#37488,1.) ;
#10194 = VECTOR('',#37489,1.) ;
#10195 = VECTOR('',#37490,1.) ;
#10196 = VECTOR('',#37491,1.) ;
#10197 = VECTOR('',#37492,1.) ;
#10198 = VECTOR('',#37493,1.) ;
#10199 = VECTOR('',#37496,1.) ;
#10200 = VECTOR('',#37497,1.) ;
#10201 = VECTOR('',#37498,1.) ;
#10202 = VECTOR('',#37499,1.) ;
#10203 = VECTOR('',#37502,1.) ;
#10204 = VECTOR('',#37503,1.) ;
#10205 = VECTOR('',#37506,1.) ;
#10206 = VECTOR('',#37509,1.) ;
#10207 = VECTOR('',#37512,1.) ;
#10208 = VECTOR('',#37513,1.) ;
#10209 = VECTOR('',#37514,1.) ;
#10210 = VECTOR('',#37515,1.) ;
#10211 = VECTOR('',#37516,1.) ;
#10212 = VECTOR('',#37517,1.) ;
#10213 = VECTOR('',#37518,1.) ;
#10214 = VECTOR('',#37519,1.) ;
#10215 = VECTOR('',#37520,1.) ;
#10216 = VECTOR('',#37521,1.) ;
#10217 = VECTOR('',#37522,1.) ;
#10218 = VECTOR('',#37523,1.) ;
#10219 = VECTOR('',#37524,1.) ;
#10220 = VECTOR('',#37525,1.) ;
#10221 = VECTOR('',#37526,1.) ;
#10222 = VECTOR('',#37527,1.) ;
#10223 = VECTOR('',#37528,1.) ;
#10224 = VECTOR('',#37529,1.) ;
#10225 = VECTOR('',#37530,1.) ;
#10226 = VECTOR('',#37531,1.) ;
#10227 = VECTOR('',#37532,1.) ;
#10228 = VECTOR('',#37533,1.) ;
#10229 = VECTOR('',#37534,1.) ;
#10230 = VECTOR('',#37535,1.) ;
#10231 = VECTOR('',#37538,1.) ;
#10232 = VECTOR('',#37539,1.) ;
#10233 = VECTOR('',#37540,1.) ;
#10234 = VECTOR('',#37543,1.) ;
#10235 = VECTOR('',#37546,1.) ;
#10236 = VECTOR('',#37551,1.) ;
#10237 = VECTOR('',#37552,1.) ;
#10238 = VECTOR('',#37553,1.) ;
#10239 = VECTOR('',#37556,1.) ;
#10240 = VECTOR('',#37559,1.) ;
#10241 = VECTOR('',#37564,1.) ;
#10242 = VECTOR('',#37565,1.) ;
#10243 = VECTOR('',#37566,1.) ;
#10244 = VECTOR('',#37569,1.) ;
#10245 = VECTOR('',#37572,1.) ;
#10246 = VECTOR('',#37577,1.) ;
#10247 = VECTOR('',#37578,1.) ;
#10248 = VECTOR('',#37579,1.) ;
#10249 = VECTOR('',#37582,1.) ;
#10250 = VECTOR('',#37585,1.) ;
#10251 = VECTOR('',#37590,1.) ;
#10252 = VECTOR('',#37591,1.) ;
#10253 = VECTOR('',#37592,1.) ;
#10254 = VECTOR('',#37595,1.) ;
#10255 = VECTOR('',#37598,1.) ;
#10256 = VECTOR('',#37603,1.) ;
#10257 = VECTOR('',#37604,1.) ;
#10258 = VECTOR('',#37605,1.) ;
#10259 = VECTOR('',#37608,1.) ;
#10260 = VECTOR('',#37611,1.) ;
#10261 = VECTOR('',#37616,1.) ;
#10262 = VECTOR('',#37617,1.) ;
#10263 = VECTOR('',#37618,1.) ;
#10264 = VECTOR('',#37621,1.) ;
#10265 = VECTOR('',#37624,1.) ;
#10266 = VECTOR('',#37629,1.) ;
#10267 = VECTOR('',#37630,1.) ;
#10268 = VECTOR('',#37631,1.) ;
#10269 = VECTOR('',#37634,1.) ;
#10270 = VECTOR('',#37637,1.) ;
#10271 = VECTOR('',#37646,0.425) ;
#10272 = VECTOR('',#37653,0.425) ;
#10273 = VECTOR('',#37660,0.425) ;
#10274 = VECTOR('',#37667,0.425) ;
#10275 = VECTOR('',#37672,1.) ;
#10276 = VECTOR('',#37675,1.) ;
#10277 = VECTOR('',#37680,1.) ;
#10278 = VECTOR('',#37681,1.) ;
#10279 = VECTOR('',#37682,1.) ;
#10280 = VECTOR('',#37683,1.) ;
#10281 = VECTOR('',#37696,9.) ;
#10282 = VECTOR('',#37703,1.) ;
#10283 = VECTOR('',#37704,1.) ;
#10284 = VECTOR('',#37705,1.) ;
#10285 = VECTOR('',#37706,1.) ;
#10286 = VECTOR('',#37709,1.) ;
#10287 = VECTOR('',#37710,1.) ;
#10288 = VECTOR('',#37713,1.) ;
#10289 = VECTOR('',#37716,1.) ;
#10290 = VECTOR('',#37721,8.7) ;
#10291 = VECTOR('',#37732,6.3) ;
#10292 = VECTOR('',#37737,6.3) ;
#10293 = VECTOR('',#37744,6.8) ;
#10294 = VECTOR('',#37765,4.65) ;
#10295 = VECTOR('',#37768,4.45) ;
#10296 = VECTOR('',#37775,0.4) ;
#10297 = VECTOR('',#37782,0.4) ;
#10298 = VECTOR('',#37789,0.4) ;
#10299 = VECTOR('',#37796,0.4) ;
#10300 = VECTOR('',#37803,0.4) ;
#10301 = VECTOR('',#37810,0.4) ;
#10302 = VECTOR('',#37817,0.4) ;
#10303 = VECTOR('',#37824,0.51) ;
#10304 = VECTOR('',#37829,1.) ;
#10305 = VECTOR('',#37830,1.) ;
#10306 = VECTOR('',#37831,1.) ;
#10307 = VECTOR('',#37832,1.) ;
#10308 = VECTOR('',#37851,0.4) ;
#10309 = VECTOR('',#37858,1.) ;
#10310 = VECTOR('',#37859,1.) ;
#10311 = VECTOR('',#37860,1.) ;
#10312 = VECTOR('',#37863,1.) ;
#10313 = VECTOR('',#37864,1.) ;
#10314 = VECTOR('',#37865,1.) ;
#10315 = VECTOR('',#37870,0.31) ;
#10316 = VECTOR('',#37883,0.15) ;
#10317 = VECTOR('',#37888,0.51) ;
#10318 = VECTOR('',#37893,1.) ;
#10319 = VECTOR('',#37894,1.) ;
#10320 = VECTOR('',#37895,1.) ;
#10321 = VECTOR('',#37896,1.) ;
#10322 = VECTOR('',#37897,1.) ;
#10323 = VECTOR('',#37898,1.) ;
#10324 = VECTOR('',#37899,1.) ;
#10325 = VECTOR('',#37900,1.) ;
#10326 = VECTOR('',#37903,1.) ;
#10327 = VECTOR('',#37904,1.) ;
#10328 = VECTOR('',#37905,1.) ;
#10329 = VECTOR('',#37906,1.) ;
#10330 = VECTOR('',#37907,1.) ;
#10331 = VECTOR('',#37908,1.) ;
#10332 = VECTOR('',#37909,1.) ;
#10333 = VECTOR('',#37912,1.) ;
#10334 = VECTOR('',#37913,1.) ;
#10335 = VECTOR('',#37916,1.) ;
#10336 = VECTOR('',#37919,1.) ;
#10337 = VECTOR('',#37924,1.) ;
#10338 = VECTOR('',#37925,1.) ;
#10339 = VECTOR('',#37928,1.) ;
#10340 = VECTOR('',#37929,1.) ;
#10341 = VECTOR('',#37932,1.) ;
#10342 = VECTOR('',#37937,1.) ;
#10343 = VECTOR('',#37938,1.) ;
#10344 = VECTOR('',#37939,1.) ;
#10345 = VECTOR('',#37942,1.) ;
#10346 = VECTOR('',#37943,1.) ;
#10347 = VECTOR('',#37946,1.) ;
#10348 = VECTOR('',#37947,1.) ;
#10349 = VECTOR('',#37950,1.) ;
#10350 = VECTOR('',#37959,0.7) ;
#10351 = VECTOR('',#37978,0.8) ;
#10352 = VECTOR('',#37987,0.5) ;
#10353 = VECTOR('',#38012,0.15) ;
#10354 = VECTOR('',#38049,0.15) ;
#10355 = VECTOR('',#38054,0.15) ;
#10356 = VECTOR('',#38061,0.4) ;
#10357 = VECTOR('',#38074,0.4) ;
#10358 = VECTOR('',#38083,0.4) ;
#10359 = VECTOR('',#38088,0.4) ;
#10360 = VECTOR('',#38097,0.4) ;
#10361 = VECTOR('',#38106,0.4) ;
#10362 = VECTOR('',#38131,0.15) ;
#10363 = VECTOR('',#38154,0.15) ;
#10364 = VECTOR('',#38179,0.15) ;
#10365 = VECTOR('',#38198,0.125) ;
#10366 = VECTOR('',#38211,1.) ;
#10367 = VECTOR('',#38212,1.) ;
#10368 = VECTOR('',#38213,1.) ;
#10369 = VECTOR('',#38222,0.125) ;
#10370 = VECTOR('',#38231,0.125) ;
#10371 = VECTOR('',#38244,0.29) ;
#10372 = VECTOR('',#38257,0.29) ;
#10373 = VECTOR('',#38270,0.55) ;
#10374 = VECTOR('',#38277,0.25) ;
#10375 = VECTOR('',#38288,0.15) ;
#10376 = VECTOR('',#38295,0.8) ;
#10377 = VECTOR('',#38302,1.1) ;
#10378 = VECTOR('',#38315,0.8) ;
#10379 = VECTOR('',#38322,1.1) ;
#10380 = VECTOR('',#38327,1.) ;
#10381 = VECTOR('',#39492,0.15) ;
#10382 = VECTOR('',#39499,0.15) ;
#10383 = VECTOR('',#39506,0.15) ;
#10384 = VECTOR('',#39513,0.15) ;
#10385 = VECTOR('',#39520,0.15) ;
#10386 = VECTOR('',#39527,0.15) ;
#10387 = VECTOR('',#39534,0.15) ;
#10388 = VECTOR('',#39541,0.15) ;
#10389 = VECTOR('',#39548,0.15) ;
#10390 = VECTOR('',#39555,0.15) ;
#10391 = VECTOR('',#39562,0.15) ;
#10392 = VECTOR('',#39569,0.15) ;
#10393 = VECTOR('',#39576,0.15) ;
#10394 = VECTOR('',#39583,0.15) ;
#10395 = VECTOR('',#39590,0.15) ;
#10396 = VECTOR('',#39597,0.15) ;
#10397 = VECTOR('',#39604,0.15) ;
#10398 = VECTOR('',#39611,0.15) ;
#10399 = VECTOR('',#39618,0.15) ;
#10400 = VECTOR('',#39625,0.15) ;
#10401 = VECTOR('',#39632,0.15) ;
#10402 = VECTOR('',#39639,0.15) ;
#10403 = VECTOR('',#39646,0.15) ;
#10404 = VECTOR('',#39653,0.15) ;
#10405 = VECTOR('',#39660,0.15) ;
#10406 = VECTOR('',#39667,0.15) ;
#10407 = VECTOR('',#39674,0.15) ;
#10408 = VECTOR('',#39681,0.15) ;
#10409 = VECTOR('',#39688,0.15) ;
#10410 = VECTOR('',#39695,0.15) ;
#10411 = VECTOR('',#39702,0.15) ;
#10412 = VECTOR('',#39709,0.15) ;
#10413 = VECTOR('',#39716,0.15) ;
#10414 = VECTOR('',#39723,0.15) ;
#10415 = VECTOR('',#39730,0.15) ;
#10416 = VECTOR('',#39737,0.15) ;
#10417 = VECTOR('',#39744,0.15) ;
#10418 = VECTOR('',#39751,0.15) ;
#10419 = VECTOR('',#39758,0.15) ;
#10420 = VECTOR('',#39765,0.15) ;
#10421 = VECTOR('',#39772,0.15) ;
#10422 = VECTOR('',#39779,0.15) ;
#10423 = VECTOR('',#39786,0.15) ;
#10424 = VECTOR('',#39793,0.15) ;
#10425 = VECTOR('',#39800,0.15) ;
#10426 = VECTOR('',#39807,0.15) ;
#10427 = VECTOR('',#39814,0.15) ;
#10428 = VECTOR('',#39821,0.15) ;
#10429 = VECTOR('',#39828,0.15) ;
#10430 = VECTOR('',#39835,0.15) ;
#10431 = VECTOR('',#39842,0.15) ;
#10432 = VECTOR('',#39849,0.15) ;
#10433 = VECTOR('',#39856,0.15) ;
#10434 = VECTOR('',#39863,0.15) ;
#10435 = VECTOR('',#39870,0.15) ;
#10436 = VECTOR('',#39877,0.15) ;
#10437 = VECTOR('',#39884,0.15) ;
#10438 = VECTOR('',#39891,0.15) ;
#10439 = VECTOR('',#39898,0.15) ;
#10440 = VECTOR('',#39905,0.15) ;
#10441 = VECTOR('',#39912,0.15) ;
#10442 = VECTOR('',#39919,0.15) ;
#10443 = VECTOR('',#39926,0.15) ;
#10444 = VECTOR('',#39933,0.15) ;
#10445 = VECTOR('',#39940,0.15) ;
#10446 = VECTOR('',#39947,0.15) ;
#10447 = VECTOR('',#39954,0.15) ;
#10448 = VECTOR('',#39961,0.15) ;
#10449 = VECTOR('',#39968,0.15) ;
#10450 = VECTOR('',#39975,0.15) ;
#10451 = VECTOR('',#39982,0.15) ;
#10452 = VECTOR('',#39989,0.15) ;
#10453 = VECTOR('',#39996,0.15) ;
#10454 = VECTOR('',#40003,0.15) ;
#10455 = VECTOR('',#40010,0.15) ;
#10456 = VECTOR('',#40017,0.15) ;
#10457 = VECTOR('',#40024,0.15) ;
#10458 = VECTOR('',#40031,0.15) ;
#10459 = VECTOR('',#40038,0.15) ;
#10460 = VECTOR('',#40045,0.15) ;
#10461 = VECTOR('',#40052,0.15) ;
#10462 = VECTOR('',#40059,0.15) ;
#10463 = VECTOR('',#40066,0.15) ;
#10464 = VECTOR('',#40073,0.15) ;
#10465 = VECTOR('',#40080,0.15) ;
#10466 = VECTOR('',#40087,0.15) ;
#10467 = VECTOR('',#40094,0.15) ;
#10468 = VECTOR('',#40101,0.15) ;
#10469 = VECTOR('',#40108,0.15) ;
#10470 = VECTOR('',#40115,0.15) ;
#10471 = VECTOR('',#40122,0.15) ;
#10472 = VECTOR('',#40129,0.15) ;
#10473 = VECTOR('',#40136,0.15) ;
#10474 = VECTOR('',#40143,0.15) ;
#10475 = VECTOR('',#40150,0.15) ;
#10476 = VECTOR('',#40157,0.15) ;
#10477 = VECTOR('',#40164,0.15) ;
#10478 = VECTOR('',#40171,0.15) ;
#10479 = VECTOR('',#40178,0.15) ;
#10480 = VECTOR('',#40185,0.15) ;
#10481 = VECTOR('',#40192,0.15) ;
#10482 = VECTOR('',#40199,0.15) ;
#10483 = VECTOR('',#40206,0.15) ;
#10484 = VECTOR('',#40213,0.15) ;
#10485 = VECTOR('',#40220,0.15) ;
#10486 = VECTOR('',#40227,0.15) ;
#10487 = VECTOR('',#40234,0.15) ;
#10488 = VECTOR('',#40241,0.15) ;
#10489 = VECTOR('',#40248,0.15) ;
#10490 = VECTOR('',#40255,0.15) ;
#10491 = VECTOR('',#40262,0.15) ;
#10492 = VECTOR('',#40269,0.15) ;
#10493 = VECTOR('',#40276,0.15) ;
#10494 = VECTOR('',#40283,0.15) ;
#10495 = VECTOR('',#40290,0.15) ;
#10496 = VECTOR('',#40297,0.15) ;
#10497 = VECTOR('',#40304,0.15) ;
#10498 = VECTOR('',#40311,0.15) ;
#10499 = VECTOR('',#40318,0.15) ;
#10500 = VECTOR('',#40325,0.15) ;
#10501 = VECTOR('',#40332,0.15) ;
#10502 = VECTOR('',#40339,0.15) ;
#10503 = VECTOR('',#40346,0.15) ;
#10504 = VECTOR('',#40353,0.15) ;
#10505 = VECTOR('',#40360,0.15) ;
#10506 = VECTOR('',#40367,0.15) ;
#10507 = VECTOR('',#40376,0.55) ;
#10508 = VECTOR('',#40377,0.55) ;
#10509 = VECTOR('',#40384,0.25) ;
#10510 = VECTOR('',#40393,0.15) ;
#10511 = VECTOR('',#40462,3.5) ;
#10512 = VECTOR('',#40477,3.5) ;
#10513 = VECTOR('',#40486,3.3) ;
#10514 = VECTOR('',#40491,3.3) ;
#10515 = VECTOR('',#40510,0.6) ;
#10516 = VECTOR('',#40517,1.) ;
#10517 = VECTOR('',#40518,1.) ;
#10518 = VECTOR('',#40519,1.) ;
#10519 = VECTOR('',#40520,1.) ;
#10520 = VECTOR('',#40523,1.) ;
#10521 = VECTOR('',#40524,1.) ;
#10522 = VECTOR('',#40525,1.) ;
#10523 = VECTOR('',#40526,1.) ;
#10524 = VECTOR('',#40529,1.) ;
#10525 = VECTOR('',#40530,1.) ;
#10526 = VECTOR('',#40531,1.) ;
#10527 = VECTOR('',#40532,1.) ;
#10528 = VECTOR('',#40535,1.) ;
#10529 = VECTOR('',#40536,1.) ;
#10530 = VECTOR('',#40541,1.) ;
#10531 = VECTOR('',#40550,1.) ;
#10532 = VECTOR('',#40555,1.) ;
#10533 = VECTOR('',#40556,1.) ;
#10534 = VECTOR('',#40563,0.32) ;
#10535 = VECTOR('',#40566,0.32) ;
#10536 = VECTOR('',#40569,1.) ;
#10537 = VECTOR('',#40576,1.) ;
#10538 = VECTOR('',#40577,1.) ;
#10539 = VECTOR('',#40586,4.5) ;
#10540 = VECTOR('',#40587,1.) ;
#10541 = VECTOR('',#40588,4.5) ;
#10542 = VECTOR('',#40591,4.5) ;
#10543 = VECTOR('',#40592,1.) ;
#10544 = VECTOR('',#40593,4.5) ;
#10545 = VECTOR('',#40596,1.) ;
#10546 = VECTOR('',#40613,3.5) ;
#10547 = VECTOR('',#40620,1.) ;
#10548 = VECTOR('',#40627,1.02) ;
#10549 = VECTOR('',#40638,1.) ;
#10550 = VECTOR('',#40641,1.) ;
#10551 = VECTOR('',#40646,1.) ;
#10552 = VECTOR('',#40647,1.) ;
#10553 = VECTOR('',#40648,1.) ;
#10554 = VECTOR('',#40649,1.) ;
#10555 = VECTOR('',#40650,1.) ;
#10556 = VECTOR('',#40653,1.) ;
#10557 = VECTOR('',#40654,1.) ;
#10558 = VECTOR('',#40657,1.) ;
#10559 = VECTOR('',#40658,1.) ;
#10560 = VECTOR('',#40661,1.) ;
#10561 = VECTOR('',#40662,1.) ;
#10562 = VECTOR('',#40663,1.) ;
#10563 = VECTOR('',#40666,1.) ;
#10564 = VECTOR('',#40669,1.) ;
#10565 = VECTOR('',#40674,1.) ;
#10566 = VECTOR('',#40675,1.) ;
#10567 = VECTOR('',#40676,1.) ;
#10568 = VECTOR('',#40677,1.) ;
#10569 = VECTOR('',#40680,1.) ;
#10570 = VECTOR('',#40681,1.) ;
#10571 = VECTOR('',#40682,1.) ;
#10572 = VECTOR('',#40683,1.) ;
#10573 = VECTOR('',#40686,1.) ;
#10574 = VECTOR('',#40687,1.) ;
#10575 = VECTOR('',#40690,1.) ;
#10576 = VECTOR('',#40693,1.) ;
#10577 = VECTOR('',#40700,1.) ;
#10578 = VECTOR('',#40701,1.) ;
#10579 = VECTOR('',#40702,1.) ;
#10580 = VECTOR('',#40703,1.) ;
#10581 = VECTOR('',#40704,1.) ;
#10582 = VECTOR('',#40705,1.) ;
#10583 = VECTOR('',#40710,1.) ;
#10584 = VECTOR('',#40711,1.) ;
#10585 = VECTOR('',#40714,1.) ;
#10586 = VECTOR('',#40715,1.) ;
#10587 = VECTOR('',#40718,1.) ;
#10588 = VECTOR('',#40719,1.) ;
#10589 = VECTOR('',#40720,1.) ;
#10590 = VECTOR('',#40723,1.) ;
#10591 = VECTOR('',#40726,1.) ;
#10592 = VECTOR('',#40727,1.) ;
#10593 = VECTOR('',#40738,3.5) ;
#10594 = VECTOR('',#40745,3.8) ;
#10595 = VECTOR('',#40768,0.6) ;
#10596 = VECTOR('',#40775,1.) ;
#10597 = VECTOR('',#40776,1.) ;
#10598 = VECTOR('',#40777,1.) ;
#10599 = VECTOR('',#40778,1.) ;
#10600 = VECTOR('',#40781,1.) ;
#10601 = VECTOR('',#40782,1.) ;
#10602 = VECTOR('',#40783,1.) ;
#10603 = VECTOR('',#40784,1.) ;
#10604 = VECTOR('',#40787,1.) ;
#10605 = VECTOR('',#40788,1.) ;
#10606 = VECTOR('',#40789,1.) ;
#10607 = VECTOR('',#40790,1.) ;
#10608 = VECTOR('',#40793,1.) ;
#10609 = VECTOR('',#40794,1.) ;
#10610 = VECTOR('',#40797,1.) ;
#10611 = VECTOR('',#40798,1.) ;
#10612 = VECTOR('',#40801,1.) ;
#10613 = VECTOR('',#40804,1.) ;
#10614 = VECTOR('',#40813,0.6) ;
#10615 = VECTOR('',#40818,1.) ;
#10616 = VECTOR('',#40819,1.) ;
#10617 = VECTOR('',#40820,1.) ;
#10618 = VECTOR('',#40821,1.) ;
#10619 = VECTOR('',#40824,1.) ;
#10620 = VECTOR('',#40825,1.) ;
#10621 = VECTOR('',#40826,1.) ;
#10622 = VECTOR('',#40827,1.) ;
#10623 = VECTOR('',#40830,1.) ;
#10624 = VECTOR('',#40831,1.) ;
#10625 = VECTOR('',#40832,1.) ;
#10626 = VECTOR('',#40833,1.) ;
#10627 = VECTOR('',#40836,1.) ;
#10628 = VECTOR('',#40837,1.) ;
#10629 = VECTOR('',#40840,1.) ;
#10630 = VECTOR('',#40841,1.) ;
#10631 = VECTOR('',#40844,1.) ;
#10632 = VECTOR('',#40847,1.) ;
#10633 = VECTOR('',#40856,0.4) ;
#10634 = VECTOR('',#40863,1.) ;
#10635 = VECTOR('',#40864,1.) ;
#10636 = VECTOR('',#40865,1.) ;
#10637 = VECTOR('',#40866,1.) ;
#10638 = VECTOR('',#40869,1.) ;
#10639 = VECTOR('',#40870,1.) ;
#10640 = VECTOR('',#40871,1.) ;
#10641 = VECTOR('',#40872,1.) ;
#10642 = VECTOR('',#40875,1.) ;
#10643 = VECTOR('',#40876,1.) ;
#10644 = VECTOR('',#40877,1.) ;
#10645 = VECTOR('',#40878,1.) ;
#10646 = VECTOR('',#40881,1.) ;
#10647 = VECTOR('',#40882,1.) ;
#10648 = VECTOR('',#40885,1.) ;
#10649 = VECTOR('',#40886,1.) ;
#10650 = VECTOR('',#40889,1.) ;
#10651 = VECTOR('',#40892,1.) ;
#10652 = VECTOR('',#40901,0.5) ;
#10653 = VECTOR('',#40906,1.) ;
#10654 = VECTOR('',#40907,1.) ;
#10655 = VECTOR('',#40908,1.) ;
#10656 = VECTOR('',#40909,1.) ;
#10657 = VECTOR('',#40912,1.) ;
#10658 = VECTOR('',#40913,1.) ;
#10659 = VECTOR('',#40914,1.) ;
#10660 = VECTOR('',#40915,1.) ;
#10661 = VECTOR('',#40918,1.) ;
#10662 = VECTOR('',#40919,1.) ;
#10663 = VECTOR('',#40920,1.) ;
#10664 = VECTOR('',#40921,1.) ;
#10665 = VECTOR('',#40924,1.) ;
#10666 = VECTOR('',#40925,1.) ;
#10667 = VECTOR('',#40928,1.) ;
#10668 = VECTOR('',#40929,1.) ;
#10669 = VECTOR('',#40932,1.) ;
#10670 = VECTOR('',#40935,1.) ;
#10671 = VECTOR('',#40950,0.45) ;
#10672 = VECTOR('',#40955,0.245) ;
#10673 = VECTOR('',#40972,0.45) ;
#10674 = VECTOR('',#40977,0.245) ;
#10675 = VECTOR('',#40992,0.25) ;
#10676 = VECTOR('',#41095,0.25) ;
#10677 = VECTOR('',#41102,0.25) ;
#10678 = VECTOR('',#41109,0.25) ;
#10679 = VECTOR('',#41116,0.25) ;
#10680 = VECTOR('',#41121,0.25) ;
#10681 = VECTOR('',#41126,0.25) ;
#10682 = VECTOR('',#41131,0.25) ;
#10683 = VECTOR('',#41136,0.25) ;
#10684 = VECTOR('',#41141,0.25) ;
#10685 = VECTOR('',#41148,0.25) ;
#10686 = VECTOR('',#41155,0.25) ;
#10687 = VECTOR('',#41162,0.3) ;
#10688 = CIRCLE('',#29215,0.62) ;
#10689 = CIRCLE('',#29216,0.62) ;
#10690 = CIRCLE('',#29222,55.) ;
#10691 = CIRCLE('',#29227,55.) ;
#10692 = CIRCLE('',#29228,55.) ;
#10693 = CIRCLE('',#29229,55.) ;
#10694 = CIRCLE('',#29230,55.) ;
#10695 = CIRCLE('',#29231,55.) ;
#10696 = CIRCLE('',#29233,0.62) ;
#10697 = CIRCLE('',#29234,0.62) ;
#10698 = CIRCLE('',#29244,28.7741935483871) ;
#10699 = CIRCLE('',#29249,27.9516129032258) ;
#10700 = CIRCLE('',#29251,27.3516129032258) ;
#10701 = CIRCLE('',#29253,28.1741935483871) ;
#10702 = CIRCLE('',#29258,28.7741935483871) ;
#10703 = CIRCLE('',#29263,27.9516129032258) ;
#10704 = CIRCLE('',#29265,27.3516129032258) ;
#10705 = CIRCLE('',#29267,28.1741935483871) ;
#10706 = CIRCLE('',#29272,28.7741935483871) ;
#10707 = CIRCLE('',#29277,27.9516129032258) ;
#10708 = CIRCLE('',#29279,27.3516129032258) ;
#10709 = CIRCLE('',#29281,28.1741935483871) ;
#10710 = CIRCLE('',#29286,28.7741935483871) ;
#10711 = CIRCLE('',#29291,27.9516129032258) ;
#10712 = CIRCLE('',#29293,27.3516129032258) ;
#10713 = CIRCLE('',#29295,28.1741935483871) ;
#10714 = CIRCLE('',#29300,53.4) ;
#10715 = CIRCLE('',#29301,53.4) ;
#10716 = CIRCLE('',#29303,53.4) ;
#10717 = CIRCLE('',#29304,53.4) ;
#10718 = CIRCLE('',#29308,10.9) ;
#10719 = CIRCLE('',#29310,11.5) ;
#10720 = CIRCLE('',#29322,55.05) ;
#10721 = CIRCLE('',#29323,55.05) ;
#10722 = CIRCLE('',#29325,55.5) ;
#10723 = CIRCLE('',#29327,55.5) ;
#10724 = CIRCLE('',#29335,0.6) ;
#10725 = CIRCLE('',#29337,0.6) ;
#10726 = CIRCLE('',#29355,51.5) ;
#10727 = CIRCLE('',#29356,51.5) ;
#10728 = CIRCLE('',#29358,51.5) ;
#10729 = CIRCLE('',#29359,51.5) ;
#10730 = CIRCLE('',#29361,50.5) ;
#10731 = CIRCLE('',#29362,50.5) ;
#10732 = CIRCLE('',#29372,51.5) ;
#10733 = CIRCLE('',#29373,51.5) ;
#10734 = CIRCLE('',#29374,51.5) ;
#10735 = CIRCLE('',#29375,51.5) ;
#10736 = CIRCLE('',#29376,51.5) ;
#10737 = CIRCLE('',#29377,51.5) ;
#10738 = CIRCLE('',#29378,51.5) ;
#10739 = CIRCLE('',#29379,51.5) ;
#10740 = CIRCLE('',#29380,51.5) ;
#10741 = CIRCLE('',#29381,51.5) ;
#10742 = CIRCLE('',#29382,51.5) ;
#10743 = CIRCLE('',#29383,51.5) ;
#10744 = CIRCLE('',#29384,51.5) ;
#10745 = CIRCLE('',#29385,51.5) ;
#10746 = CIRCLE('',#29386,51.5) ;
#10747 = CIRCLE('',#29387,51.5) ;
#10748 = CIRCLE('',#29388,51.5) ;
#10749 = CIRCLE('',#29389,51.5) ;
#10750 = CIRCLE('',#29390,51.5) ;
#10751 = CIRCLE('',#29391,51.5) ;
#10752 = CIRCLE('',#29392,51.5) ;
#10753 = CIRCLE('',#29393,51.5) ;
#10754 = CIRCLE('',#29394,51.5) ;
#10755 = CIRCLE('',#29395,51.5) ;
#10756 = CIRCLE('',#29396,51.5) ;
#10757 = CIRCLE('',#29397,51.5) ;
#10758 = CIRCLE('',#29398,50.5) ;
#10759 = CIRCLE('',#29399,50.5) ;
#10760 = CIRCLE('',#29400,50.5) ;
#10761 = CIRCLE('',#29401,50.5) ;
#10762 = CIRCLE('',#29402,50.5) ;
#10763 = CIRCLE('',#29403,50.5) ;
#10764 = CIRCLE('',#29404,50.5) ;
#10765 = CIRCLE('',#29405,50.5) ;
#10766 = CIRCLE('',#29406,50.5) ;
#10767 = CIRCLE('',#29407,50.5) ;
#10768 = CIRCLE('',#29408,50.5) ;
#10769 = CIRCLE('',#29409,50.5) ;
#10770 = CIRCLE('',#29410,50.5) ;
#10771 = CIRCLE('',#29411,50.5) ;
#10772 = CIRCLE('',#29412,50.5) ;
#10773 = CIRCLE('',#29413,50.5) ;
#10774 = CIRCLE('',#29414,50.5) ;
#10775 = CIRCLE('',#29415,50.5) ;
#10776 = CIRCLE('',#29416,50.5) ;
#10777 = CIRCLE('',#29418,50.5) ;
#10778 = CIRCLE('',#29420,51.5) ;
#10779 = CIRCLE('',#29421,51.5) ;
#10780 = CIRCLE('',#29422,51.5) ;
#10781 = CIRCLE('',#29423,51.5) ;
#10782 = CIRCLE('',#29424,51.5) ;
#10783 = CIRCLE('',#29425,51.5) ;
#10784 = CIRCLE('',#29426,51.5) ;
#10785 = CIRCLE('',#29427,51.5) ;
#10786 = CIRCLE('',#29428,51.5) ;
#10787 = CIRCLE('',#29429,51.5) ;
#10788 = CIRCLE('',#29430,51.5) ;
#10789 = CIRCLE('',#29431,51.5) ;
#10790 = CIRCLE('',#29432,51.5) ;
#10791 = CIRCLE('',#29433,51.5) ;
#10792 = CIRCLE('',#29434,51.5) ;
#10793 = CIRCLE('',#29435,51.5) ;
#10794 = CIRCLE('',#29436,51.5) ;
#10795 = CIRCLE('',#29437,51.5) ;
#10796 = CIRCLE('',#29438,51.5) ;
#10797 = CIRCLE('',#29439,51.5) ;
#10798 = CIRCLE('',#29440,51.5) ;
#10799 = CIRCLE('',#29441,51.5) ;
#10800 = CIRCLE('',#29442,51.5) ;
#10801 = CIRCLE('',#29443,51.5) ;
#10802 = CIRCLE('',#29444,51.5) ;
#10803 = CIRCLE('',#29445,51.5) ;
#10804 = CIRCLE('',#29446,50.5) ;
#10805 = CIRCLE('',#29447,50.5) ;
#10806 = CIRCLE('',#29448,50.5) ;
#10807 = CIRCLE('',#29449,50.5) ;
#10808 = CIRCLE('',#29450,50.5) ;
#10809 = CIRCLE('',#29451,50.5) ;
#10810 = CIRCLE('',#29452,50.5) ;
#10811 = CIRCLE('',#29453,50.5) ;
#10812 = CIRCLE('',#29454,50.5) ;
#10813 = CIRCLE('',#29455,50.5) ;
#10814 = CIRCLE('',#29456,50.5) ;
#10815 = CIRCLE('',#29457,50.5) ;
#10816 = CIRCLE('',#29458,50.5) ;
#10817 = CIRCLE('',#29459,50.5) ;
#10818 = CIRCLE('',#29460,50.5) ;
#10819 = CIRCLE('',#29461,50.5) ;
#10820 = CIRCLE('',#29462,50.5) ;
#10821 = CIRCLE('',#29463,50.5) ;
#10822 = CIRCLE('',#29732,2.) ;
#10823 = CIRCLE('',#29733,2.) ;
#10824 = CIRCLE('',#29735,2.) ;
#10825 = CIRCLE('',#29736,2.) ;
#10826 = CIRCLE('',#29738,2.) ;
#10827 = CIRCLE('',#29739,2.) ;
#10828 = CIRCLE('',#29741,2.) ;
#10829 = CIRCLE('',#29742,2.) ;
#10830 = CIRCLE('',#29744,2.) ;
#10831 = CIRCLE('',#29745,2.) ;
#10832 = CIRCLE('',#29747,2.) ;
#10833 = CIRCLE('',#29748,2.) ;
#10834 = CIRCLE('',#29750,2.) ;
#10835 = CIRCLE('',#29751,2.) ;
#10836 = CIRCLE('',#29753,2.) ;
#10837 = CIRCLE('',#29754,2.) ;
#10838 = CIRCLE('',#29755,2.) ;
#10839 = CIRCLE('',#29757,2.) ;
#10840 = CIRCLE('',#29758,2.) ;
#10841 = CIRCLE('',#29759,2.) ;
#10842 = CIRCLE('',#29760,2.) ;
#10843 = CIRCLE('',#29762,2.) ;
#10844 = CIRCLE('',#29763,2.) ;
#10845 = CIRCLE('',#29764,2.) ;
#10846 = CIRCLE('',#29765,2.) ;
#10847 = CIRCLE('',#29767,2.) ;
#10848 = CIRCLE('',#29768,2.) ;
#10849 = CIRCLE('',#29769,2.) ;
#10850 = CIRCLE('',#29770,2.) ;
#10851 = CIRCLE('',#29772,2.) ;
#10852 = CIRCLE('',#29773,2.) ;
#10853 = CIRCLE('',#29774,2.) ;
#10854 = CIRCLE('',#29775,2.) ;
#10855 = CIRCLE('',#29777,2.) ;
#10856 = CIRCLE('',#29778,2.) ;
#10857 = CIRCLE('',#29779,2.) ;
#10858 = CIRCLE('',#29780,2.) ;
#10859 = CIRCLE('',#29782,2.) ;
#10860 = CIRCLE('',#29783,2.) ;
#10861 = CIRCLE('',#29784,2.) ;
#10862 = CIRCLE('',#29785,2.) ;
#10863 = CIRCLE('',#29787,2.) ;
#10864 = CIRCLE('',#29788,2.) ;
#10865 = CIRCLE('',#29789,2.) ;
#10866 = CIRCLE('',#29790,2.) ;
#10867 = CIRCLE('',#29792,2.) ;
#10868 = CIRCLE('',#29793,2.) ;
#10869 = CIRCLE('',#29794,2.) ;
#10870 = CIRCLE('',#29795,2.) ;
#10871 = CIRCLE('',#29797,2.) ;
#10872 = CIRCLE('',#29798,2.) ;
#10873 = CIRCLE('',#29799,2.) ;
#10874 = CIRCLE('',#29800,2.) ;
#10875 = CIRCLE('',#29802,2.) ;
#10876 = CIRCLE('',#29803,2.) ;
#10877 = CIRCLE('',#29804,2.) ;
#10878 = CIRCLE('',#29805,2.) ;
#10879 = CIRCLE('',#29807,2.) ;
#10880 = CIRCLE('',#29808,2.) ;
#10881 = CIRCLE('',#29809,2.) ;
#10882 = CIRCLE('',#29810,2.) ;
#10883 = CIRCLE('',#29812,2.) ;
#10884 = CIRCLE('',#29813,2.) ;
#10885 = CIRCLE('',#29814,2.) ;
#10886 = CIRCLE('',#29815,2.) ;
#10887 = CIRCLE('',#29817,2.) ;
#10888 = CIRCLE('',#29818,2.) ;
#10889 = CIRCLE('',#29819,2.) ;
#10890 = CIRCLE('',#29820,2.) ;
#10891 = CIRCLE('',#29822,2.) ;
#10892 = CIRCLE('',#29823,2.) ;
#10893 = CIRCLE('',#29824,2.) ;
#10894 = CIRCLE('',#29826,2.) ;
#10895 = CIRCLE('',#29827,2.) ;
#10896 = CIRCLE('',#29829,2.) ;
#10897 = CIRCLE('',#29830,2.) ;
#10898 = CIRCLE('',#29832,2.) ;
#10899 = CIRCLE('',#29833,2.) ;
#10900 = CIRCLE('',#29835,2.) ;
#10901 = CIRCLE('',#29836,2.) ;
#10902 = CIRCLE('',#29838,2.) ;
#10903 = CIRCLE('',#29839,2.) ;
#10904 = CIRCLE('',#29841,2.) ;
#10905 = CIRCLE('',#29842,2.) ;
#10906 = CIRCLE('',#29923,0.65) ;
#10907 = CIRCLE('',#29924,0.65) ;
#10908 = CIRCLE('',#29926,0.65) ;
#10909 = CIRCLE('',#29927,0.65) ;
#10910 = CIRCLE('',#29929,0.65) ;
#10911 = CIRCLE('',#29930,0.65) ;
#10912 = CIRCLE('',#29932,0.65) ;
#10913 = CIRCLE('',#29933,0.65) ;
#10914 = CIRCLE('',#29935,0.65) ;
#10915 = CIRCLE('',#29936,0.65) ;
#10916 = CIRCLE('',#29938,0.65) ;
#10917 = CIRCLE('',#29939,0.65) ;
#10918 = CIRCLE('',#29941,3.) ;
#10919 = CIRCLE('',#29942,3.) ;
#10920 = CIRCLE('',#29951,0.65) ;
#10921 = CIRCLE('',#29952,0.65) ;
#10922 = CIRCLE('',#29954,0.65) ;
#10923 = CIRCLE('',#29955,0.65) ;
#10924 = CIRCLE('',#29957,3.) ;
#10925 = CIRCLE('',#29958,3.) ;
#10926 = CIRCLE('',#29967,1.28) ;
#10927 = CIRCLE('',#29968,1.28) ;
#10928 = CIRCLE('',#29970,1.28) ;
#10929 = CIRCLE('',#29971,1.28) ;
#10930 = CIRCLE('',#29973,1.2) ;
#10931 = CIRCLE('',#29974,1.2) ;
#10932 = CIRCLE('',#29976,1.5) ;
#10933 = CIRCLE('',#29977,1.5) ;
#10934 = CIRCLE('',#29980,1.5) ;
#10935 = CIRCLE('',#29982,1.2) ;
#10936 = CIRCLE('',#29983,1.2) ;
#10937 = CIRCLE('',#29985,1.5) ;
#10938 = CIRCLE('',#29999,1.2) ;
#10939 = CIRCLE('',#30002,3.) ;
#10940 = CIRCLE('',#30006,3.) ;
#10941 = CIRCLE('',#30008,3.) ;
#10942 = CIRCLE('',#30015,3.) ;
#10943 = CIRCLE('',#30017,3.) ;
#10944 = CIRCLE('',#30020,3.) ;
#10945 = CIRCLE('',#30030,2.6) ;
#10946 = CIRCLE('',#30032,2.6) ;
#10947 = CIRCLE('',#30037,3.) ;
#10948 = CIRCLE('',#30043,3.) ;
#10949 = CIRCLE('',#30044,2.6) ;
#10950 = CIRCLE('',#30046,3.) ;
#10951 = CIRCLE('',#30047,2.6) ;
#10952 = CIRCLE('',#30070,1.2) ;
#10953 = CIRCLE('',#30072,1.5) ;
#10954 = CIRCLE('',#30073,1.2) ;
#10955 = CIRCLE('',#30075,1.5) ;
#10956 = CIRCLE('',#30078,1.5) ;
#10957 = CIRCLE('',#30080,1.5) ;
#10958 = CIRCLE('',#30081,1.2) ;
#10959 = CIRCLE('',#30085,3.) ;
#10960 = CIRCLE('',#30086,3.) ;
#10961 = CIRCLE('',#30087,3.) ;
#10962 = CIRCLE('',#30107,3.) ;
#10963 = CIRCLE('',#30108,3.) ;
#10964 = CIRCLE('',#30116,3.) ;
#10965 = CIRCLE('',#30119,3.) ;
#10966 = CIRCLE('',#30123,2.6) ;
#10967 = CIRCLE('',#30125,2.6) ;
#10968 = CIRCLE('',#30131,3.) ;
#10969 = CIRCLE('',#30133,3.) ;
#10970 = CIRCLE('',#30136,3.) ;
#10971 = CIRCLE('',#30139,3.) ;
#10972 = CIRCLE('',#30145,3.) ;
#10973 = CIRCLE('',#30147,3.) ;
#10974 = CIRCLE('',#30150,3.) ;
#10975 = CIRCLE('',#30152,3.) ;
#10976 = CIRCLE('',#30158,3.) ;
#10977 = CIRCLE('',#30159,3.) ;
#10978 = CIRCLE('',#30164,3.) ;
#10979 = CIRCLE('',#30166,3.) ;
#10980 = CIRCLE('',#30172,2.6) ;
#10981 = CIRCLE('',#30174,2.6) ;
#10982 = CIRCLE('',#30177,2.6) ;
#10983 = CIRCLE('',#30178,2.6) ;
#10984 = CIRCLE('',#30184,2.6) ;
#10985 = CIRCLE('',#30186,2.6) ;
#10986 = CIRCLE('',#30189,2.6) ;
#10987 = CIRCLE('',#30190,2.6) ;
#10988 = CIRCLE('',#30196,2.6) ;
#10989 = CIRCLE('',#30198,2.6) ;
#10990 = CIRCLE('',#30227,2.6) ;
#10991 = CIRCLE('',#30228,2.6) ;
#10992 = CIRCLE('',#30233,2.6) ;
#10993 = CIRCLE('',#30236,2.6) ;
#10994 = CIRCLE('',#30237,2.6) ;
#10995 = CIRCLE('',#30238,2.6) ;
#10996 = CIRCLE('',#30239,2.6) ;
#10997 = CIRCLE('',#30240,2.6) ;
#10998 = CIRCLE('',#30256,2.25) ;
#10999 = CIRCLE('',#30257,1.4) ;
#11000 = CIRCLE('',#30259,2.25) ;
#11001 = CIRCLE('',#30262,1.4) ;
#11002 = CIRCLE('',#30267,2.) ;
#11003 = CIRCLE('',#30268,1.25) ;
#11004 = CIRCLE('',#30270,2.) ;
#11005 = CIRCLE('',#30273,1.25) ;
#11006 = CIRCLE('',#30286,0.65) ;
#11007 = CIRCLE('',#30287,0.65) ;
#11008 = CIRCLE('',#30289,0.65) ;
#11009 = CIRCLE('',#30290,0.65) ;
#11010 = CIRCLE('',#30292,0.65) ;
#11011 = CIRCLE('',#30293,0.65) ;
#11012 = CIRCLE('',#30295,0.65) ;
#11013 = CIRCLE('',#30296,0.65) ;
#11014 = CIRCLE('',#30298,0.425) ;
#11015 = CIRCLE('',#30299,0.425) ;
#11016 = CIRCLE('',#30302,2.5) ;
#11017 = CIRCLE('',#30303,2.5) ;
#11018 = CIRCLE('',#30304,7.) ;
#11019 = CIRCLE('',#30305,7.) ;
#11020 = CIRCLE('',#30306,2.5) ;
#11021 = CIRCLE('',#30307,0.425) ;
#11022 = CIRCLE('',#30308,0.425) ;
#11023 = CIRCLE('',#30309,0.425) ;
#11024 = CIRCLE('',#30311,0.425) ;
#11025 = CIRCLE('',#30314,3.5) ;
#11026 = CIRCLE('',#30316,0.425) ;
#11027 = CIRCLE('',#30319,1.) ;
#11028 = CIRCLE('',#30321,0.425) ;
#11029 = CIRCLE('',#30324,0.5) ;
#11030 = CIRCLE('',#30325,0.5) ;
#11031 = CIRCLE('',#30328,1.) ;
#11032 = CIRCLE('',#30331,1.02) ;
#11033 = CIRCLE('',#30332,1.02) ;
#11034 = CIRCLE('',#30334,1.02) ;
#11035 = CIRCLE('',#30335,1.02) ;
#11036 = CIRCLE('',#30349,2.5) ;
#11037 = CIRCLE('',#30350,7.) ;
#11038 = CIRCLE('',#30352,7.) ;
#11039 = CIRCLE('',#30354,2.5) ;
#11040 = CIRCLE('',#30356,1.02) ;
#11041 = CIRCLE('',#30357,1.02) ;
#11042 = CIRCLE('',#30361,1.51) ;
#11043 = CIRCLE('',#30362,1.51) ;
#11044 = CIRCLE('',#30365,3.) ;
#11045 = CIRCLE('',#30366,3.) ;
#11046 = CIRCLE('',#30369,1.77) ;
#11047 = CIRCLE('',#30370,1.77) ;
#11048 = CIRCLE('',#30373,3.5) ;
#11049 = CIRCLE('',#30396,0.49) ;
#11050 = CIRCLE('',#30397,0.49) ;
#11051 = CIRCLE('',#30409,1.75) ;
#11052 = CIRCLE('',#30410,1.55) ;
#11053 = CIRCLE('',#30412,1.55) ;
#11054 = CIRCLE('',#30413,1.75) ;
#11055 = CIRCLE('',#30415,1.55) ;
#11056 = CIRCLE('',#30416,1.75) ;
#11057 = CIRCLE('',#30418,1.55) ;
#11058 = CIRCLE('',#30419,1.75) ;
#11059 = CIRCLE('',#30421,1.55) ;
#11060 = CIRCLE('',#30422,1.75) ;
#11061 = CIRCLE('',#30424,1.55) ;
#11062 = CIRCLE('',#30425,1.75) ;
#11063 = CIRCLE('',#30427,1.55) ;
#11064 = CIRCLE('',#30429,1.55) ;
#11065 = CIRCLE('',#30431,1.55) ;
#11066 = CIRCLE('',#30433,1.55) ;
#11067 = CIRCLE('',#30435,1.55) ;
#11068 = CIRCLE('',#30437,1.55) ;
#11069 = CIRCLE('',#30439,1.75) ;
#11070 = CIRCLE('',#30441,1.75) ;
#11071 = CIRCLE('',#30442,1.75) ;
#11072 = CIRCLE('',#30444,1.75) ;
#11073 = CIRCLE('',#30446,1.75) ;
#11074 = CIRCLE('',#30448,1.75) ;
#11075 = CIRCLE('',#30450,1.75) ;
#11076 = CIRCLE('',#30464,1.75) ;
#11077 = CIRCLE('',#30466,1.75) ;
#11078 = CIRCLE('',#30468,1.75) ;
#11079 = CIRCLE('',#30470,1.75) ;
#11080 = CIRCLE('',#30472,1.75) ;
#11081 = CIRCLE('',#30474,1.75) ;
#11082 = CIRCLE('',#30476,1.75) ;
#11083 = CIRCLE('',#30482,1.75) ;
#11084 = CIRCLE('',#30484,1.75) ;
#11085 = CIRCLE('',#30487,1.75) ;
#11086 = CIRCLE('',#30488,1.75) ;
#11087 = CIRCLE('',#30489,1.75) ;
#11088 = CIRCLE('',#30490,1.75) ;
#11089 = CIRCLE('',#30501,1.75) ;
#11090 = CIRCLE('',#30502,1.75) ;
#11091 = CIRCLE('',#30505,2.2) ;
#11092 = CIRCLE('',#30507,2.2) ;
#11093 = CIRCLE('',#30511,1.75) ;
#11094 = CIRCLE('',#30512,1.75) ;
#11095 = CIRCLE('',#30514,2.5) ;
#11096 = CIRCLE('',#30515,2.5) ;
#11097 = CIRCLE('',#30520,4.6) ;
#11098 = CIRCLE('',#30521,4.2) ;
#11099 = CIRCLE('',#30526,4.6) ;
#11100 = CIRCLE('',#30527,4.6) ;
#11101 = CIRCLE('',#30528,4.6) ;
#11102 = CIRCLE('',#30530,4.2) ;
#11103 = CIRCLE('',#30541,1.5) ;
#11104 = CIRCLE('',#30542,1.5) ;
#11105 = CIRCLE('',#30547,0.8) ;
#11106 = CIRCLE('',#30548,0.8) ;
#11107 = CIRCLE('',#30551,1.5) ;
#11108 = CIRCLE('',#30552,1.5) ;
#11109 = CIRCLE('',#30554,4.5) ;
#11110 = CIRCLE('',#30555,4.5) ;
#11111 = CIRCLE('',#30560,0.61) ;
#11112 = CIRCLE('',#30561,0.61) ;
#11113 = CIRCLE('',#30563,1.1) ;
#11114 = CIRCLE('',#30564,1.1) ;
#11115 = CIRCLE('',#30568,0.81) ;
#11116 = CIRCLE('',#30569,0.81) ;
#11117 = CIRCLE('',#30571,1.4) ;
#11118 = CIRCLE('',#30572,1.4) ;
#11119 = CIRCLE('',#30576,0.6) ;
#11120 = CIRCLE('',#30577,0.6) ;
#11121 = CIRCLE('',#30582,1.6) ;
#11122 = CIRCLE('',#30583,1.) ;
#11123 = CIRCLE('',#30585,1.6) ;
#11124 = CIRCLE('',#30586,1.) ;
#11125 = CIRCLE('',#30589,1.) ;
#11126 = CIRCLE('',#30590,1.) ;
#11127 = CIRCLE('',#30591,1.) ;
#11128 = CIRCLE('',#30592,1.) ;
#11129 = CIRCLE('',#30593,1.) ;
#11130 = CIRCLE('',#30594,1.) ;
#11131 = CIRCLE('',#30595,1.) ;
#11132 = CIRCLE('',#30596,1.) ;
#11133 = CIRCLE('',#30597,1.) ;
#11134 = CIRCLE('',#30598,1.) ;
#11135 = CIRCLE('',#30599,1.) ;
#11136 = CIRCLE('',#30600,1.) ;
#11137 = CIRCLE('',#30601,1.) ;
#11138 = CIRCLE('',#30602,1.) ;
#11139 = CIRCLE('',#30603,1.) ;
#11140 = CIRCLE('',#30604,1.) ;
#11141 = CIRCLE('',#30605,1.) ;
#11142 = CIRCLE('',#30606,1.) ;
#11143 = CIRCLE('',#30607,1.) ;
#11144 = CIRCLE('',#30608,1.) ;
#11145 = CIRCLE('',#30609,1.) ;
#11146 = CIRCLE('',#30651,1.) ;
#11147 = CIRCLE('',#30656,1.) ;
#11148 = CIRCLE('',#30657,1.) ;
#11149 = CIRCLE('',#30659,1.6) ;
#11150 = CIRCLE('',#30660,1.6) ;
#11151 = CIRCLE('',#30676,0.26) ;
#11152 = CIRCLE('',#30677,0.26) ;
#11153 = CIRCLE('',#30686,0.41) ;
#11154 = CIRCLE('',#30687,0.41) ;
#11155 = CIRCLE('',#30694,0.425) ;
#11156 = CIRCLE('',#30695,0.425) ;
#11157 = CIRCLE('',#30697,0.425) ;
#11158 = CIRCLE('',#30698,0.425) ;
#11159 = CIRCLE('',#30700,0.425) ;
#11160 = CIRCLE('',#30701,0.425) ;
#11161 = CIRCLE('',#30703,0.425) ;
#11162 = CIRCLE('',#30704,0.425) ;
#11163 = CIRCLE('',#30706,1.05) ;
#11164 = CIRCLE('',#30707,1.05) ;
#11165 = CIRCLE('',#30708,1.05) ;
#11166 = CIRCLE('',#30709,1.05) ;
#11167 = CIRCLE('',#30711,2.55) ;
#11168 = CIRCLE('',#30712,6.5) ;
#11169 = CIRCLE('',#30713,2.55) ;
#11170 = CIRCLE('',#30716,2.55) ;
#11171 = CIRCLE('',#30726,2.55) ;
#11172 = CIRCLE('',#30728,6.5) ;
#11173 = CIRCLE('',#30743,0.25) ;
#11174 = CIRCLE('',#30744,0.25) ;
#11175 = CIRCLE('',#30751,0.3) ;
#11176 = CIRCLE('',#30752,0.3) ;
#11177 = CIRCLE('',#30759,4.5) ;
#11178 = CIRCLE('',#30760,4.5) ;
#11179 = CIRCLE('',#30810,0.425) ;
#11180 = CIRCLE('',#30811,0.425) ;
#11181 = CIRCLE('',#30813,0.425) ;
#11182 = CIRCLE('',#30814,0.425) ;
#11183 = CIRCLE('',#30816,0.425) ;
#11184 = CIRCLE('',#30817,0.425) ;
#11185 = CIRCLE('',#30819,0.425) ;
#11186 = CIRCLE('',#30820,0.425) ;
#11187 = CIRCLE('',#30822,2.55) ;
#11188 = CIRCLE('',#30823,2.55) ;
#11189 = CIRCLE('',#30825,6.2) ;
#11190 = CIRCLE('',#30827,6.2) ;
#11191 = CIRCLE('',#30828,6.2) ;
#11192 = CIRCLE('',#30830,11.5) ;
#11193 = CIRCLE('',#30831,6.5) ;
#11194 = CIRCLE('',#30832,6.5) ;
#11195 = CIRCLE('',#30839,11.2) ;
#11196 = CIRCLE('',#30843,6.3) ;
#11197 = CIRCLE('',#30844,6.3) ;
#11198 = CIRCLE('',#30846,6.3) ;
#11199 = CIRCLE('',#30848,6.8) ;
#11200 = CIRCLE('',#30849,6.8) ;
#11201 = CIRCLE('',#30853,3.) ;
#11202 = CIRCLE('',#30854,2.8) ;
#11203 = CIRCLE('',#30856,6.3) ;
#11204 = CIRCLE('',#30857,6.1) ;
#11205 = CIRCLE('',#30862,0.4) ;
#11206 = CIRCLE('',#30863,0.4) ;
#11207 = CIRCLE('',#30865,0.4) ;
#11208 = CIRCLE('',#30866,0.4) ;
#11209 = CIRCLE('',#30868,0.4) ;
#11210 = CIRCLE('',#30869,0.4) ;
#11211 = CIRCLE('',#30871,0.4) ;
#11212 = CIRCLE('',#30872,0.4) ;
#11213 = CIRCLE('',#30874,0.4) ;
#11214 = CIRCLE('',#30875,0.4) ;
#11215 = CIRCLE('',#30877,0.4) ;
#11216 = CIRCLE('',#30878,0.4) ;
#11217 = CIRCLE('',#30880,0.4) ;
#11218 = CIRCLE('',#30881,0.4) ;
#11219 = CIRCLE('',#30883,0.51) ;
#11220 = CIRCLE('',#30884,0.51) ;
#11221 = CIRCLE('',#30887,8.) ;
#11222 = CIRCLE('',#30889,8.) ;
#11223 = CIRCLE('',#30893,0.4) ;
#11224 = CIRCLE('',#30894,0.4) ;
#11225 = CIRCLE('',#30895,0.4) ;
#11226 = CIRCLE('',#30900,0.31) ;
#11227 = CIRCLE('',#30901,0.31) ;
#11228 = CIRCLE('',#30903,0.15) ;
#11229 = CIRCLE('',#30906,0.15) ;
#11230 = CIRCLE('',#30908,0.51) ;
#11231 = CIRCLE('',#30909,0.51) ;
#11232 = CIRCLE('',#30927,0.700000000000003) ;
#11233 = CIRCLE('',#30928,0.7) ;
#11234 = CIRCLE('',#30931,1.6) ;
#11235 = CIRCLE('',#30934,0.8) ;
#11236 = CIRCLE('',#30935,0.5) ;
#11237 = CIRCLE('',#30937,0.8) ;
#11238 = CIRCLE('',#30940,0.5) ;
#11239 = CIRCLE('',#30944,0.149999999999999) ;
#11240 = CIRCLE('',#30946,0.149999999999999) ;
#11241 = CIRCLE('',#30948,0.149999999999999) ;
#11242 = CIRCLE('',#30950,0.15) ;
#11243 = CIRCLE('',#30952,0.15) ;
#11244 = CIRCLE('',#30955,0.4) ;
#11245 = CIRCLE('',#30956,0.4) ;
#11246 = CIRCLE('',#30958,0.4) ;
#11247 = CIRCLE('',#30959,0.4) ;
#11248 = CIRCLE('',#30960,0.4) ;
#11249 = CIRCLE('',#30961,0.4) ;
#11250 = CIRCLE('',#30963,0.4) ;
#11251 = CIRCLE('',#30964,0.150000000000006) ;
#11252 = CIRCLE('',#30966,0.4) ;
#11253 = CIRCLE('',#30967,0.4) ;
#11254 = CIRCLE('',#30968,0.4) ;
#11255 = CIRCLE('',#30970,0.15) ;
#11256 = CIRCLE('',#30972,0.149999999999999) ;
#11257 = CIRCLE('',#30973,0.15) ;
#11258 = CIRCLE('',#30975,0.4) ;
#11259 = CIRCLE('',#30977,0.4) ;
#11260 = CIRCLE('',#30981,0.4) ;
#11261 = CIRCLE('',#30984,0.4) ;
#11262 = CIRCLE('',#30988,0.4) ;
#11263 = CIRCLE('',#30991,0.4) ;
#11264 = CIRCLE('',#30996,0.4) ;
#11265 = CIRCLE('',#31002,0.149999999999999) ;
#11266 = CIRCLE('',#31004,0.149999999999999) ;
#11267 = CIRCLE('',#31005,0.4) ;
#11268 = CIRCLE('',#31006,0.149999999999999) ;
#11269 = CIRCLE('',#31010,0.149999999999999) ;
#11270 = CIRCLE('',#31012,0.4) ;
#11271 = CIRCLE('',#31013,0.149999999999999) ;
#11272 = CIRCLE('',#31014,0.149999999999999) ;
#11273 = CIRCLE('',#31017,0.4) ;
#11274 = CIRCLE('',#31019,0.149999999999999) ;
#11275 = CIRCLE('',#31020,0.149999999999999) ;
#11276 = CIRCLE('',#31023,0.149999999999999) ;
#11277 = CIRCLE('',#31024,0.4) ;
#11278 = CIRCLE('',#31025,0.149999999999999) ;
#11279 = CIRCLE('',#31026,0.399999999999999) ;
#11280 = CIRCLE('',#31028,0.4) ;
#11281 = CIRCLE('',#31030,0.149999999999999) ;
#11282 = CIRCLE('',#31031,0.149999999999999) ;
#11283 = CIRCLE('',#31035,0.149999999999999) ;
#11284 = CIRCLE('',#31040,0.125) ;
#11285 = CIRCLE('',#31043,0.125) ;
#11286 = CIRCLE('',#31047,0.125) ;
#11287 = CIRCLE('',#31048,0.125) ;
#11288 = CIRCLE('',#31050,0.125) ;
#11289 = CIRCLE('',#31053,0.125) ;
#11290 = CIRCLE('',#31054,0.125) ;
#11291 = CIRCLE('',#31059,0.29) ;
#11292 = CIRCLE('',#31060,0.29) ;
#11293 = CIRCLE('',#31065,0.29) ;
#11294 = CIRCLE('',#31066,0.29) ;
#11295 = CIRCLE('',#31071,0.55) ;
#11296 = CIRCLE('',#31072,0.55) ;
#11297 = CIRCLE('',#31074,0.25) ;
#11298 = CIRCLE('',#31075,0.25) ;
#11299 = CIRCLE('',#31079,0.15) ;
#11300 = CIRCLE('',#31082,0.8) ;
#11301 = CIRCLE('',#31083,0.8) ;
#11302 = CIRCLE('',#31085,1.1) ;
#11303 = CIRCLE('',#31086,1.1) ;
#11304 = CIRCLE('',#31091,0.8) ;
#11305 = CIRCLE('',#31092,0.8) ;
#11306 = CIRCLE('',#31094,1.1) ;
#11307 = CIRCLE('',#31095,1.1) ;
#11308 = CIRCLE('',#31098,0.0992156741649173) ;
#11309 = CIRCLE('',#31100,0.139053721633041) ;
#11310 = CIRCLE('',#31104,0.15) ;
#11311 = CIRCLE('',#31106,0.15) ;
#11312 = CIRCLE('',#31107,0.15) ;
#11313 = CIRCLE('',#31109,0.15) ;
#11314 = CIRCLE('',#31110,0.15) ;
#11315 = CIRCLE('',#31111,0.15) ;
#11316 = CIRCLE('',#31113,0.15) ;
#11317 = CIRCLE('',#31114,0.15) ;
#11318 = CIRCLE('',#31115,0.15) ;
#11319 = CIRCLE('',#31117,0.15) ;
#11320 = CIRCLE('',#31118,0.15) ;
#11321 = CIRCLE('',#31119,0.149999999999999) ;
#11322 = CIRCLE('',#31120,0.15) ;
#11323 = CIRCLE('',#31121,0.15) ;
#11324 = CIRCLE('',#31123,0.15) ;
#11325 = CIRCLE('',#31124,0.15) ;
#11326 = CIRCLE('',#31125,0.15) ;
#11327 = CIRCLE('',#31127,0.15) ;
#11328 = CIRCLE('',#31128,0.15) ;
#11329 = CIRCLE('',#31129,0.15) ;
#11330 = CIRCLE('',#31131,0.15) ;
#11331 = CIRCLE('',#31132,0.15) ;
#11332 = CIRCLE('',#31133,0.15) ;
#11333 = CIRCLE('',#31135,0.15) ;
#11334 = CIRCLE('',#31136,0.15) ;
#11335 = CIRCLE('',#31137,0.149999999999999) ;
#11336 = CIRCLE('',#31138,0.15) ;
#11337 = CIRCLE('',#31139,0.15) ;
#11338 = CIRCLE('',#31141,0.15) ;
#11339 = CIRCLE('',#31142,0.15) ;
#11340 = CIRCLE('',#31143,0.15) ;
#11341 = CIRCLE('',#31145,0.15) ;
#11342 = CIRCLE('',#31146,0.15) ;
#11343 = CIRCLE('',#31147,0.15) ;
#11344 = CIRCLE('',#31149,0.15) ;
#11345 = CIRCLE('',#31150,0.15) ;
#11346 = CIRCLE('',#31151,0.15) ;
#11347 = CIRCLE('',#31153,0.15) ;
#11348 = CIRCLE('',#31154,0.15) ;
#11349 = CIRCLE('',#31155,0.149999999999999) ;
#11350 = CIRCLE('',#31156,0.15) ;
#11351 = CIRCLE('',#31157,0.15) ;
#11352 = CIRCLE('',#31159,0.15) ;
#11353 = CIRCLE('',#31160,0.15) ;
#11354 = CIRCLE('',#31161,0.15) ;
#11355 = CIRCLE('',#31163,0.15) ;
#11356 = CIRCLE('',#31164,0.15) ;
#11357 = CIRCLE('',#31165,0.15) ;
#11358 = CIRCLE('',#31167,0.15) ;
#11359 = CIRCLE('',#31168,0.15) ;
#11360 = CIRCLE('',#31169,0.15) ;
#11361 = CIRCLE('',#31171,0.15) ;
#11362 = CIRCLE('',#31172,0.15) ;
#11363 = CIRCLE('',#31173,0.149999999999999) ;
#11364 = CIRCLE('',#31174,0.15) ;
#11365 = CIRCLE('',#31175,0.15) ;
#11366 = CIRCLE('',#31177,0.15) ;
#11367 = CIRCLE('',#31178,0.15) ;
#11368 = CIRCLE('',#31179,0.15) ;
#11369 = CIRCLE('',#31181,0.15) ;
#11370 = CIRCLE('',#31182,0.15) ;
#11371 = CIRCLE('',#31183,0.15) ;
#11372 = CIRCLE('',#31185,0.15) ;
#11373 = CIRCLE('',#31186,0.15) ;
#11374 = CIRCLE('',#31187,0.15) ;
#11375 = CIRCLE('',#31189,0.15) ;
#11376 = CIRCLE('',#31190,0.15) ;
#11377 = CIRCLE('',#31191,0.149999999999999) ;
#11378 = CIRCLE('',#31192,0.15) ;
#11379 = CIRCLE('',#31193,0.15) ;
#11380 = CIRCLE('',#31195,0.15) ;
#11381 = CIRCLE('',#31196,0.15) ;
#11382 = CIRCLE('',#31197,0.15) ;
#11383 = CIRCLE('',#31199,0.15) ;
#11384 = CIRCLE('',#31200,0.15) ;
#11385 = CIRCLE('',#31201,0.15) ;
#11386 = CIRCLE('',#31203,0.15) ;
#11387 = CIRCLE('',#31204,0.15) ;
#11388 = CIRCLE('',#31205,0.15) ;
#11389 = CIRCLE('',#31207,0.15) ;
#11390 = CIRCLE('',#31208,0.15) ;
#11391 = CIRCLE('',#31209,0.149999999999999) ;
#11392 = CIRCLE('',#31210,0.15) ;
#11393 = CIRCLE('',#31211,0.15) ;
#11394 = CIRCLE('',#31213,0.15) ;
#11395 = CIRCLE('',#31214,0.15) ;
#11396 = CIRCLE('',#31215,0.15) ;
#11397 = CIRCLE('',#31217,0.15) ;
#11398 = CIRCLE('',#31218,0.15) ;
#11399 = CIRCLE('',#31219,0.15) ;
#11400 = CIRCLE('',#31221,0.15) ;
#11401 = CIRCLE('',#31222,0.15) ;
#11402 = CIRCLE('',#31223,0.15) ;
#11403 = CIRCLE('',#31225,0.15) ;
#11404 = CIRCLE('',#31226,0.15) ;
#11405 = CIRCLE('',#31227,0.149999999999999) ;
#11406 = CIRCLE('',#31228,0.15) ;
#11407 = CIRCLE('',#31229,0.15) ;
#11408 = CIRCLE('',#31231,0.15) ;
#11409 = CIRCLE('',#31232,0.15) ;
#11410 = CIRCLE('',#31233,0.15) ;
#11411 = CIRCLE('',#31235,0.15) ;
#11412 = CIRCLE('',#31236,0.15) ;
#11413 = CIRCLE('',#31237,0.15) ;
#11414 = CIRCLE('',#31239,0.15) ;
#11415 = CIRCLE('',#31240,0.15) ;
#11416 = CIRCLE('',#31241,0.15) ;
#11417 = CIRCLE('',#31243,0.15) ;
#11418 = CIRCLE('',#31244,0.15) ;
#11419 = CIRCLE('',#31245,0.149999999999999) ;
#11420 = CIRCLE('',#31246,0.15) ;
#11421 = CIRCLE('',#31247,0.15) ;
#11422 = CIRCLE('',#31249,0.15) ;
#11423 = CIRCLE('',#31250,0.15) ;
#11424 = CIRCLE('',#31251,0.15) ;
#11425 = CIRCLE('',#31253,0.15) ;
#11426 = CIRCLE('',#31254,0.15) ;
#11427 = CIRCLE('',#31255,0.15) ;
#11428 = CIRCLE('',#31257,0.15) ;
#11429 = CIRCLE('',#31258,0.15) ;
#11430 = CIRCLE('',#31259,0.15) ;
#11431 = CIRCLE('',#31261,0.15) ;
#11432 = CIRCLE('',#31262,0.15) ;
#11433 = CIRCLE('',#31263,0.149999999999999) ;
#11434 = CIRCLE('',#31264,0.15) ;
#11435 = CIRCLE('',#31265,0.15) ;
#11436 = CIRCLE('',#31267,0.15) ;
#11437 = CIRCLE('',#31268,0.15) ;
#11438 = CIRCLE('',#31269,0.15) ;
#11439 = CIRCLE('',#31271,0.15) ;
#11440 = CIRCLE('',#31272,0.15) ;
#11441 = CIRCLE('',#31273,0.15) ;
#11442 = CIRCLE('',#31275,0.15) ;
#11443 = CIRCLE('',#31276,0.15) ;
#11444 = CIRCLE('',#31277,0.15) ;
#11445 = CIRCLE('',#31279,0.15) ;
#11446 = CIRCLE('',#31280,0.15) ;
#11447 = CIRCLE('',#31281,0.149999999999999) ;
#11448 = CIRCLE('',#31282,0.15) ;
#11449 = CIRCLE('',#31283,0.15) ;
#11450 = CIRCLE('',#31285,0.15) ;
#11451 = CIRCLE('',#31286,0.15) ;
#11452 = CIRCLE('',#31287,0.15) ;
#11453 = CIRCLE('',#31289,0.15) ;
#11454 = CIRCLE('',#31290,0.15) ;
#11455 = CIRCLE('',#31291,0.15) ;
#11456 = CIRCLE('',#31293,0.15) ;
#11457 = CIRCLE('',#31294,0.15) ;
#11458 = CIRCLE('',#31295,0.15) ;
#11459 = CIRCLE('',#31297,0.15) ;
#11460 = CIRCLE('',#31298,0.15) ;
#11461 = CIRCLE('',#31299,0.149999999999999) ;
#11462 = CIRCLE('',#31300,0.15) ;
#11463 = CIRCLE('',#31301,0.15) ;
#11464 = CIRCLE('',#31303,0.15) ;
#11465 = CIRCLE('',#31304,0.15) ;
#11466 = CIRCLE('',#31305,0.15) ;
#11467 = CIRCLE('',#31307,0.15) ;
#11468 = CIRCLE('',#31308,0.15) ;
#11469 = CIRCLE('',#31309,0.15) ;
#11470 = CIRCLE('',#31311,0.15) ;
#11471 = CIRCLE('',#31312,0.15) ;
#11472 = CIRCLE('',#31313,0.15) ;
#11473 = CIRCLE('',#31315,0.15) ;
#11474 = CIRCLE('',#31316,0.15) ;
#11475 = CIRCLE('',#31317,0.149999999999999) ;
#11476 = CIRCLE('',#31318,0.15) ;
#11477 = CIRCLE('',#31319,0.15) ;
#11478 = CIRCLE('',#31321,0.15) ;
#11479 = CIRCLE('',#31322,0.15) ;
#11480 = CIRCLE('',#31323,0.15) ;
#11481 = CIRCLE('',#31325,0.15) ;
#11482 = CIRCLE('',#31326,0.15) ;
#11483 = CIRCLE('',#31327,0.15) ;
#11484 = CIRCLE('',#31329,0.15) ;
#11485 = CIRCLE('',#31330,0.15) ;
#11486 = CIRCLE('',#31331,0.15) ;
#11487 = CIRCLE('',#31333,0.15) ;
#11488 = CIRCLE('',#31334,0.15) ;
#11489 = CIRCLE('',#31335,0.149999999999999) ;
#11490 = CIRCLE('',#31336,0.15) ;
#11491 = CIRCLE('',#31337,0.15) ;
#11492 = CIRCLE('',#31339,0.15) ;
#11493 = CIRCLE('',#31340,0.15) ;
#11494 = CIRCLE('',#31341,0.15) ;
#11495 = CIRCLE('',#31343,0.15) ;
#11496 = CIRCLE('',#31344,0.15) ;
#11497 = CIRCLE('',#31345,0.15) ;
#11498 = CIRCLE('',#31347,0.15) ;
#11499 = CIRCLE('',#31348,0.15) ;
#11500 = CIRCLE('',#31349,0.15) ;
#11501 = CIRCLE('',#31351,0.15) ;
#11502 = CIRCLE('',#31352,0.15) ;
#11503 = CIRCLE('',#31353,0.149999999999999) ;
#11504 = CIRCLE('',#31354,0.15) ;
#11505 = CIRCLE('',#31355,0.15) ;
#11506 = CIRCLE('',#31357,0.15) ;
#11507 = CIRCLE('',#31358,0.15) ;
#11508 = CIRCLE('',#31359,0.15) ;
#11509 = CIRCLE('',#31361,0.15) ;
#11510 = CIRCLE('',#31362,0.15) ;
#11511 = CIRCLE('',#31363,0.15) ;
#11512 = CIRCLE('',#31365,0.15) ;
#11513 = CIRCLE('',#31366,0.15) ;
#11514 = CIRCLE('',#31367,0.15) ;
#11515 = CIRCLE('',#31369,0.15) ;
#11516 = CIRCLE('',#31370,0.15) ;
#11517 = CIRCLE('',#31371,0.149999999999999) ;
#11518 = CIRCLE('',#31372,0.15) ;
#11519 = CIRCLE('',#31373,0.15) ;
#11520 = CIRCLE('',#31375,0.15) ;
#11521 = CIRCLE('',#31376,0.15) ;
#11522 = CIRCLE('',#31377,0.15) ;
#11523 = CIRCLE('',#31379,0.15) ;
#11524 = CIRCLE('',#31380,0.15) ;
#11525 = CIRCLE('',#31381,0.15) ;
#11526 = CIRCLE('',#31383,0.15) ;
#11527 = CIRCLE('',#31384,0.15) ;
#11528 = CIRCLE('',#31385,0.15) ;
#11529 = CIRCLE('',#31387,0.15) ;
#11530 = CIRCLE('',#31388,0.15) ;
#11531 = CIRCLE('',#31389,0.149999999999999) ;
#11532 = CIRCLE('',#31390,0.15) ;
#11533 = CIRCLE('',#31391,0.15) ;
#11534 = CIRCLE('',#31393,0.15) ;
#11535 = CIRCLE('',#31394,0.15) ;
#11536 = CIRCLE('',#31395,0.15) ;
#11537 = CIRCLE('',#31397,0.15) ;
#11538 = CIRCLE('',#31398,0.15) ;
#11539 = CIRCLE('',#31399,0.15) ;
#11540 = CIRCLE('',#31401,0.15) ;
#11541 = CIRCLE('',#31402,0.15) ;
#11542 = CIRCLE('',#31403,0.15) ;
#11543 = CIRCLE('',#31405,0.15) ;
#11544 = CIRCLE('',#31406,0.15) ;
#11545 = CIRCLE('',#31407,0.149999999999999) ;
#11546 = CIRCLE('',#31408,0.15) ;
#11547 = CIRCLE('',#31409,0.15) ;
#11548 = CIRCLE('',#31411,0.15) ;
#11549 = CIRCLE('',#31412,0.15) ;
#11550 = CIRCLE('',#31413,0.15) ;
#11551 = CIRCLE('',#31415,0.15) ;
#11552 = CIRCLE('',#31416,0.15) ;
#11553 = CIRCLE('',#31417,0.15) ;
#11554 = CIRCLE('',#31419,0.15) ;
#11555 = CIRCLE('',#31420,0.15) ;
#11556 = CIRCLE('',#31421,0.15) ;
#11557 = CIRCLE('',#31423,0.15) ;
#11558 = CIRCLE('',#31424,0.15) ;
#11559 = CIRCLE('',#31425,0.149999999999999) ;
#11560 = CIRCLE('',#31426,0.15) ;
#11561 = CIRCLE('',#31427,0.15) ;
#11562 = CIRCLE('',#31429,0.15) ;
#11563 = CIRCLE('',#31430,0.15) ;
#11564 = CIRCLE('',#31431,0.15) ;
#11565 = CIRCLE('',#31433,0.15) ;
#11566 = CIRCLE('',#31434,0.15) ;
#11567 = CIRCLE('',#31435,0.15) ;
#11568 = CIRCLE('',#31437,0.15) ;
#11569 = CIRCLE('',#31438,0.15) ;
#11570 = CIRCLE('',#31439,0.15) ;
#11571 = CIRCLE('',#31441,0.15) ;
#11572 = CIRCLE('',#31442,0.15) ;
#11573 = CIRCLE('',#31443,0.149999999999999) ;
#11574 = CIRCLE('',#31444,0.15) ;
#11575 = CIRCLE('',#31445,0.15) ;
#11576 = CIRCLE('',#31447,0.15) ;
#11577 = CIRCLE('',#31448,0.15) ;
#11578 = CIRCLE('',#31449,0.15) ;
#11579 = CIRCLE('',#31451,0.15) ;
#11580 = CIRCLE('',#31452,0.15) ;
#11581 = CIRCLE('',#31453,0.15) ;
#11582 = CIRCLE('',#31455,0.15) ;
#11583 = CIRCLE('',#31456,0.15) ;
#11584 = CIRCLE('',#31457,0.15) ;
#11585 = CIRCLE('',#31459,0.15) ;
#11586 = CIRCLE('',#31460,0.15) ;
#11587 = CIRCLE('',#31461,0.149999999999999) ;
#11588 = CIRCLE('',#31462,0.15) ;
#11589 = CIRCLE('',#31463,0.15) ;
#11590 = CIRCLE('',#31465,0.15) ;
#11591 = CIRCLE('',#31466,0.15) ;
#11592 = CIRCLE('',#31467,0.15) ;
#11593 = CIRCLE('',#31469,0.15) ;
#11594 = CIRCLE('',#31470,0.15) ;
#11595 = CIRCLE('',#31471,0.15) ;
#11596 = CIRCLE('',#31473,0.15) ;
#11597 = CIRCLE('',#31474,0.15) ;
#11598 = CIRCLE('',#31475,0.15) ;
#11599 = CIRCLE('',#31477,0.15) ;
#11600 = CIRCLE('',#31478,0.15) ;
#11601 = CIRCLE('',#31479,0.149999999999999) ;
#11602 = CIRCLE('',#31480,0.15) ;
#11603 = CIRCLE('',#31481,0.15) ;
#11604 = CIRCLE('',#31483,0.15) ;
#11605 = CIRCLE('',#31484,0.15) ;
#11606 = CIRCLE('',#31485,0.15) ;
#11607 = CIRCLE('',#31487,0.15) ;
#11608 = CIRCLE('',#31488,0.15) ;
#11609 = CIRCLE('',#31489,0.15) ;
#11610 = CIRCLE('',#31491,0.15) ;
#11611 = CIRCLE('',#31492,0.15) ;
#11612 = CIRCLE('',#31493,0.15) ;
#11613 = CIRCLE('',#31495,0.15) ;
#11614 = CIRCLE('',#31496,0.15) ;
#11615 = CIRCLE('',#31497,0.149999999999999) ;
#11616 = CIRCLE('',#31498,0.15) ;
#11617 = CIRCLE('',#31499,0.15) ;
#11618 = CIRCLE('',#31501,0.15) ;
#11619 = CIRCLE('',#31502,0.15) ;
#11620 = CIRCLE('',#31503,0.15) ;
#11621 = CIRCLE('',#31505,0.15) ;
#11622 = CIRCLE('',#31506,0.15) ;
#11623 = CIRCLE('',#31507,0.15) ;
#11624 = CIRCLE('',#31509,0.15) ;
#11625 = CIRCLE('',#31510,0.15) ;
#11626 = CIRCLE('',#31511,0.15) ;
#11627 = CIRCLE('',#31513,0.15) ;
#11628 = CIRCLE('',#31514,0.15) ;
#11629 = CIRCLE('',#31515,0.149999999999999) ;
#11630 = CIRCLE('',#31516,0.15) ;
#11631 = CIRCLE('',#31517,0.15) ;
#11632 = CIRCLE('',#31519,0.15) ;
#11633 = CIRCLE('',#31520,0.15) ;
#11634 = CIRCLE('',#31521,0.15) ;
#11635 = CIRCLE('',#31523,0.15) ;
#11636 = CIRCLE('',#31524,0.15) ;
#11637 = CIRCLE('',#31525,0.15) ;
#11638 = CIRCLE('',#31527,0.15) ;
#11639 = CIRCLE('',#31528,0.15) ;
#11640 = CIRCLE('',#31529,0.15) ;
#11641 = CIRCLE('',#31531,0.15) ;
#11642 = CIRCLE('',#31532,0.15) ;
#11643 = CIRCLE('',#31533,0.149999999999999) ;
#11644 = CIRCLE('',#31534,0.15) ;
#11645 = CIRCLE('',#31535,0.15) ;
#11646 = CIRCLE('',#31537,0.15) ;
#11647 = CIRCLE('',#31538,0.15) ;
#11648 = CIRCLE('',#31539,0.15) ;
#11649 = CIRCLE('',#31541,0.15) ;
#11650 = CIRCLE('',#31542,0.15) ;
#11651 = CIRCLE('',#31543,0.15) ;
#11652 = CIRCLE('',#31545,0.15) ;
#11653 = CIRCLE('',#31546,0.15) ;
#11654 = CIRCLE('',#31547,0.15) ;
#11655 = CIRCLE('',#31549,0.15) ;
#11656 = CIRCLE('',#31550,0.15) ;
#11657 = CIRCLE('',#31551,0.149999999999999) ;
#11658 = CIRCLE('',#31552,0.15) ;
#11659 = CIRCLE('',#31553,0.15) ;
#11660 = CIRCLE('',#31555,0.15) ;
#11661 = CIRCLE('',#31556,0.15) ;
#11662 = CIRCLE('',#31557,0.15) ;
#11663 = CIRCLE('',#31559,0.15) ;
#11664 = CIRCLE('',#31560,0.15) ;
#11665 = CIRCLE('',#31561,0.15) ;
#11666 = CIRCLE('',#31563,0.15) ;
#11667 = CIRCLE('',#31564,0.15) ;
#11668 = CIRCLE('',#31565,0.15) ;
#11669 = CIRCLE('',#31567,0.15) ;
#11670 = CIRCLE('',#31568,0.15) ;
#11671 = CIRCLE('',#31569,0.149999999999999) ;
#11672 = CIRCLE('',#31570,0.15) ;
#11673 = CIRCLE('',#31571,0.15) ;
#11674 = CIRCLE('',#31573,0.15) ;
#11675 = CIRCLE('',#31574,0.15) ;
#11676 = CIRCLE('',#31575,0.15) ;
#11677 = CIRCLE('',#31577,0.15) ;
#11678 = CIRCLE('',#31578,0.15) ;
#11679 = CIRCLE('',#31579,0.15) ;
#11680 = CIRCLE('',#31581,0.15) ;
#11681 = CIRCLE('',#31582,0.15) ;
#11682 = CIRCLE('',#31583,0.15) ;
#11683 = CIRCLE('',#31585,0.15) ;
#11684 = CIRCLE('',#31586,0.15) ;
#11685 = CIRCLE('',#31587,0.149999999999999) ;
#11686 = CIRCLE('',#31588,0.15) ;
#11687 = CIRCLE('',#31589,0.15) ;
#11688 = CIRCLE('',#31591,0.15) ;
#11689 = CIRCLE('',#31592,0.15) ;
#11690 = CIRCLE('',#31593,0.15) ;
#11691 = CIRCLE('',#31595,0.15) ;
#11692 = CIRCLE('',#31596,0.15) ;
#11693 = CIRCLE('',#31597,0.15) ;
#11694 = CIRCLE('',#31599,0.15) ;
#11695 = CIRCLE('',#31600,0.15) ;
#11696 = CIRCLE('',#31601,0.15) ;
#11697 = CIRCLE('',#31603,0.15) ;
#11698 = CIRCLE('',#31604,0.15) ;
#11699 = CIRCLE('',#31605,0.149999999999999) ;
#11700 = CIRCLE('',#31606,0.15) ;
#11701 = CIRCLE('',#31607,0.15) ;
#11702 = CIRCLE('',#31609,0.15) ;
#11703 = CIRCLE('',#31610,0.15) ;
#11704 = CIRCLE('',#31611,0.15) ;
#11705 = CIRCLE('',#31613,0.15) ;
#11706 = CIRCLE('',#31614,0.15) ;
#11707 = CIRCLE('',#31615,0.15) ;
#11708 = CIRCLE('',#31617,0.15) ;
#11709 = CIRCLE('',#31618,0.15) ;
#11710 = CIRCLE('',#31619,0.15) ;
#11711 = CIRCLE('',#31621,0.15) ;
#11712 = CIRCLE('',#31622,0.15) ;
#11713 = CIRCLE('',#31623,0.149999999999999) ;
#11714 = CIRCLE('',#31624,0.15) ;
#11715 = CIRCLE('',#31625,0.15) ;
#11716 = CIRCLE('',#31627,0.15) ;
#11717 = CIRCLE('',#31628,0.15) ;
#11718 = CIRCLE('',#31629,0.15) ;
#11719 = CIRCLE('',#31631,0.15) ;
#11720 = CIRCLE('',#31632,0.15) ;
#11721 = CIRCLE('',#31633,0.15) ;
#11722 = CIRCLE('',#31635,0.15) ;
#11723 = CIRCLE('',#31636,0.15) ;
#11724 = CIRCLE('',#31637,0.15) ;
#11725 = CIRCLE('',#31639,0.15) ;
#11726 = CIRCLE('',#31640,0.15) ;
#11727 = CIRCLE('',#31641,0.149999999999999) ;
#11728 = CIRCLE('',#31642,0.15) ;
#11729 = CIRCLE('',#31643,0.15) ;
#11730 = CIRCLE('',#31645,0.15) ;
#11731 = CIRCLE('',#31646,0.15) ;
#11732 = CIRCLE('',#31647,0.15) ;
#11733 = CIRCLE('',#31649,0.15) ;
#11734 = CIRCLE('',#31650,0.15) ;
#11735 = CIRCLE('',#31651,0.15) ;
#11736 = CIRCLE('',#31653,0.15) ;
#11737 = CIRCLE('',#31654,0.15) ;
#11738 = CIRCLE('',#31655,0.15) ;
#11739 = CIRCLE('',#31657,0.15) ;
#11740 = CIRCLE('',#31658,0.15) ;
#11741 = CIRCLE('',#31659,0.149999999999999) ;
#11742 = CIRCLE('',#31660,0.15) ;
#11743 = CIRCLE('',#31661,0.15) ;
#11744 = CIRCLE('',#31663,0.15) ;
#11745 = CIRCLE('',#31664,0.15) ;
#11746 = CIRCLE('',#31665,0.15) ;
#11747 = CIRCLE('',#31667,0.15) ;
#11748 = CIRCLE('',#31668,0.15) ;
#11749 = CIRCLE('',#31669,0.15) ;
#11750 = CIRCLE('',#31671,0.15) ;
#11751 = CIRCLE('',#31672,0.15) ;
#11752 = CIRCLE('',#31673,0.15) ;
#11753 = CIRCLE('',#32054,0.15) ;
#11754 = CIRCLE('',#32057,0.55) ;
#11755 = CIRCLE('',#32058,0.55) ;
#11756 = CIRCLE('',#32060,0.25) ;
#11757 = CIRCLE('',#32061,0.25) ;
#11758 = CIRCLE('',#32065,0.15) ;
#11759 = CIRCLE('',#32084,3.3) ;
#11760 = CIRCLE('',#32086,3.3) ;
#11761 = CIRCLE('',#32087,3.3) ;
#11762 = CIRCLE('',#32092,3.5) ;
#11763 = CIRCLE('',#32093,3.3) ;
#11764 = CIRCLE('',#32095,3.5) ;
#11765 = CIRCLE('',#32098,3.5) ;
#11766 = CIRCLE('',#32099,3.5) ;
#11767 = CIRCLE('',#32101,3.5) ;
#11768 = CIRCLE('',#32102,3.3) ;
#11769 = CIRCLE('',#32104,3.5) ;
#11770 = CIRCLE('',#32106,3.5) ;
#11771 = CIRCLE('',#32107,3.5) ;
#11772 = CIRCLE('',#32109,3.3) ;
#11773 = CIRCLE('',#32110,3.3) ;
#11774 = CIRCLE('',#32112,3.3) ;
#11775 = CIRCLE('',#32113,3.3) ;
#11776 = CIRCLE('',#32117,3.5) ;
#11777 = CIRCLE('',#32120,0.6) ;
#11778 = CIRCLE('',#32121,0.6) ;
#11779 = CIRCLE('',#32131,1.) ;
#11780 = CIRCLE('',#32133,1.) ;
#11781 = CIRCLE('',#32135,1.) ;
#11782 = CIRCLE('',#32140,1.) ;
#11783 = CIRCLE('',#32142,1.) ;
#11784 = CIRCLE('',#32143,1.) ;
#11785 = CIRCLE('',#32147,4.5) ;
#11786 = CIRCLE('',#32148,4.5) ;
#11787 = CIRCLE('',#32150,4.5) ;
#11788 = CIRCLE('',#32151,3.5) ;
#11789 = CIRCLE('',#32153,4.5) ;
#11790 = CIRCLE('',#32154,3.5) ;
#11791 = CIRCLE('',#32159,1.) ;
#11792 = CIRCLE('',#32160,1.) ;
#11793 = CIRCLE('',#32162,1.02) ;
#11794 = CIRCLE('',#32163,1.02) ;
#11795 = CIRCLE('',#32168,3.5) ;
#11796 = CIRCLE('',#32169,3.5) ;
#11797 = CIRCLE('',#32192,3.8) ;
#11798 = CIRCLE('',#32193,3.8) ;
#11799 = CIRCLE('',#32194,3.5) ;
#11800 = CIRCLE('',#32196,3.5) ;
#11801 = CIRCLE('',#32198,3.8) ;
#11802 = CIRCLE('',#32209,0.6) ;
#11803 = CIRCLE('',#32210,0.6) ;
#11804 = CIRCLE('',#32222,0.6) ;
#11805 = CIRCLE('',#32223,0.6) ;
#11806 = CIRCLE('',#32234,0.4) ;
#11807 = CIRCLE('',#32235,0.4) ;
#11808 = CIRCLE('',#32247,0.5) ;
#11809 = CIRCLE('',#32248,0.5) ;
#11810 = CIRCLE('',#32259,0.45) ;
#11811 = CIRCLE('',#32260,0.245) ;
#11812 = CIRCLE('',#32262,0.45) ;
#11813 = CIRCLE('',#32265,0.245) ;
#11814 = CIRCLE('',#32269,0.45) ;
#11815 = CIRCLE('',#32270,0.245) ;
#11816 = CIRCLE('',#32272,0.45) ;
#11817 = CIRCLE('',#32275,0.245) ;
#11818 = CIRCLE('',#32283,0.25) ;
#11819 = CIRCLE('',#32287,0.25) ;
#11820 = CIRCLE('',#32288,0.25) ;
#11821 = CIRCLE('',#32290,0.25) ;
#11822 = CIRCLE('',#32291,0.25) ;
#11823 = CIRCLE('',#32293,0.25) ;
#11824 = CIRCLE('',#32294,0.25) ;
#11825 = CIRCLE('',#32296,0.25) ;
#11826 = CIRCLE('',#32297,0.25) ;
#11827 = CIRCLE('',#32298,0.25) ;
#11828 = CIRCLE('',#32299,0.25) ;
#11829 = CIRCLE('',#32301,0.25) ;
#11830 = CIRCLE('',#32302,0.25) ;
#11831 = CIRCLE('',#32303,0.25) ;
#11832 = CIRCLE('',#32304,0.25) ;
#11833 = CIRCLE('',#32306,0.25) ;
#11834 = CIRCLE('',#32307,0.25) ;
#11835 = CIRCLE('',#32308,0.25) ;
#11836 = CIRCLE('',#32309,0.25) ;
#11837 = CIRCLE('',#32311,0.25) ;
#11838 = CIRCLE('',#32312,0.25) ;
#11839 = CIRCLE('',#32313,0.25) ;
#11840 = CIRCLE('',#32314,0.25) ;
#11841 = CIRCLE('',#32316,0.25) ;
#11842 = CIRCLE('',#32317,0.25) ;
#11843 = CIRCLE('',#32318,0.25) ;
#11844 = CIRCLE('',#32319,0.25) ;
#11845 = CIRCLE('',#32321,0.25) ;
#11846 = CIRCLE('',#32322,0.25) ;
#11847 = CIRCLE('',#32323,0.25) ;
#11848 = CIRCLE('',#32324,0.25) ;
#11849 = CIRCLE('',#32326,0.25) ;
#11850 = CIRCLE('',#32328,0.25) ;
#11851 = CIRCLE('',#32329,0.25) ;
#11852 = CIRCLE('',#32359,0.3) ;
#11853 = CIRCLE('',#32361,0.3) ;
#11854 = CIRCLE('',#32362,0.3) ;
#11855 = VERTEX_POINT('',#41227) ;
#11856 = VERTEX_POINT('',#41229) ;
#11857 = VERTEX_POINT('',#41233) ;
#11858 = VERTEX_POINT('',#41234) ;
#11859 = VERTEX_POINT('',#41236) ;
#11860 = VERTEX_POINT('',#41238) ;
#11861 = VERTEX_POINT('',#41240) ;
#11862 = VERTEX_POINT('',#41242) ;
#11863 = VERTEX_POINT('',#41244) ;
#11864 = VERTEX_POINT('',#41246) ;
#11865 = VERTEX_POINT('',#41250) ;
#11866 = VERTEX_POINT('',#41252) ;
#11867 = VERTEX_POINT('',#41256) ;
#11868 = VERTEX_POINT('',#41258) ;
#11869 = VERTEX_POINT('',#41262) ;
#11870 = VERTEX_POINT('',#41266) ;
#11871 = VERTEX_POINT('',#41270) ;
#11872 = VERTEX_POINT('',#41274) ;
#11873 = VERTEX_POINT('',#41280) ;
#11874 = VERTEX_POINT('',#41282) ;
#11875 = VERTEX_POINT('',#41284) ;
#11876 = VERTEX_POINT('',#41286) ;
#11877 = VERTEX_POINT('',#41288) ;
#11878 = VERTEX_POINT('',#41290) ;
#11879 = VERTEX_POINT('',#41295) ;
#11880 = VERTEX_POINT('',#41297) ;
#11881 = VERTEX_POINT('',#41301) ;
#11882 = VERTEX_POINT('',#41303) ;
#11883 = VERTEX_POINT('',#41305) ;
#11884 = VERTEX_POINT('',#41307) ;
#11885 = VERTEX_POINT('',#41309) ;
#11886 = VERTEX_POINT('',#41311) ;
#11887 = VERTEX_POINT('',#41315) ;
#11888 = VERTEX_POINT('',#41317) ;
#11889 = VERTEX_POINT('',#41321) ;
#11890 = VERTEX_POINT('',#41323) ;
#11891 = VERTEX_POINT('',#41327) ;
#11892 = VERTEX_POINT('',#41333) ;
#11893 = VERTEX_POINT('',#41341) ;
#11894 = VERTEX_POINT('',#41342) ;
#11895 = VERTEX_POINT('',#41344) ;
#11896 = VERTEX_POINT('',#41346) ;
#11897 = VERTEX_POINT('',#41350) ;
#11898 = VERTEX_POINT('',#41354) ;
#11899 = VERTEX_POINT('',#41358) ;
#11900 = VERTEX_POINT('',#41362) ;
#11901 = VERTEX_POINT('',#41366) ;
#11902 = VERTEX_POINT('',#41367) ;
#11903 = VERTEX_POINT('',#41371) ;
#11904 = VERTEX_POINT('',#41373) ;
#11905 = VERTEX_POINT('',#41380) ;
#11906 = VERTEX_POINT('',#41382) ;
#11907 = VERTEX_POINT('',#41386) ;
#11908 = VERTEX_POINT('',#41388) ;
#11909 = VERTEX_POINT('',#41399) ;
#11910 = VERTEX_POINT('',#41400) ;
#11911 = VERTEX_POINT('',#41402) ;
#11912 = VERTEX_POINT('',#41404) ;
#11913 = VERTEX_POINT('',#41408) ;
#11914 = VERTEX_POINT('',#41412) ;
#11915 = VERTEX_POINT('',#41416) ;
#11916 = VERTEX_POINT('',#41420) ;
#11917 = VERTEX_POINT('',#41424) ;
#11918 = VERTEX_POINT('',#41425) ;
#11919 = VERTEX_POINT('',#41429) ;
#11920 = VERTEX_POINT('',#41431) ;
#11921 = VERTEX_POINT('',#41438) ;
#11922 = VERTEX_POINT('',#41440) ;
#11923 = VERTEX_POINT('',#41444) ;
#11924 = VERTEX_POINT('',#41446) ;
#11925 = VERTEX_POINT('',#41457) ;
#11926 = VERTEX_POINT('',#41458) ;
#11927 = VERTEX_POINT('',#41460) ;
#11928 = VERTEX_POINT('',#41462) ;
#11929 = VERTEX_POINT('',#41466) ;
#11930 = VERTEX_POINT('',#41470) ;
#11931 = VERTEX_POINT('',#41474) ;
#11932 = VERTEX_POINT('',#41478) ;
#11933 = VERTEX_POINT('',#41482) ;
#11934 = VERTEX_POINT('',#41483) ;
#11935 = VERTEX_POINT('',#41487) ;
#11936 = VERTEX_POINT('',#41489) ;
#11937 = VERTEX_POINT('',#41496) ;
#11938 = VERTEX_POINT('',#41498) ;
#11939 = VERTEX_POINT('',#41502) ;
#11940 = VERTEX_POINT('',#41504) ;
#11941 = VERTEX_POINT('',#41515) ;
#11942 = VERTEX_POINT('',#41516) ;
#11943 = VERTEX_POINT('',#41518) ;
#11944 = VERTEX_POINT('',#41520) ;
#11945 = VERTEX_POINT('',#41524) ;
#11946 = VERTEX_POINT('',#41528) ;
#11947 = VERTEX_POINT('',#41532) ;
#11948 = VERTEX_POINT('',#41536) ;
#11949 = VERTEX_POINT('',#41540) ;
#11950 = VERTEX_POINT('',#41541) ;
#11951 = VERTEX_POINT('',#41545) ;
#11952 = VERTEX_POINT('',#41547) ;
#11953 = VERTEX_POINT('',#41554) ;
#11954 = VERTEX_POINT('',#41556) ;
#11955 = VERTEX_POINT('',#41560) ;
#11956 = VERTEX_POINT('',#41562) ;
#11957 = VERTEX_POINT('',#41573) ;
#11958 = VERTEX_POINT('',#41575) ;
#11959 = VERTEX_POINT('',#41579) ;
#11960 = VERTEX_POINT('',#41581) ;
#11961 = VERTEX_POINT('',#41587) ;
#11962 = VERTEX_POINT('',#41591) ;
#11963 = VERTEX_POINT('',#41597) ;
#11964 = VERTEX_POINT('',#41598) ;
#11965 = VERTEX_POINT('',#41600) ;
#11966 = VERTEX_POINT('',#41602) ;
#11967 = VERTEX_POINT('',#41606) ;
#11968 = VERTEX_POINT('',#41608) ;
#11969 = VERTEX_POINT('',#41612) ;
#11970 = VERTEX_POINT('',#41614) ;
#11971 = VERTEX_POINT('',#41618) ;
#11972 = VERTEX_POINT('',#41620) ;
#11973 = VERTEX_POINT('',#41622) ;
#11974 = VERTEX_POINT('',#41624) ;
#11975 = VERTEX_POINT('',#41628) ;
#11976 = VERTEX_POINT('',#41630) ;
#11977 = VERTEX_POINT('',#41632) ;
#11978 = VERTEX_POINT('',#41634) ;
#11979 = VERTEX_POINT('',#41645) ;
#11980 = VERTEX_POINT('',#41647) ;
#11981 = VERTEX_POINT('',#41651) ;
#11982 = VERTEX_POINT('',#41654) ;
#11983 = VERTEX_POINT('',#41661) ;
#11984 = VERTEX_POINT('',#41662) ;
#11985 = VERTEX_POINT('',#41664) ;
#11986 = VERTEX_POINT('',#41666) ;
#11987 = VERTEX_POINT('',#41670) ;
#11988 = VERTEX_POINT('',#41671) ;
#11989 = VERTEX_POINT('',#41673) ;
#11990 = VERTEX_POINT('',#41675) ;
#11991 = VERTEX_POINT('',#41688) ;
#11992 = VERTEX_POINT('',#41689) ;
#11993 = VERTEX_POINT('',#41691) ;
#11994 = VERTEX_POINT('',#41693) ;
#11995 = VERTEX_POINT('',#41697) ;
#11996 = VERTEX_POINT('',#41698) ;
#11997 = VERTEX_POINT('',#41700) ;
#11998 = VERTEX_POINT('',#41702) ;
#11999 = VERTEX_POINT('',#41706) ;
#12000 = VERTEX_POINT('',#41707) ;
#12001 = VERTEX_POINT('',#41709) ;
#12002 = VERTEX_POINT('',#41711) ;
#12003 = VERTEX_POINT('',#41715) ;
#12004 = VERTEX_POINT('',#41716) ;
#12005 = VERTEX_POINT('',#41718) ;
#12006 = VERTEX_POINT('',#41720) ;
#12007 = VERTEX_POINT('',#41724) ;
#12008 = VERTEX_POINT('',#41725) ;
#12009 = VERTEX_POINT('',#41727) ;
#12010 = VERTEX_POINT('',#41729) ;
#12011 = VERTEX_POINT('',#41733) ;
#12012 = VERTEX_POINT('',#41734) ;
#12013 = VERTEX_POINT('',#41736) ;
#12014 = VERTEX_POINT('',#41738) ;
#12015 = VERTEX_POINT('',#41742) ;
#12016 = VERTEX_POINT('',#41743) ;
#12017 = VERTEX_POINT('',#41745) ;
#12018 = VERTEX_POINT('',#41747) ;
#12019 = VERTEX_POINT('',#41751) ;
#12020 = VERTEX_POINT('',#41752) ;
#12021 = VERTEX_POINT('',#41754) ;
#12022 = VERTEX_POINT('',#41756) ;
#12023 = VERTEX_POINT('',#41760) ;
#12024 = VERTEX_POINT('',#41761) ;
#12025 = VERTEX_POINT('',#41763) ;
#12026 = VERTEX_POINT('',#41765) ;
#12027 = VERTEX_POINT('',#41769) ;
#12028 = VERTEX_POINT('',#41770) ;
#12029 = VERTEX_POINT('',#41772) ;
#12030 = VERTEX_POINT('',#41774) ;
#12031 = VERTEX_POINT('',#41778) ;
#12032 = VERTEX_POINT('',#41779) ;
#12033 = VERTEX_POINT('',#41781) ;
#12034 = VERTEX_POINT('',#41783) ;
#12035 = VERTEX_POINT('',#41787) ;
#12036 = VERTEX_POINT('',#41788) ;
#12037 = VERTEX_POINT('',#41790) ;
#12038 = VERTEX_POINT('',#41792) ;
#12039 = VERTEX_POINT('',#41796) ;
#12040 = VERTEX_POINT('',#41797) ;
#12041 = VERTEX_POINT('',#41802) ;
#12042 = VERTEX_POINT('',#41803) ;
#12043 = VERTEX_POINT('',#41808) ;
#12044 = VERTEX_POINT('',#41810) ;
#12045 = VERTEX_POINT('',#41814) ;
#12046 = VERTEX_POINT('',#41816) ;
#12047 = VERTEX_POINT('',#41820) ;
#12048 = VERTEX_POINT('',#41822) ;
#12049 = VERTEX_POINT('',#41826) ;
#12050 = VERTEX_POINT('',#41828) ;
#12051 = VERTEX_POINT('',#41832) ;
#12052 = VERTEX_POINT('',#41834) ;
#12053 = VERTEX_POINT('',#41838) ;
#12054 = VERTEX_POINT('',#41840) ;
#12055 = VERTEX_POINT('',#41844) ;
#12056 = VERTEX_POINT('',#41846) ;
#12057 = VERTEX_POINT('',#41850) ;
#12058 = VERTEX_POINT('',#41852) ;
#12059 = VERTEX_POINT('',#41856) ;
#12060 = VERTEX_POINT('',#41858) ;
#12061 = VERTEX_POINT('',#41862) ;
#12062 = VERTEX_POINT('',#41864) ;
#12063 = VERTEX_POINT('',#41868) ;
#12064 = VERTEX_POINT('',#41870) ;
#12065 = VERTEX_POINT('',#41874) ;
#12066 = VERTEX_POINT('',#41876) ;
#12067 = VERTEX_POINT('',#41878) ;
#12068 = VERTEX_POINT('',#41880) ;
#12069 = VERTEX_POINT('',#41882) ;
#12070 = VERTEX_POINT('',#41884) ;
#12071 = VERTEX_POINT('',#41886) ;
#12072 = VERTEX_POINT('',#41888) ;
#12073 = VERTEX_POINT('',#41890) ;
#12074 = VERTEX_POINT('',#41892) ;
#12075 = VERTEX_POINT('',#41894) ;
#12076 = VERTEX_POINT('',#41896) ;
#12077 = VERTEX_POINT('',#41898) ;
#12078 = VERTEX_POINT('',#41900) ;
#12079 = VERTEX_POINT('',#41902) ;
#12080 = VERTEX_POINT('',#41904) ;
#12081 = VERTEX_POINT('',#41906) ;
#12082 = VERTEX_POINT('',#41908) ;
#12083 = VERTEX_POINT('',#41910) ;
#12084 = VERTEX_POINT('',#41912) ;
#12085 = VERTEX_POINT('',#41914) ;
#12086 = VERTEX_POINT('',#41916) ;
#12087 = VERTEX_POINT('',#41918) ;
#12088 = VERTEX_POINT('',#41920) ;
#12089 = VERTEX_POINT('',#41922) ;
#12090 = VERTEX_POINT('',#41924) ;
#12091 = VERTEX_POINT('',#41926) ;
#12092 = VERTEX_POINT('',#41928) ;
#12093 = VERTEX_POINT('',#41930) ;
#12094 = VERTEX_POINT('',#41932) ;
#12095 = VERTEX_POINT('',#41934) ;
#12096 = VERTEX_POINT('',#41936) ;
#12097 = VERTEX_POINT('',#41938) ;
#12098 = VERTEX_POINT('',#41940) ;
#12099 = VERTEX_POINT('',#41942) ;
#12100 = VERTEX_POINT('',#41944) ;
#12101 = VERTEX_POINT('',#41946) ;
#12102 = VERTEX_POINT('',#41948) ;
#12103 = VERTEX_POINT('',#41950) ;
#12104 = VERTEX_POINT('',#41952) ;
#12105 = VERTEX_POINT('',#41954) ;
#12106 = VERTEX_POINT('',#41956) ;
#12107 = VERTEX_POINT('',#41958) ;
#12108 = VERTEX_POINT('',#41960) ;
#12109 = VERTEX_POINT('',#41962) ;
#12110 = VERTEX_POINT('',#41964) ;
#12111 = VERTEX_POINT('',#41966) ;
#12112 = VERTEX_POINT('',#41968) ;
#12113 = VERTEX_POINT('',#41970) ;
#12114 = VERTEX_POINT('',#41972) ;
#12115 = VERTEX_POINT('',#41974) ;
#12116 = VERTEX_POINT('',#41976) ;
#12117 = VERTEX_POINT('',#41978) ;
#12118 = VERTEX_POINT('',#41980) ;
#12119 = VERTEX_POINT('',#41982) ;
#12120 = VERTEX_POINT('',#41984) ;
#12121 = VERTEX_POINT('',#41986) ;
#12122 = VERTEX_POINT('',#41988) ;
#12123 = VERTEX_POINT('',#41990) ;
#12124 = VERTEX_POINT('',#41992) ;
#12125 = VERTEX_POINT('',#41994) ;
#12126 = VERTEX_POINT('',#41996) ;
#12127 = VERTEX_POINT('',#41998) ;
#12128 = VERTEX_POINT('',#42000) ;
#12129 = VERTEX_POINT('',#42002) ;
#12130 = VERTEX_POINT('',#42005) ;
#12131 = VERTEX_POINT('',#42007) ;
#12132 = VERTEX_POINT('',#42009) ;
#12133 = VERTEX_POINT('',#42011) ;
#12134 = VERTEX_POINT('',#42013) ;
#12135 = VERTEX_POINT('',#42015) ;
#12136 = VERTEX_POINT('',#42017) ;
#12137 = VERTEX_POINT('',#42019) ;
#12138 = VERTEX_POINT('',#42021) ;
#12139 = VERTEX_POINT('',#42023) ;
#12140 = VERTEX_POINT('',#42025) ;
#12141 = VERTEX_POINT('',#42027) ;
#12142 = VERTEX_POINT('',#42029) ;
#12143 = VERTEX_POINT('',#42031) ;
#12144 = VERTEX_POINT('',#42033) ;
#12145 = VERTEX_POINT('',#42037) ;
#12146 = VERTEX_POINT('',#42040) ;
#12147 = VERTEX_POINT('',#42044) ;
#12148 = VERTEX_POINT('',#42047) ;
#12149 = VERTEX_POINT('',#42050) ;
#12150 = VERTEX_POINT('',#42053) ;
#12151 = VERTEX_POINT('',#42056) ;
#12152 = VERTEX_POINT('',#42058) ;
#12153 = VERTEX_POINT('',#42061) ;
#12154 = VERTEX_POINT('',#42062) ;
#12155 = VERTEX_POINT('',#42064) ;
#12156 = VERTEX_POINT('',#42067) ;
#12157 = VERTEX_POINT('',#42068) ;
#12158 = VERTEX_POINT('',#42070) ;
#12159 = VERTEX_POINT('',#42072) ;
#12160 = VERTEX_POINT('',#42075) ;
#12161 = VERTEX_POINT('',#42076) ;
#12162 = VERTEX_POINT('',#42078) ;
#12163 = VERTEX_POINT('',#42080) ;
#12164 = VERTEX_POINT('',#42083) ;
#12165 = VERTEX_POINT('',#42084) ;
#12166 = VERTEX_POINT('',#42086) ;
#12167 = VERTEX_POINT('',#42088) ;
#12168 = VERTEX_POINT('',#42091) ;
#12169 = VERTEX_POINT('',#42092) ;
#12170 = VERTEX_POINT('',#42094) ;
#12171 = VERTEX_POINT('',#42096) ;
#12172 = VERTEX_POINT('',#42099) ;
#12173 = VERTEX_POINT('',#42100) ;
#12174 = VERTEX_POINT('',#42102) ;
#12175 = VERTEX_POINT('',#42104) ;
#12176 = VERTEX_POINT('',#42107) ;
#12177 = VERTEX_POINT('',#42108) ;
#12178 = VERTEX_POINT('',#42110) ;
#12179 = VERTEX_POINT('',#42112) ;
#12180 = VERTEX_POINT('',#42115) ;
#12181 = VERTEX_POINT('',#42116) ;
#12182 = VERTEX_POINT('',#42118) ;
#12183 = VERTEX_POINT('',#42120) ;
#12184 = VERTEX_POINT('',#42122) ;
#12185 = VERTEX_POINT('',#42125) ;
#12186 = VERTEX_POINT('',#42126) ;
#12187 = VERTEX_POINT('',#42128) ;
#12188 = VERTEX_POINT('',#42131) ;
#12189 = VERTEX_POINT('',#42132) ;
#12190 = VERTEX_POINT('',#42134) ;
#12191 = VERTEX_POINT('',#42136) ;
#12192 = VERTEX_POINT('',#42139) ;
#12193 = VERTEX_POINT('',#42140) ;
#12194 = VERTEX_POINT('',#42142) ;
#12195 = VERTEX_POINT('',#42144) ;
#12196 = VERTEX_POINT('',#42147) ;
#12197 = VERTEX_POINT('',#42148) ;
#12198 = VERTEX_POINT('',#42150) ;
#12199 = VERTEX_POINT('',#42152) ;
#12200 = VERTEX_POINT('',#42155) ;
#12201 = VERTEX_POINT('',#42156) ;
#12202 = VERTEX_POINT('',#42158) ;
#12203 = VERTEX_POINT('',#42160) ;
#12204 = VERTEX_POINT('',#42163) ;
#12205 = VERTEX_POINT('',#42164) ;
#12206 = VERTEX_POINT('',#42166) ;
#12207 = VERTEX_POINT('',#42168) ;
#12208 = VERTEX_POINT('',#42171) ;
#12209 = VERTEX_POINT('',#42172) ;
#12210 = VERTEX_POINT('',#42174) ;
#12211 = VERTEX_POINT('',#42176) ;
#12212 = VERTEX_POINT('',#42179) ;
#12213 = VERTEX_POINT('',#42180) ;
#12214 = VERTEX_POINT('',#42182) ;
#12215 = VERTEX_POINT('',#42184) ;
#12216 = VERTEX_POINT('',#42187) ;
#12217 = VERTEX_POINT('',#42188) ;
#12218 = VERTEX_POINT('',#42190) ;
#12219 = VERTEX_POINT('',#42192) ;
#12220 = VERTEX_POINT('',#42195) ;
#12221 = VERTEX_POINT('',#42196) ;
#12222 = VERTEX_POINT('',#42198) ;
#12223 = VERTEX_POINT('',#42200) ;
#12224 = VERTEX_POINT('',#42203) ;
#12225 = VERTEX_POINT('',#42204) ;
#12226 = VERTEX_POINT('',#42206) ;
#12227 = VERTEX_POINT('',#42209) ;
#12228 = VERTEX_POINT('',#42210) ;
#12229 = VERTEX_POINT('',#42212) ;
#12230 = VERTEX_POINT('',#42214) ;
#12231 = VERTEX_POINT('',#42216) ;
#12232 = VERTEX_POINT('',#42219) ;
#12233 = VERTEX_POINT('',#42220) ;
#12234 = VERTEX_POINT('',#42222) ;
#12235 = VERTEX_POINT('',#42225) ;
#12236 = VERTEX_POINT('',#42226) ;
#12237 = VERTEX_POINT('',#42228) ;
#12238 = VERTEX_POINT('',#42230) ;
#12239 = VERTEX_POINT('',#42233) ;
#12240 = VERTEX_POINT('',#42234) ;
#12241 = VERTEX_POINT('',#42236) ;
#12242 = VERTEX_POINT('',#42239) ;
#12243 = VERTEX_POINT('',#42240) ;
#12244 = VERTEX_POINT('',#42242) ;
#12245 = VERTEX_POINT('',#42244) ;
#12246 = VERTEX_POINT('',#42247) ;
#12247 = VERTEX_POINT('',#42248) ;
#12248 = VERTEX_POINT('',#42250) ;
#12249 = VERTEX_POINT('',#42252) ;
#12250 = VERTEX_POINT('',#42255) ;
#12251 = VERTEX_POINT('',#42256) ;
#12252 = VERTEX_POINT('',#42258) ;
#12253 = VERTEX_POINT('',#42260) ;
#12254 = VERTEX_POINT('',#42263) ;
#12255 = VERTEX_POINT('',#42264) ;
#12256 = VERTEX_POINT('',#42266) ;
#12257 = VERTEX_POINT('',#42268) ;
#12258 = VERTEX_POINT('',#42271) ;
#12259 = VERTEX_POINT('',#42272) ;
#12260 = VERTEX_POINT('',#42274) ;
#12261 = VERTEX_POINT('',#42276) ;
#12262 = VERTEX_POINT('',#42279) ;
#12263 = VERTEX_POINT('',#42280) ;
#12264 = VERTEX_POINT('',#42282) ;
#12265 = VERTEX_POINT('',#42284) ;
#12266 = VERTEX_POINT('',#42287) ;
#12267 = VERTEX_POINT('',#42288) ;
#12268 = VERTEX_POINT('',#42290) ;
#12269 = VERTEX_POINT('',#42292) ;
#12270 = VERTEX_POINT('',#42295) ;
#12271 = VERTEX_POINT('',#42296) ;
#12272 = VERTEX_POINT('',#42298) ;
#12273 = VERTEX_POINT('',#42301) ;
#12274 = VERTEX_POINT('',#42302) ;
#12275 = VERTEX_POINT('',#42304) ;
#12276 = VERTEX_POINT('',#42306) ;
#12277 = VERTEX_POINT('',#42309) ;
#12278 = VERTEX_POINT('',#42310) ;
#12279 = VERTEX_POINT('',#42312) ;
#12280 = VERTEX_POINT('',#42314) ;
#12281 = VERTEX_POINT('',#42317) ;
#12282 = VERTEX_POINT('',#42318) ;
#12283 = VERTEX_POINT('',#42320) ;
#12284 = VERTEX_POINT('',#42322) ;
#12285 = VERTEX_POINT('',#42325) ;
#12286 = VERTEX_POINT('',#42326) ;
#12287 = VERTEX_POINT('',#42328) ;
#12288 = VERTEX_POINT('',#42330) ;
#12289 = VERTEX_POINT('',#42333) ;
#12290 = VERTEX_POINT('',#42334) ;
#12291 = VERTEX_POINT('',#42336) ;
#12292 = VERTEX_POINT('',#42338) ;
#12293 = VERTEX_POINT('',#42341) ;
#12294 = VERTEX_POINT('',#42342) ;
#12295 = VERTEX_POINT('',#42344) ;
#12296 = VERTEX_POINT('',#42346) ;
#12297 = VERTEX_POINT('',#42349) ;
#12298 = VERTEX_POINT('',#42350) ;
#12299 = VERTEX_POINT('',#42352) ;
#12300 = VERTEX_POINT('',#42354) ;
#12301 = VERTEX_POINT('',#42357) ;
#12302 = VERTEX_POINT('',#42358) ;
#12303 = VERTEX_POINT('',#42360) ;
#12304 = VERTEX_POINT('',#42362) ;
#12305 = VERTEX_POINT('',#42365) ;
#12306 = VERTEX_POINT('',#42366) ;
#12307 = VERTEX_POINT('',#42368) ;
#12308 = VERTEX_POINT('',#42370) ;
#12309 = VERTEX_POINT('',#42373) ;
#12310 = VERTEX_POINT('',#42374) ;
#12311 = VERTEX_POINT('',#42376) ;
#12312 = VERTEX_POINT('',#42378) ;
#12313 = VERTEX_POINT('',#42381) ;
#12314 = VERTEX_POINT('',#42382) ;
#12315 = VERTEX_POINT('',#42384) ;
#12316 = VERTEX_POINT('',#42386) ;
#12317 = VERTEX_POINT('',#42389) ;
#12318 = VERTEX_POINT('',#42391) ;
#12319 = VERTEX_POINT('',#42393) ;
#12320 = VERTEX_POINT('',#42397) ;
#12321 = VERTEX_POINT('',#42401) ;
#12322 = VERTEX_POINT('',#42403) ;
#12323 = VERTEX_POINT('',#42405) ;
#12324 = VERTEX_POINT('',#42407) ;
#12325 = VERTEX_POINT('',#42409) ;
#12326 = VERTEX_POINT('',#42411) ;
#12327 = VERTEX_POINT('',#42413) ;
#12328 = VERTEX_POINT('',#42415) ;
#12329 = VERTEX_POINT('',#42417) ;
#12330 = VERTEX_POINT('',#42419) ;
#12331 = VERTEX_POINT('',#42421) ;
#12332 = VERTEX_POINT('',#42423) ;
#12333 = VERTEX_POINT('',#42425) ;
#12334 = VERTEX_POINT('',#42427) ;
#12335 = VERTEX_POINT('',#42429) ;
#12336 = VERTEX_POINT('',#42432) ;
#12337 = VERTEX_POINT('',#42434) ;
#12338 = VERTEX_POINT('',#42436) ;
#12339 = VERTEX_POINT('',#42438) ;
#12340 = VERTEX_POINT('',#42440) ;
#12341 = VERTEX_POINT('',#42442) ;
#12342 = VERTEX_POINT('',#42444) ;
#12343 = VERTEX_POINT('',#42446) ;
#12344 = VERTEX_POINT('',#42448) ;
#12345 = VERTEX_POINT('',#42450) ;
#12346 = VERTEX_POINT('',#42452) ;
#12347 = VERTEX_POINT('',#42454) ;
#12348 = VERTEX_POINT('',#42456) ;
#12349 = VERTEX_POINT('',#42458) ;
#12350 = VERTEX_POINT('',#42460) ;
#12351 = VERTEX_POINT('',#42462) ;
#12352 = VERTEX_POINT('',#42464) ;
#12353 = VERTEX_POINT('',#42466) ;
#12354 = VERTEX_POINT('',#42468) ;
#12355 = VERTEX_POINT('',#42470) ;
#12356 = VERTEX_POINT('',#42472) ;
#12357 = VERTEX_POINT('',#42474) ;
#12358 = VERTEX_POINT('',#42476) ;
#12359 = VERTEX_POINT('',#42478) ;
#12360 = VERTEX_POINT('',#42480) ;
#12361 = VERTEX_POINT('',#42482) ;
#12362 = VERTEX_POINT('',#42484) ;
#12363 = VERTEX_POINT('',#42486) ;
#12364 = VERTEX_POINT('',#42488) ;
#12365 = VERTEX_POINT('',#42490) ;
#12366 = VERTEX_POINT('',#42492) ;
#12367 = VERTEX_POINT('',#42494) ;
#12368 = VERTEX_POINT('',#42496) ;
#12369 = VERTEX_POINT('',#42498) ;
#12370 = VERTEX_POINT('',#42500) ;
#12371 = VERTEX_POINT('',#42502) ;
#12372 = VERTEX_POINT('',#42504) ;
#12373 = VERTEX_POINT('',#42506) ;
#12374 = VERTEX_POINT('',#42508) ;
#12375 = VERTEX_POINT('',#42510) ;
#12376 = VERTEX_POINT('',#42512) ;
#12377 = VERTEX_POINT('',#42514) ;
#12378 = VERTEX_POINT('',#42516) ;
#12379 = VERTEX_POINT('',#42518) ;
#12380 = VERTEX_POINT('',#42520) ;
#12381 = VERTEX_POINT('',#42522) ;
#12382 = VERTEX_POINT('',#42524) ;
#12383 = VERTEX_POINT('',#42526) ;
#12384 = VERTEX_POINT('',#42528) ;
#12385 = VERTEX_POINT('',#42530) ;
#12386 = VERTEX_POINT('',#42532) ;
#12387 = VERTEX_POINT('',#42534) ;
#12388 = VERTEX_POINT('',#42536) ;
#12389 = VERTEX_POINT('',#42538) ;
#12390 = VERTEX_POINT('',#42540) ;
#12391 = VERTEX_POINT('',#42542) ;
#12392 = VERTEX_POINT('',#42544) ;
#12393 = VERTEX_POINT('',#42546) ;
#12394 = VERTEX_POINT('',#42548) ;
#12395 = VERTEX_POINT('',#42550) ;
#12396 = VERTEX_POINT('',#42552) ;
#12397 = VERTEX_POINT('',#42554) ;
#12398 = VERTEX_POINT('',#42556) ;
#12399 = VERTEX_POINT('',#42558) ;
#12400 = VERTEX_POINT('',#42560) ;
#12401 = VERTEX_POINT('',#42563) ;
#12402 = VERTEX_POINT('',#42566) ;
#12403 = VERTEX_POINT('',#42569) ;
#12404 = VERTEX_POINT('',#42572) ;
#12405 = VERTEX_POINT('',#42575) ;
#12406 = VERTEX_POINT('',#42577) ;
#12407 = VERTEX_POINT('',#42580) ;
#12408 = VERTEX_POINT('',#42583) ;
#12409 = VERTEX_POINT('',#42587) ;
#12410 = VERTEX_POINT('',#42589) ;
#12411 = VERTEX_POINT('',#42593) ;
#12412 = VERTEX_POINT('',#42594) ;
#12413 = VERTEX_POINT('',#42596) ;
#12414 = VERTEX_POINT('',#42598) ;
#12415 = VERTEX_POINT('',#42600) ;
#12416 = VERTEX_POINT('',#42603) ;
#12417 = VERTEX_POINT('',#42604) ;
#12418 = VERTEX_POINT('',#42606) ;
#12419 = VERTEX_POINT('',#42608) ;
#12420 = VERTEX_POINT('',#42611) ;
#12421 = VERTEX_POINT('',#42612) ;
#12422 = VERTEX_POINT('',#42614) ;
#12423 = VERTEX_POINT('',#42616) ;
#12424 = VERTEX_POINT('',#42619) ;
#12425 = VERTEX_POINT('',#42620) ;
#12426 = VERTEX_POINT('',#42622) ;
#12427 = VERTEX_POINT('',#42624) ;
#12428 = VERTEX_POINT('',#42627) ;
#12429 = VERTEX_POINT('',#42628) ;
#12430 = VERTEX_POINT('',#42630) ;
#12431 = VERTEX_POINT('',#42632) ;
#12432 = VERTEX_POINT('',#42635) ;
#12433 = VERTEX_POINT('',#42636) ;
#12434 = VERTEX_POINT('',#42638) ;
#12435 = VERTEX_POINT('',#42641) ;
#12436 = VERTEX_POINT('',#42642) ;
#12437 = VERTEX_POINT('',#42644) ;
#12438 = VERTEX_POINT('',#42646) ;
#12439 = VERTEX_POINT('',#42649) ;
#12440 = VERTEX_POINT('',#42650) ;
#12441 = VERTEX_POINT('',#42652) ;
#12442 = VERTEX_POINT('',#42654) ;
#12443 = VERTEX_POINT('',#42657) ;
#12444 = VERTEX_POINT('',#42658) ;
#12445 = VERTEX_POINT('',#42660) ;
#12446 = VERTEX_POINT('',#42662) ;
#12447 = VERTEX_POINT('',#42665) ;
#12448 = VERTEX_POINT('',#42666) ;
#12449 = VERTEX_POINT('',#42668) ;
#12450 = VERTEX_POINT('',#42670) ;
#12451 = VERTEX_POINT('',#42673) ;
#12452 = VERTEX_POINT('',#42674) ;
#12453 = VERTEX_POINT('',#42676) ;
#12454 = VERTEX_POINT('',#42678) ;
#12455 = VERTEX_POINT('',#42681) ;
#12456 = VERTEX_POINT('',#42682) ;
#12457 = VERTEX_POINT('',#42684) ;
#12458 = VERTEX_POINT('',#42686) ;
#12459 = VERTEX_POINT('',#42689) ;
#12460 = VERTEX_POINT('',#42690) ;
#12461 = VERTEX_POINT('',#42692) ;
#12462 = VERTEX_POINT('',#42694) ;
#12463 = VERTEX_POINT('',#42697) ;
#12464 = VERTEX_POINT('',#42698) ;
#12465 = VERTEX_POINT('',#42700) ;
#12466 = VERTEX_POINT('',#42702) ;
#12467 = VERTEX_POINT('',#42705) ;
#12468 = VERTEX_POINT('',#42706) ;
#12469 = VERTEX_POINT('',#42708) ;
#12470 = VERTEX_POINT('',#42710) ;
#12471 = VERTEX_POINT('',#42712) ;
#12472 = VERTEX_POINT('',#42715) ;
#12473 = VERTEX_POINT('',#42716) ;
#12474 = VERTEX_POINT('',#42718) ;
#12475 = VERTEX_POINT('',#42721) ;
#12476 = VERTEX_POINT('',#42722) ;
#12477 = VERTEX_POINT('',#42724) ;
#12478 = VERTEX_POINT('',#42726) ;
#12479 = VERTEX_POINT('',#42729) ;
#12480 = VERTEX_POINT('',#42730) ;
#12481 = VERTEX_POINT('',#42732) ;
#12482 = VERTEX_POINT('',#42735) ;
#12483 = VERTEX_POINT('',#42736) ;
#12484 = VERTEX_POINT('',#42738) ;
#12485 = VERTEX_POINT('',#42740) ;
#12486 = VERTEX_POINT('',#42743) ;
#12487 = VERTEX_POINT('',#42744) ;
#12488 = VERTEX_POINT('',#42746) ;
#12489 = VERTEX_POINT('',#42748) ;
#12490 = VERTEX_POINT('',#42751) ;
#12491 = VERTEX_POINT('',#42752) ;
#12492 = VERTEX_POINT('',#42754) ;
#12493 = VERTEX_POINT('',#42756) ;
#12494 = VERTEX_POINT('',#42759) ;
#12495 = VERTEX_POINT('',#42760) ;
#12496 = VERTEX_POINT('',#42762) ;
#12497 = VERTEX_POINT('',#42764) ;
#12498 = VERTEX_POINT('',#42767) ;
#12499 = VERTEX_POINT('',#42768) ;
#12500 = VERTEX_POINT('',#42770) ;
#12501 = VERTEX_POINT('',#42772) ;
#12502 = VERTEX_POINT('',#42775) ;
#12503 = VERTEX_POINT('',#42776) ;
#12504 = VERTEX_POINT('',#42778) ;
#12505 = VERTEX_POINT('',#42780) ;
#12506 = VERTEX_POINT('',#42783) ;
#12507 = VERTEX_POINT('',#42784) ;
#12508 = VERTEX_POINT('',#42786) ;
#12509 = VERTEX_POINT('',#42788) ;
#12510 = VERTEX_POINT('',#42791) ;
#12511 = VERTEX_POINT('',#42792) ;
#12512 = VERTEX_POINT('',#42794) ;
#12513 = VERTEX_POINT('',#42796) ;
#12514 = VERTEX_POINT('',#42799) ;
#12515 = VERTEX_POINT('',#42800) ;
#12516 = VERTEX_POINT('',#42802) ;
#12517 = VERTEX_POINT('',#42804) ;
#12518 = VERTEX_POINT('',#42807) ;
#12519 = VERTEX_POINT('',#42808) ;
#12520 = VERTEX_POINT('',#42810) ;
#12521 = VERTEX_POINT('',#42813) ;
#12522 = VERTEX_POINT('',#42814) ;
#12523 = VERTEX_POINT('',#42816) ;
#12524 = VERTEX_POINT('',#42818) ;
#12525 = VERTEX_POINT('',#42821) ;
#12526 = VERTEX_POINT('',#42822) ;
#12527 = VERTEX_POINT('',#42824) ;
#12528 = VERTEX_POINT('',#42826) ;
#12529 = VERTEX_POINT('',#42829) ;
#12530 = VERTEX_POINT('',#42830) ;
#12531 = VERTEX_POINT('',#42832) ;
#12532 = VERTEX_POINT('',#42834) ;
#12533 = VERTEX_POINT('',#42837) ;
#12534 = VERTEX_POINT('',#42838) ;
#12535 = VERTEX_POINT('',#42840) ;
#12536 = VERTEX_POINT('',#42842) ;
#12537 = VERTEX_POINT('',#42845) ;
#12538 = VERTEX_POINT('',#42846) ;
#12539 = VERTEX_POINT('',#42848) ;
#12540 = VERTEX_POINT('',#42850) ;
#12541 = VERTEX_POINT('',#42853) ;
#12542 = VERTEX_POINT('',#42854) ;
#12543 = VERTEX_POINT('',#42856) ;
#12544 = VERTEX_POINT('',#42858) ;
#12545 = VERTEX_POINT('',#42861) ;
#12546 = VERTEX_POINT('',#42862) ;
#12547 = VERTEX_POINT('',#42864) ;
#12548 = VERTEX_POINT('',#42866) ;
#12549 = VERTEX_POINT('',#42869) ;
#12550 = VERTEX_POINT('',#42870) ;
#12551 = VERTEX_POINT('',#42872) ;
#12552 = VERTEX_POINT('',#42874) ;
#12553 = VERTEX_POINT('',#42877) ;
#12554 = VERTEX_POINT('',#42878) ;
#12555 = VERTEX_POINT('',#42880) ;
#12556 = VERTEX_POINT('',#42882) ;
#12557 = VERTEX_POINT('',#42885) ;
#12558 = VERTEX_POINT('',#42886) ;
#12559 = VERTEX_POINT('',#42888) ;
#12560 = VERTEX_POINT('',#42891) ;
#12561 = VERTEX_POINT('',#42892) ;
#12562 = VERTEX_POINT('',#42894) ;
#12563 = VERTEX_POINT('',#42897) ;
#12564 = VERTEX_POINT('',#42898) ;
#12565 = VERTEX_POINT('',#42900) ;
#12566 = VERTEX_POINT('',#42902) ;
#12567 = VERTEX_POINT('',#42905) ;
#12568 = VERTEX_POINT('',#42906) ;
#12569 = VERTEX_POINT('',#42908) ;
#12570 = VERTEX_POINT('',#42910) ;
#12571 = VERTEX_POINT('',#42913) ;
#12572 = VERTEX_POINT('',#42914) ;
#12573 = VERTEX_POINT('',#42916) ;
#12574 = VERTEX_POINT('',#42918) ;
#12575 = VERTEX_POINT('',#43443) ;
#12576 = VERTEX_POINT('',#43444) ;
#12577 = VERTEX_POINT('',#43448) ;
#12578 = VERTEX_POINT('',#43449) ;
#12579 = VERTEX_POINT('',#43453) ;
#12580 = VERTEX_POINT('',#43454) ;
#12581 = VERTEX_POINT('',#43458) ;
#12582 = VERTEX_POINT('',#43459) ;
#12583 = VERTEX_POINT('',#43463) ;
#12584 = VERTEX_POINT('',#43464) ;
#12585 = VERTEX_POINT('',#43468) ;
#12586 = VERTEX_POINT('',#43469) ;
#12587 = VERTEX_POINT('',#43473) ;
#12588 = VERTEX_POINT('',#43474) ;
#12589 = VERTEX_POINT('',#43478) ;
#12590 = VERTEX_POINT('',#43479) ;
#12591 = VERTEX_POINT('',#43481) ;
#12592 = VERTEX_POINT('',#43485) ;
#12593 = VERTEX_POINT('',#43486) ;
#12594 = VERTEX_POINT('',#43488) ;
#12595 = VERTEX_POINT('',#43490) ;
#12596 = VERTEX_POINT('',#43494) ;
#12597 = VERTEX_POINT('',#43495) ;
#12598 = VERTEX_POINT('',#43497) ;
#12599 = VERTEX_POINT('',#43499) ;
#12600 = VERTEX_POINT('',#43503) ;
#12601 = VERTEX_POINT('',#43504) ;
#12602 = VERTEX_POINT('',#43506) ;
#12603 = VERTEX_POINT('',#43508) ;
#12604 = VERTEX_POINT('',#43512) ;
#12605 = VERTEX_POINT('',#43513) ;
#12606 = VERTEX_POINT('',#43515) ;
#12607 = VERTEX_POINT('',#43517) ;
#12608 = VERTEX_POINT('',#43521) ;
#12609 = VERTEX_POINT('',#43522) ;
#12610 = VERTEX_POINT('',#43524) ;
#12611 = VERTEX_POINT('',#43526) ;
#12612 = VERTEX_POINT('',#43530) ;
#12613 = VERTEX_POINT('',#43531) ;
#12614 = VERTEX_POINT('',#43533) ;
#12615 = VERTEX_POINT('',#43535) ;
#12616 = VERTEX_POINT('',#43539) ;
#12617 = VERTEX_POINT('',#43540) ;
#12618 = VERTEX_POINT('',#43542) ;
#12619 = VERTEX_POINT('',#43544) ;
#12620 = VERTEX_POINT('',#43548) ;
#12621 = VERTEX_POINT('',#43549) ;
#12622 = VERTEX_POINT('',#43551) ;
#12623 = VERTEX_POINT('',#43553) ;
#12624 = VERTEX_POINT('',#43557) ;
#12625 = VERTEX_POINT('',#43558) ;
#12626 = VERTEX_POINT('',#43560) ;
#12627 = VERTEX_POINT('',#43562) ;
#12628 = VERTEX_POINT('',#43566) ;
#12629 = VERTEX_POINT('',#43567) ;
#12630 = VERTEX_POINT('',#43569) ;
#12631 = VERTEX_POINT('',#43571) ;
#12632 = VERTEX_POINT('',#43575) ;
#12633 = VERTEX_POINT('',#43576) ;
#12634 = VERTEX_POINT('',#43578) ;
#12635 = VERTEX_POINT('',#43580) ;
#12636 = VERTEX_POINT('',#43584) ;
#12637 = VERTEX_POINT('',#43585) ;
#12638 = VERTEX_POINT('',#43587) ;
#12639 = VERTEX_POINT('',#43589) ;
#12640 = VERTEX_POINT('',#43593) ;
#12641 = VERTEX_POINT('',#43594) ;
#12642 = VERTEX_POINT('',#43596) ;
#12643 = VERTEX_POINT('',#43598) ;
#12644 = VERTEX_POINT('',#43602) ;
#12645 = VERTEX_POINT('',#43603) ;
#12646 = VERTEX_POINT('',#43605) ;
#12647 = VERTEX_POINT('',#43609) ;
#12648 = VERTEX_POINT('',#43610) ;
#12649 = VERTEX_POINT('',#43614) ;
#12650 = VERTEX_POINT('',#43615) ;
#12651 = VERTEX_POINT('',#43619) ;
#12652 = VERTEX_POINT('',#43620) ;
#12653 = VERTEX_POINT('',#43624) ;
#12654 = VERTEX_POINT('',#43625) ;
#12655 = VERTEX_POINT('',#43629) ;
#12656 = VERTEX_POINT('',#43630) ;
#12657 = VERTEX_POINT('',#43634) ;
#12658 = VERTEX_POINT('',#43635) ;
#12659 = VERTEX_POINT('',#43639) ;
#12660 = VERTEX_POINT('',#43642) ;
#12661 = VERTEX_POINT('',#43647) ;
#12662 = VERTEX_POINT('',#43652) ;
#12663 = VERTEX_POINT('',#43657) ;
#12664 = VERTEX_POINT('',#43662) ;
#12665 = VERTEX_POINT('',#43667) ;
#12666 = VERTEX_POINT('',#43672) ;
#12667 = VERTEX_POINT('',#43717) ;
#12668 = VERTEX_POINT('',#43721) ;
#12669 = VERTEX_POINT('',#43726) ;
#12670 = VERTEX_POINT('',#43731) ;
#12671 = VERTEX_POINT('',#43736) ;
#12672 = VERTEX_POINT('',#43741) ;
#12673 = VERTEX_POINT('',#43746) ;
#12674 = VERTEX_POINT('',#43761) ;
#12675 = VERTEX_POINT('',#43763) ;
#12676 = VERTEX_POINT('',#43767) ;
#12677 = VERTEX_POINT('',#43769) ;
#12678 = VERTEX_POINT('',#43773) ;
#12679 = VERTEX_POINT('',#43775) ;
#12680 = VERTEX_POINT('',#43779) ;
#12681 = VERTEX_POINT('',#43781) ;
#12682 = VERTEX_POINT('',#43785) ;
#12683 = VERTEX_POINT('',#43787) ;
#12684 = VERTEX_POINT('',#43791) ;
#12685 = VERTEX_POINT('',#43793) ;
#12686 = VERTEX_POINT('',#43797) ;
#12687 = VERTEX_POINT('',#43798) ;
#12688 = VERTEX_POINT('',#43800) ;
#12689 = VERTEX_POINT('',#43802) ;
#12690 = VERTEX_POINT('',#43806) ;
#12691 = VERTEX_POINT('',#43807) ;
#12692 = VERTEX_POINT('',#43809) ;
#12693 = VERTEX_POINT('',#43811) ;
#12694 = VERTEX_POINT('',#43816) ;
#12695 = VERTEX_POINT('',#43818) ;
#12696 = VERTEX_POINT('',#43822) ;
#12697 = VERTEX_POINT('',#43824) ;
#12698 = VERTEX_POINT('',#43835) ;
#12699 = VERTEX_POINT('',#43837) ;
#12700 = VERTEX_POINT('',#43841) ;
#12701 = VERTEX_POINT('',#43843) ;
#12702 = VERTEX_POINT('',#43847) ;
#12703 = VERTEX_POINT('',#43848) ;
#12704 = VERTEX_POINT('',#43850) ;
#12705 = VERTEX_POINT('',#43852) ;
#12706 = VERTEX_POINT('',#43856) ;
#12707 = VERTEX_POINT('',#43857) ;
#12708 = VERTEX_POINT('',#43859) ;
#12709 = VERTEX_POINT('',#43861) ;
#12710 = VERTEX_POINT('',#43866) ;
#12711 = VERTEX_POINT('',#43868) ;
#12712 = VERTEX_POINT('',#43872) ;
#12713 = VERTEX_POINT('',#43874) ;
#12714 = VERTEX_POINT('',#43885) ;
#12715 = VERTEX_POINT('',#43887) ;
#12716 = VERTEX_POINT('',#43891) ;
#12717 = VERTEX_POINT('',#43893) ;
#12718 = VERTEX_POINT('',#43897) ;
#12719 = VERTEX_POINT('',#43899) ;
#12720 = VERTEX_POINT('',#43903) ;
#12721 = VERTEX_POINT('',#43905) ;
#12722 = VERTEX_POINT('',#43910) ;
#12723 = VERTEX_POINT('',#43911) ;
#12724 = VERTEX_POINT('',#43913) ;
#12725 = VERTEX_POINT('',#43915) ;
#12726 = VERTEX_POINT('',#43917) ;
#12727 = VERTEX_POINT('',#43920) ;
#12728 = VERTEX_POINT('',#43923) ;
#12729 = VERTEX_POINT('',#43925) ;
#12730 = VERTEX_POINT('',#43929) ;
#12731 = VERTEX_POINT('',#43935) ;
#12732 = VERTEX_POINT('',#43936) ;
#12733 = VERTEX_POINT('',#43938) ;
#12734 = VERTEX_POINT('',#43940) ;
#12735 = VERTEX_POINT('',#43944) ;
#12736 = VERTEX_POINT('',#43946) ;
#12737 = VERTEX_POINT('',#43950) ;
#12738 = VERTEX_POINT('',#43952) ;
#12739 = VERTEX_POINT('',#43959) ;
#12740 = VERTEX_POINT('',#43960) ;
#12741 = VERTEX_POINT('',#43962) ;
#12742 = VERTEX_POINT('',#43964) ;
#12743 = VERTEX_POINT('',#43968) ;
#12744 = VERTEX_POINT('',#43970) ;
#12745 = VERTEX_POINT('',#43974) ;
#12746 = VERTEX_POINT('',#43976) ;
#12747 = VERTEX_POINT('',#43980) ;
#12748 = VERTEX_POINT('',#43982) ;
#12749 = VERTEX_POINT('',#43984) ;
#12750 = VERTEX_POINT('',#43989) ;
#12751 = VERTEX_POINT('',#43990) ;
#12752 = VERTEX_POINT('',#43992) ;
#12753 = VERTEX_POINT('',#43994) ;
#12754 = VERTEX_POINT('',#43998) ;
#12755 = VERTEX_POINT('',#44001) ;
#12756 = VERTEX_POINT('',#44002) ;
#12757 = VERTEX_POINT('',#44004) ;
#12758 = VERTEX_POINT('',#44006) ;
#12759 = VERTEX_POINT('',#44010) ;
#12760 = VERTEX_POINT('',#44012) ;
#12761 = VERTEX_POINT('',#44014) ;
#12762 = VERTEX_POINT('',#44016) ;
#12763 = VERTEX_POINT('',#44019) ;
#12764 = VERTEX_POINT('',#44021) ;
#12765 = VERTEX_POINT('',#44025) ;
#12766 = VERTEX_POINT('',#44026) ;
#12767 = VERTEX_POINT('',#44028) ;
#12768 = VERTEX_POINT('',#44031) ;
#12769 = VERTEX_POINT('',#44033) ;
#12770 = VERTEX_POINT('',#44035) ;
#12771 = VERTEX_POINT('',#44041) ;
#12772 = VERTEX_POINT('',#44043) ;
#12773 = VERTEX_POINT('',#44045) ;
#12774 = VERTEX_POINT('',#44049) ;
#12775 = VERTEX_POINT('',#44051) ;
#12776 = VERTEX_POINT('',#44055) ;
#12777 = VERTEX_POINT('',#44057) ;
#12778 = VERTEX_POINT('',#44061) ;
#12779 = VERTEX_POINT('',#44062) ;
#12780 = VERTEX_POINT('',#44064) ;
#12781 = VERTEX_POINT('',#44066) ;
#12782 = VERTEX_POINT('',#44070) ;
#12783 = VERTEX_POINT('',#44071) ;
#12784 = VERTEX_POINT('',#44073) ;
#12785 = VERTEX_POINT('',#44075) ;
#12786 = VERTEX_POINT('',#44079) ;
#12787 = VERTEX_POINT('',#44080) ;
#12788 = VERTEX_POINT('',#44082) ;
#12789 = VERTEX_POINT('',#44084) ;
#12790 = VERTEX_POINT('',#44088) ;
#12791 = VERTEX_POINT('',#44090) ;
#12792 = VERTEX_POINT('',#44094) ;
#12793 = VERTEX_POINT('',#44095) ;
#12794 = VERTEX_POINT('',#44097) ;
#12795 = VERTEX_POINT('',#44099) ;
#12796 = VERTEX_POINT('',#44103) ;
#12797 = VERTEX_POINT('',#44105) ;
#12798 = VERTEX_POINT('',#44110) ;
#12799 = VERTEX_POINT('',#44111) ;
#12800 = VERTEX_POINT('',#44113) ;
#12801 = VERTEX_POINT('',#44115) ;
#12802 = VERTEX_POINT('',#44117) ;
#12803 = VERTEX_POINT('',#44119) ;
#12804 = VERTEX_POINT('',#44122) ;
#12805 = VERTEX_POINT('',#44125) ;
#12806 = VERTEX_POINT('',#44127) ;
#12807 = VERTEX_POINT('',#44129) ;
#12808 = VERTEX_POINT('',#44131) ;
#12809 = VERTEX_POINT('',#44133) ;
#12810 = VERTEX_POINT('',#44135) ;
#12811 = VERTEX_POINT('',#44138) ;
#12812 = VERTEX_POINT('',#44139) ;
#12813 = VERTEX_POINT('',#44141) ;
#12814 = VERTEX_POINT('',#44144) ;
#12815 = VERTEX_POINT('',#44146) ;
#12816 = VERTEX_POINT('',#44151) ;
#12817 = VERTEX_POINT('',#44153) ;
#12818 = VERTEX_POINT('',#44157) ;
#12819 = VERTEX_POINT('',#44161) ;
#12820 = VERTEX_POINT('',#44165) ;
#12821 = VERTEX_POINT('',#44167) ;
#12822 = VERTEX_POINT('',#44171) ;
#12823 = VERTEX_POINT('',#44175) ;
#12824 = VERTEX_POINT('',#44177) ;
#12825 = VERTEX_POINT('',#44181) ;
#12826 = VERTEX_POINT('',#44186) ;
#12827 = VERTEX_POINT('',#44190) ;
#12828 = VERTEX_POINT('',#44194) ;
#12829 = VERTEX_POINT('',#44197) ;
#12830 = VERTEX_POINT('',#44200) ;
#12831 = VERTEX_POINT('',#44203) ;
#12832 = VERTEX_POINT('',#44207) ;
#12833 = VERTEX_POINT('',#44209) ;
#12834 = VERTEX_POINT('',#44225) ;
#12835 = VERTEX_POINT('',#44227) ;
#12836 = VERTEX_POINT('',#44230) ;
#12837 = VERTEX_POINT('',#44232) ;
#12838 = VERTEX_POINT('',#44243) ;
#12839 = VERTEX_POINT('',#44245) ;
#12840 = VERTEX_POINT('',#44249) ;
#12841 = VERTEX_POINT('',#44250) ;
#12842 = VERTEX_POINT('',#44252) ;
#12843 = VERTEX_POINT('',#44254) ;
#12844 = VERTEX_POINT('',#44258) ;
#12845 = VERTEX_POINT('',#44259) ;
#12846 = VERTEX_POINT('',#44261) ;
#12847 = VERTEX_POINT('',#44263) ;
#12848 = VERTEX_POINT('',#44270) ;
#12849 = VERTEX_POINT('',#44271) ;
#12850 = VERTEX_POINT('',#44283) ;
#12851 = VERTEX_POINT('',#44284) ;
#12852 = VERTEX_POINT('',#44286) ;
#12853 = VERTEX_POINT('',#44288) ;
#12854 = VERTEX_POINT('',#44299) ;
#12855 = VERTEX_POINT('',#44300) ;
#12856 = VERTEX_POINT('',#44302) ;
#12857 = VERTEX_POINT('',#44304) ;
#12858 = VERTEX_POINT('',#44316) ;
#12859 = VERTEX_POINT('',#44319) ;
#12860 = VERTEX_POINT('',#44321) ;
#12861 = VERTEX_POINT('',#44324) ;
#12862 = VERTEX_POINT('',#44330) ;
#12863 = VERTEX_POINT('',#44333) ;
#12864 = VERTEX_POINT('',#44335) ;
#12865 = VERTEX_POINT('',#44342) ;
#12866 = VERTEX_POINT('',#44343) ;
#12867 = VERTEX_POINT('',#44355) ;
#12868 = VERTEX_POINT('',#44357) ;
#12869 = VERTEX_POINT('',#44370) ;
#12870 = VERTEX_POINT('',#44374) ;
#12871 = VERTEX_POINT('',#44376) ;
#12872 = VERTEX_POINT('',#44380) ;
#12873 = VERTEX_POINT('',#44381) ;
#12874 = VERTEX_POINT('',#44383) ;
#12875 = VERTEX_POINT('',#44385) ;
#12876 = VERTEX_POINT('',#44389) ;
#12877 = VERTEX_POINT('',#44390) ;
#12878 = VERTEX_POINT('',#44392) ;
#12879 = VERTEX_POINT('',#44394) ;
#12880 = VERTEX_POINT('',#44409) ;
#12881 = VERTEX_POINT('',#44410) ;
#12882 = VERTEX_POINT('',#44412) ;
#12883 = VERTEX_POINT('',#44414) ;
#12884 = VERTEX_POINT('',#44418) ;
#12885 = VERTEX_POINT('',#44420) ;
#12886 = VERTEX_POINT('',#44424) ;
#12887 = VERTEX_POINT('',#44428) ;
#12888 = VERTEX_POINT('',#44435) ;
#12889 = VERTEX_POINT('',#44436) ;
#12890 = VERTEX_POINT('',#44438) ;
#12891 = VERTEX_POINT('',#44440) ;
#12892 = VERTEX_POINT('',#44444) ;
#12893 = VERTEX_POINT('',#44445) ;
#12894 = VERTEX_POINT('',#44450) ;
#12895 = VERTEX_POINT('',#44454) ;
#12896 = VERTEX_POINT('',#44461) ;
#12897 = VERTEX_POINT('',#44462) ;
#12898 = VERTEX_POINT('',#44466) ;
#12899 = VERTEX_POINT('',#44467) ;
#12900 = VERTEX_POINT('',#44475) ;
#12901 = VERTEX_POINT('',#44476) ;
#12902 = VERTEX_POINT('',#44478) ;
#12903 = VERTEX_POINT('',#44480) ;
#12904 = VERTEX_POINT('',#44484) ;
#12905 = VERTEX_POINT('',#44486) ;
#12906 = VERTEX_POINT('',#44495) ;
#12907 = VERTEX_POINT('',#44496) ;
#12908 = VERTEX_POINT('',#44498) ;
#12909 = VERTEX_POINT('',#44502) ;
#12910 = VERTEX_POINT('',#44504) ;
#12911 = VERTEX_POINT('',#44508) ;
#12912 = VERTEX_POINT('',#44515) ;
#12913 = VERTEX_POINT('',#44516) ;
#12914 = VERTEX_POINT('',#44518) ;
#12915 = VERTEX_POINT('',#44520) ;
#12916 = VERTEX_POINT('',#44524) ;
#12917 = VERTEX_POINT('',#44526) ;
#12918 = VERTEX_POINT('',#44535) ;
#12919 = VERTEX_POINT('',#44536) ;
#12920 = VERTEX_POINT('',#44538) ;
#12921 = VERTEX_POINT('',#44542) ;
#12922 = VERTEX_POINT('',#44543) ;
#12923 = VERTEX_POINT('',#44545) ;
#12924 = VERTEX_POINT('',#44555) ;
#12925 = VERTEX_POINT('',#44556) ;
#12926 = VERTEX_POINT('',#44558) ;
#12927 = VERTEX_POINT('',#44560) ;
#12928 = VERTEX_POINT('',#44564) ;
#12929 = VERTEX_POINT('',#44566) ;
#12930 = VERTEX_POINT('',#44575) ;
#12931 = VERTEX_POINT('',#44576) ;
#12932 = VERTEX_POINT('',#44578) ;
#12933 = VERTEX_POINT('',#44582) ;
#12934 = VERTEX_POINT('',#44583) ;
#12935 = VERTEX_POINT('',#44585) ;
#12936 = VERTEX_POINT('',#44595) ;
#12937 = VERTEX_POINT('',#44596) ;
#12938 = VERTEX_POINT('',#44598) ;
#12939 = VERTEX_POINT('',#44600) ;
#12940 = VERTEX_POINT('',#44609) ;
#12941 = VERTEX_POINT('',#44610) ;
#12942 = VERTEX_POINT('',#44612) ;
#12943 = VERTEX_POINT('',#44614) ;
#12944 = VERTEX_POINT('',#44623) ;
#12945 = VERTEX_POINT('',#44624) ;
#12946 = VERTEX_POINT('',#44626) ;
#12947 = VERTEX_POINT('',#44628) ;
#12948 = VERTEX_POINT('',#44637) ;
#12949 = VERTEX_POINT('',#44638) ;
#12950 = VERTEX_POINT('',#44640) ;
#12951 = VERTEX_POINT('',#44642) ;
#12952 = VERTEX_POINT('',#44651) ;
#12953 = VERTEX_POINT('',#44652) ;
#12954 = VERTEX_POINT('',#44654) ;
#12955 = VERTEX_POINT('',#44656) ;
#12956 = VERTEX_POINT('',#44665) ;
#12957 = VERTEX_POINT('',#44666) ;
#12958 = VERTEX_POINT('',#44668) ;
#12959 = VERTEX_POINT('',#44670) ;
#12960 = VERTEX_POINT('',#44674) ;
#12961 = VERTEX_POINT('',#44676) ;
#12962 = VERTEX_POINT('',#44680) ;
#12963 = VERTEX_POINT('',#44682) ;
#12964 = VERTEX_POINT('',#44691) ;
#12965 = VERTEX_POINT('',#44692) ;
#12966 = VERTEX_POINT('',#44694) ;
#12967 = VERTEX_POINT('',#44696) ;
#12968 = VERTEX_POINT('',#44700) ;
#12969 = VERTEX_POINT('',#44701) ;
#12970 = VERTEX_POINT('',#44703) ;
#12971 = VERTEX_POINT('',#44705) ;
#12972 = VERTEX_POINT('',#44717) ;
#12973 = VERTEX_POINT('',#44718) ;
#12974 = VERTEX_POINT('',#44720) ;
#12975 = VERTEX_POINT('',#44722) ;
#12976 = VERTEX_POINT('',#44726) ;
#12977 = VERTEX_POINT('',#44728) ;
#12978 = VERTEX_POINT('',#44732) ;
#12979 = VERTEX_POINT('',#44734) ;
#12980 = VERTEX_POINT('',#44738) ;
#12981 = VERTEX_POINT('',#44740) ;
#12982 = VERTEX_POINT('',#44742) ;
#12983 = VERTEX_POINT('',#44744) ;
#12984 = VERTEX_POINT('',#44746) ;
#12985 = VERTEX_POINT('',#44748) ;
#12986 = VERTEX_POINT('',#44750) ;
#12987 = VERTEX_POINT('',#44752) ;
#12988 = VERTEX_POINT('',#44756) ;
#12989 = VERTEX_POINT('',#44760) ;
#12990 = VERTEX_POINT('',#44764) ;
#12991 = VERTEX_POINT('',#44766) ;
#12992 = VERTEX_POINT('',#44768) ;
#12993 = VERTEX_POINT('',#44770) ;
#12994 = VERTEX_POINT('',#44772) ;
#12995 = VERTEX_POINT('',#44774) ;
#12996 = VERTEX_POINT('',#44791) ;
#12997 = VERTEX_POINT('',#44792) ;
#12998 = VERTEX_POINT('',#44794) ;
#12999 = VERTEX_POINT('',#44796) ;
#13000 = VERTEX_POINT('',#44805) ;
#13001 = VERTEX_POINT('',#44806) ;
#13002 = VERTEX_POINT('',#44810) ;
#13003 = VERTEX_POINT('',#44812) ;
#13004 = VERTEX_POINT('',#44816) ;
#13005 = VERTEX_POINT('',#44818) ;
#13006 = VERTEX_POINT('',#44820) ;
#13007 = VERTEX_POINT('',#44822) ;
#13008 = VERTEX_POINT('',#44824) ;
#13009 = VERTEX_POINT('',#44826) ;
#13010 = VERTEX_POINT('',#44828) ;
#13011 = VERTEX_POINT('',#44830) ;
#13012 = VERTEX_POINT('',#44844) ;
#13013 = VERTEX_POINT('',#44845) ;
#13014 = VERTEX_POINT('',#44847) ;
#13015 = VERTEX_POINT('',#44849) ;
#13016 = VERTEX_POINT('',#44853) ;
#13017 = VERTEX_POINT('',#44854) ;
#13018 = VERTEX_POINT('',#44856) ;
#13019 = VERTEX_POINT('',#44858) ;
#13020 = VERTEX_POINT('',#44871) ;
#13021 = VERTEX_POINT('',#44872) ;
#13022 = VERTEX_POINT('',#44909) ;
#13023 = VERTEX_POINT('',#44911) ;
#13024 = VERTEX_POINT('',#44949) ;
#13025 = VERTEX_POINT('',#44951) ;
#13026 = VERTEX_POINT('',#44954) ;
#13027 = VERTEX_POINT('',#44959) ;
#13028 = VERTEX_POINT('',#44965) ;
#13029 = VERTEX_POINT('',#44966) ;
#13030 = VERTEX_POINT('',#45003) ;
#13031 = VERTEX_POINT('',#45005) ;
#13032 = VERTEX_POINT('',#45043) ;
#13033 = VERTEX_POINT('',#45045) ;
#13034 = VERTEX_POINT('',#45048) ;
#13035 = VERTEX_POINT('',#45053) ;
#13036 = VERTEX_POINT('',#45068) ;
#13037 = VERTEX_POINT('',#45070) ;
#13038 = VERTEX_POINT('',#45074) ;
#13039 = VERTEX_POINT('',#45076) ;
#13040 = VERTEX_POINT('',#45080) ;
#13041 = VERTEX_POINT('',#45082) ;
#13042 = VERTEX_POINT('',#45086) ;
#13043 = VERTEX_POINT('',#45088) ;
#13044 = VERTEX_POINT('',#45092) ;
#13045 = VERTEX_POINT('',#45093) ;
#13046 = VERTEX_POINT('',#45095) ;
#13047 = VERTEX_POINT('',#45097) ;
#13048 = VERTEX_POINT('',#45103) ;
#13049 = VERTEX_POINT('',#45105) ;
#13050 = VERTEX_POINT('',#45107) ;
#13051 = VERTEX_POINT('',#45109) ;
#13052 = VERTEX_POINT('',#45111) ;
#13053 = VERTEX_POINT('',#45113) ;
#13054 = VERTEX_POINT('',#45116) ;
#13055 = VERTEX_POINT('',#45118) ;
#13056 = VERTEX_POINT('',#45120) ;
#13057 = VERTEX_POINT('',#45122) ;
#13058 = VERTEX_POINT('',#45124) ;
#13059 = VERTEX_POINT('',#45126) ;
#13060 = VERTEX_POINT('',#45128) ;
#13061 = VERTEX_POINT('',#45130) ;
#13062 = VERTEX_POINT('',#45132) ;
#13063 = VERTEX_POINT('',#45136) ;
#13064 = VERTEX_POINT('',#45137) ;
#13065 = VERTEX_POINT('',#45144) ;
#13066 = VERTEX_POINT('',#45146) ;
#13067 = VERTEX_POINT('',#45148) ;
#13068 = VERTEX_POINT('',#45150) ;
#13069 = VERTEX_POINT('',#45152) ;
#13070 = VERTEX_POINT('',#45154) ;
#13071 = VERTEX_POINT('',#45156) ;
#13072 = VERTEX_POINT('',#45158) ;
#13073 = VERTEX_POINT('',#45160) ;
#13074 = VERTEX_POINT('',#45162) ;
#13075 = VERTEX_POINT('',#45165) ;
#13076 = VERTEX_POINT('',#45168) ;
#13077 = VERTEX_POINT('',#45169) ;
#13078 = VERTEX_POINT('',#45176) ;
#13079 = VERTEX_POINT('',#45178) ;
#13080 = VERTEX_POINT('',#45180) ;
#13081 = VERTEX_POINT('',#45182) ;
#13082 = VERTEX_POINT('',#45184) ;
#13083 = VERTEX_POINT('',#45186) ;
#13084 = VERTEX_POINT('',#45188) ;
#13085 = VERTEX_POINT('',#45190) ;
#13086 = VERTEX_POINT('',#45192) ;
#13087 = VERTEX_POINT('',#45194) ;
#13088 = VERTEX_POINT('',#45197) ;
#13089 = VERTEX_POINT('',#45199) ;
#13090 = VERTEX_POINT('',#45202) ;
#13091 = VERTEX_POINT('',#45208) ;
#13092 = VERTEX_POINT('',#45210) ;
#13093 = VERTEX_POINT('',#45215) ;
#13094 = VERTEX_POINT('',#45220) ;
#13095 = VERTEX_POINT('',#45221) ;
#13096 = VERTEX_POINT('',#45223) ;
#13097 = VERTEX_POINT('',#45225) ;
#13098 = VERTEX_POINT('',#45229) ;
#13099 = VERTEX_POINT('',#45230) ;
#13100 = VERTEX_POINT('',#45232) ;
#13101 = VERTEX_POINT('',#45234) ;
#13102 = VERTEX_POINT('',#45238) ;
#13103 = VERTEX_POINT('',#45240) ;
#13104 = VERTEX_POINT('',#45242) ;
#13105 = VERTEX_POINT('',#45244) ;
#13106 = VERTEX_POINT('',#45248) ;
#13107 = VERTEX_POINT('',#45252) ;
#13108 = VERTEX_POINT('',#45256) ;
#13109 = VERTEX_POINT('',#45258) ;
#13110 = VERTEX_POINT('',#45260) ;
#13111 = VERTEX_POINT('',#45262) ;
#13112 = VERTEX_POINT('',#45266) ;
#13113 = VERTEX_POINT('',#45270) ;
#13114 = VERTEX_POINT('',#45274) ;
#13115 = VERTEX_POINT('',#45278) ;
#13116 = VERTEX_POINT('',#45284) ;
#13117 = VERTEX_POINT('',#45288) ;
#13118 = VERTEX_POINT('',#45294) ;
#13119 = VERTEX_POINT('',#45295) ;
#13120 = VERTEX_POINT('',#45299) ;
#13121 = VERTEX_POINT('',#45305) ;
#13122 = VERTEX_POINT('',#45309) ;
#13123 = VERTEX_POINT('',#45311) ;
#13124 = VERTEX_POINT('',#45317) ;
#13125 = VERTEX_POINT('',#45319) ;
#13126 = VERTEX_POINT('',#45324) ;
#13127 = VERTEX_POINT('',#45326) ;
#13128 = VERTEX_POINT('',#45331) ;
#13129 = VERTEX_POINT('',#45333) ;
#13130 = VERTEX_POINT('',#45338) ;
#13131 = VERTEX_POINT('',#45343) ;
#13132 = VERTEX_POINT('',#45344) ;
#13133 = VERTEX_POINT('',#45349) ;
#13134 = VERTEX_POINT('',#45350) ;
#13135 = VERTEX_POINT('',#45360) ;
#13136 = VERTEX_POINT('',#45362) ;
#13137 = VERTEX_POINT('',#45366) ;
#13138 = VERTEX_POINT('',#45367) ;
#13139 = VERTEX_POINT('',#45372) ;
#13140 = VERTEX_POINT('',#45373) ;
#13141 = VERTEX_POINT('',#45382) ;
#13142 = VERTEX_POINT('',#45386) ;
#13143 = VERTEX_POINT('',#45393) ;
#13144 = VERTEX_POINT('',#45395) ;
#13145 = VERTEX_POINT('',#45399) ;
#13146 = VERTEX_POINT('',#45401) ;
#13147 = VERTEX_POINT('',#45413) ;
#13148 = VERTEX_POINT('',#45415) ;
#13149 = VERTEX_POINT('',#45420) ;
#13150 = VERTEX_POINT('',#45421) ;
#13151 = VERTEX_POINT('',#45423) ;
#13152 = VERTEX_POINT('',#45425) ;
#13153 = VERTEX_POINT('',#45429) ;
#13154 = VERTEX_POINT('',#45430) ;
#13155 = VERTEX_POINT('',#45432) ;
#13156 = VERTEX_POINT('',#45434) ;
#13157 = VERTEX_POINT('',#45438) ;
#13158 = VERTEX_POINT('',#45441) ;
#13159 = VERTEX_POINT('',#45445) ;
#13160 = VERTEX_POINT('',#45449) ;
#13161 = VERTEX_POINT('',#45459) ;
#13162 = VERTEX_POINT('',#45460) ;
#13163 = VERTEX_POINT('',#45462) ;
#13164 = VERTEX_POINT('',#45464) ;
#13165 = VERTEX_POINT('',#45466) ;
#13166 = VERTEX_POINT('',#45470) ;
#13167 = VERTEX_POINT('',#45471) ;
#13168 = VERTEX_POINT('',#45473) ;
#13169 = VERTEX_POINT('',#45475) ;
#13170 = VERTEX_POINT('',#45477) ;
#13171 = VERTEX_POINT('',#45481) ;
#13172 = VERTEX_POINT('',#45482) ;
#13173 = VERTEX_POINT('',#45484) ;
#13174 = VERTEX_POINT('',#45486) ;
#13175 = VERTEX_POINT('',#45490) ;
#13176 = VERTEX_POINT('',#45491) ;
#13177 = VERTEX_POINT('',#45493) ;
#13178 = VERTEX_POINT('',#45495) ;
#13179 = VERTEX_POINT('',#45497) ;
#13180 = VERTEX_POINT('',#45501) ;
#13181 = VERTEX_POINT('',#45502) ;
#13182 = VERTEX_POINT('',#45504) ;
#13183 = VERTEX_POINT('',#45506) ;
#13184 = VERTEX_POINT('',#45508) ;
#13185 = VERTEX_POINT('',#45512) ;
#13186 = VERTEX_POINT('',#45513) ;
#13187 = VERTEX_POINT('',#45515) ;
#13188 = VERTEX_POINT('',#45517) ;
#13189 = VERTEX_POINT('',#45521) ;
#13190 = VERTEX_POINT('',#45523) ;
#13191 = VERTEX_POINT('',#45527) ;
#13192 = VERTEX_POINT('',#45529) ;
#13193 = VERTEX_POINT('',#45533) ;
#13194 = VERTEX_POINT('',#45535) ;
#13195 = VERTEX_POINT('',#45539) ;
#13196 = VERTEX_POINT('',#45541) ;
#13197 = VERTEX_POINT('',#45545) ;
#13198 = VERTEX_POINT('',#45547) ;
#13199 = VERTEX_POINT('',#45551) ;
#13200 = VERTEX_POINT('',#45553) ;
#13201 = VERTEX_POINT('',#45557) ;
#13202 = VERTEX_POINT('',#45559) ;
#13203 = VERTEX_POINT('',#45561) ;
#13204 = VERTEX_POINT('',#45565) ;
#13205 = VERTEX_POINT('',#45567) ;
#13206 = VERTEX_POINT('',#45569) ;
#13207 = VERTEX_POINT('',#45573) ;
#13208 = VERTEX_POINT('',#45575) ;
#13209 = VERTEX_POINT('',#45577) ;
#13210 = VERTEX_POINT('',#45581) ;
#13211 = VERTEX_POINT('',#45583) ;
#13212 = VERTEX_POINT('',#45585) ;
#13213 = VERTEX_POINT('',#45589) ;
#13214 = VERTEX_POINT('',#45591) ;
#13215 = VERTEX_POINT('',#45593) ;
#13216 = VERTEX_POINT('',#45597) ;
#13217 = VERTEX_POINT('',#45599) ;
#13218 = VERTEX_POINT('',#45603) ;
#13219 = VERTEX_POINT('',#45605) ;
#13220 = VERTEX_POINT('',#45607) ;
#13221 = VERTEX_POINT('',#45609) ;
#13222 = VERTEX_POINT('',#45613) ;
#13223 = VERTEX_POINT('',#45615) ;
#13224 = VERTEX_POINT('',#45617) ;
#13225 = VERTEX_POINT('',#45619) ;
#13226 = VERTEX_POINT('',#45623) ;
#13227 = VERTEX_POINT('',#45625) ;
#13228 = VERTEX_POINT('',#45629) ;
#13229 = VERTEX_POINT('',#45632) ;
#13230 = VERTEX_POINT('',#45636) ;
#13231 = VERTEX_POINT('',#45640) ;
#13232 = VERTEX_POINT('',#45644) ;
#13233 = VERTEX_POINT('',#45646) ;
#13234 = VERTEX_POINT('',#45648) ;
#13235 = VERTEX_POINT('',#45650) ;
#13236 = VERTEX_POINT('',#45654) ;
#13237 = VERTEX_POINT('',#45656) ;
#13238 = VERTEX_POINT('',#45660) ;
#13239 = VERTEX_POINT('',#45662) ;
#13240 = VERTEX_POINT('',#45664) ;
#13241 = VERTEX_POINT('',#45666) ;
#13242 = VERTEX_POINT('',#45670) ;
#13243 = VERTEX_POINT('',#45672) ;
#13244 = VERTEX_POINT('',#45676) ;
#13245 = VERTEX_POINT('',#45678) ;
#13246 = VERTEX_POINT('',#45682) ;
#13247 = VERTEX_POINT('',#45684) ;
#13248 = VERTEX_POINT('',#45686) ;
#13249 = VERTEX_POINT('',#45688) ;
#13250 = VERTEX_POINT('',#45692) ;
#13251 = VERTEX_POINT('',#45698) ;
#13252 = VERTEX_POINT('',#45702) ;
#13253 = VERTEX_POINT('',#45708) ;
#13254 = VERTEX_POINT('',#45714) ;
#13255 = VERTEX_POINT('',#45716) ;
#13256 = VERTEX_POINT('',#45720) ;
#13257 = VERTEX_POINT('',#45724) ;
#13258 = VERTEX_POINT('',#45728) ;
#13259 = VERTEX_POINT('',#45730) ;
#13260 = VERTEX_POINT('',#45744) ;
#13261 = VERTEX_POINT('',#45747) ;
#13262 = VERTEX_POINT('',#45749) ;
#13263 = VERTEX_POINT('',#45752) ;
#13264 = VERTEX_POINT('',#45757) ;
#13265 = VERTEX_POINT('',#45761) ;
#13266 = VERTEX_POINT('',#45771) ;
#13267 = VERTEX_POINT('',#45778) ;
#13268 = VERTEX_POINT('',#45780) ;
#13269 = VERTEX_POINT('',#45785) ;
#13270 = VERTEX_POINT('',#45788) ;
#13271 = VERTEX_POINT('',#45794) ;
#13272 = VERTEX_POINT('',#45796) ;
#13273 = VERTEX_POINT('',#45800) ;
#13274 = VERTEX_POINT('',#45802) ;
#13275 = VERTEX_POINT('',#45809) ;
#13276 = VERTEX_POINT('',#45810) ;
#13277 = VERTEX_POINT('',#45812) ;
#13278 = VERTEX_POINT('',#45814) ;
#13279 = VERTEX_POINT('',#45818) ;
#13280 = VERTEX_POINT('',#45820) ;
#13281 = VERTEX_POINT('',#45822) ;
#13282 = VERTEX_POINT('',#45824) ;
#13283 = VERTEX_POINT('',#45828) ;
#13284 = VERTEX_POINT('',#45830) ;
#13285 = VERTEX_POINT('',#45834) ;
#13286 = VERTEX_POINT('',#45837) ;
#13287 = VERTEX_POINT('',#45841) ;
#13288 = VERTEX_POINT('',#45843) ;
#13289 = VERTEX_POINT('',#45845) ;
#13290 = VERTEX_POINT('',#45847) ;
#13291 = VERTEX_POINT('',#45851) ;
#13292 = VERTEX_POINT('',#45853) ;
#13293 = VERTEX_POINT('',#45857) ;
#13294 = VERTEX_POINT('',#45862) ;
#13295 = VERTEX_POINT('',#45864) ;
#13296 = VERTEX_POINT('',#45866) ;
#13297 = VERTEX_POINT('',#45870) ;
#13298 = VERTEX_POINT('',#45872) ;
#13299 = VERTEX_POINT('',#45886) ;
#13300 = VERTEX_POINT('',#45888) ;
#13301 = VERTEX_POINT('',#45895) ;
#13302 = VERTEX_POINT('',#45897) ;
#13303 = VERTEX_POINT('',#45902) ;
#13304 = VERTEX_POINT('',#45904) ;
#13305 = VERTEX_POINT('',#45908) ;
#13306 = VERTEX_POINT('',#45910) ;
#13307 = VERTEX_POINT('',#45917) ;
#13308 = VERTEX_POINT('',#45919) ;
#13309 = VERTEX_POINT('',#45923) ;
#13310 = VERTEX_POINT('',#45925) ;
#13311 = VERTEX_POINT('',#45931) ;
#13312 = VERTEX_POINT('',#45933) ;
#13313 = VERTEX_POINT('',#45937) ;
#13314 = VERTEX_POINT('',#45939) ;
#13315 = VERTEX_POINT('',#45945) ;
#13316 = VERTEX_POINT('',#45947) ;
#13317 = VERTEX_POINT('',#45954) ;
#13318 = VERTEX_POINT('',#45956) ;
#13319 = VERTEX_POINT('',#45959) ;
#13320 = VERTEX_POINT('',#45961) ;
#13321 = VERTEX_POINT('',#45966) ;
#13322 = VERTEX_POINT('',#45968) ;
#13323 = VERTEX_POINT('',#45970) ;
#13324 = VERTEX_POINT('',#45972) ;
#13325 = VERTEX_POINT('',#45974) ;
#13326 = VERTEX_POINT('',#45976) ;
#13327 = VERTEX_POINT('',#45978) ;
#13328 = VERTEX_POINT('',#45980) ;
#13329 = VERTEX_POINT('',#45982) ;
#13330 = VERTEX_POINT('',#45985) ;
#13331 = VERTEX_POINT('',#45987) ;
#13332 = VERTEX_POINT('',#45990) ;
#13333 = VERTEX_POINT('',#45992) ;
#13334 = VERTEX_POINT('',#45995) ;
#13335 = VERTEX_POINT('',#45996) ;
#13336 = VERTEX_POINT('',#45998) ;
#13337 = VERTEX_POINT('',#46000) ;
#13338 = VERTEX_POINT('',#46003) ;
#13339 = VERTEX_POINT('',#46004) ;
#13340 = VERTEX_POINT('',#46006) ;
#13341 = VERTEX_POINT('',#46008) ;
#13342 = VERTEX_POINT('',#46011) ;
#13343 = VERTEX_POINT('',#46012) ;
#13344 = VERTEX_POINT('',#46014) ;
#13345 = VERTEX_POINT('',#46016) ;
#13346 = VERTEX_POINT('',#46019) ;
#13347 = VERTEX_POINT('',#46020) ;
#13348 = VERTEX_POINT('',#46022) ;
#13349 = VERTEX_POINT('',#46024) ;
#13350 = VERTEX_POINT('',#46027) ;
#13351 = VERTEX_POINT('',#46028) ;
#13352 = VERTEX_POINT('',#46030) ;
#13353 = VERTEX_POINT('',#46032) ;
#13354 = VERTEX_POINT('',#46035) ;
#13355 = VERTEX_POINT('',#46036) ;
#13356 = VERTEX_POINT('',#46038) ;
#13357 = VERTEX_POINT('',#46040) ;
#13358 = VERTEX_POINT('',#46044) ;
#13359 = VERTEX_POINT('',#46046) ;
#13360 = VERTEX_POINT('',#46050) ;
#13361 = VERTEX_POINT('',#46054) ;
#13362 = VERTEX_POINT('',#46058) ;
#13363 = VERTEX_POINT('',#46060) ;
#13364 = VERTEX_POINT('',#46066) ;
#13365 = VERTEX_POINT('',#46070) ;
#13366 = VERTEX_POINT('',#46078) ;
#13367 = VERTEX_POINT('',#46080) ;
#13368 = VERTEX_POINT('',#46084) ;
#13369 = VERTEX_POINT('',#46088) ;
#13370 = VERTEX_POINT('',#46092) ;
#13371 = VERTEX_POINT('',#46094) ;
#13372 = VERTEX_POINT('',#46100) ;
#13373 = VERTEX_POINT('',#46104) ;
#13374 = VERTEX_POINT('',#46112) ;
#13375 = VERTEX_POINT('',#46114) ;
#13376 = VERTEX_POINT('',#46118) ;
#13377 = VERTEX_POINT('',#46122) ;
#13378 = VERTEX_POINT('',#46126) ;
#13379 = VERTEX_POINT('',#46128) ;
#13380 = VERTEX_POINT('',#46134) ;
#13381 = VERTEX_POINT('',#46138) ;
#13382 = VERTEX_POINT('',#46146) ;
#13383 = VERTEX_POINT('',#46148) ;
#13384 = VERTEX_POINT('',#46152) ;
#13385 = VERTEX_POINT('',#46156) ;
#13386 = VERTEX_POINT('',#46160) ;
#13387 = VERTEX_POINT('',#46162) ;
#13388 = VERTEX_POINT('',#46168) ;
#13389 = VERTEX_POINT('',#46172) ;
#13390 = VERTEX_POINT('',#46180) ;
#13391 = VERTEX_POINT('',#46187) ;
#13392 = VERTEX_POINT('',#46189) ;
#13393 = VERTEX_POINT('',#46193) ;
#13394 = VERTEX_POINT('',#46195) ;
#13395 = VERTEX_POINT('',#46213) ;
#13396 = VERTEX_POINT('',#46215) ;
#13397 = VERTEX_POINT('',#46219) ;
#13398 = VERTEX_POINT('',#46220) ;
#13399 = VERTEX_POINT('',#46222) ;
#13400 = VERTEX_POINT('',#46224) ;
#13401 = VERTEX_POINT('',#46228) ;
#13402 = VERTEX_POINT('',#46230) ;
#13403 = VERTEX_POINT('',#46234) ;
#13404 = VERTEX_POINT('',#46235) ;
#13405 = VERTEX_POINT('',#46237) ;
#13406 = VERTEX_POINT('',#46242) ;
#13407 = VERTEX_POINT('',#46243) ;
#13408 = VERTEX_POINT('',#46250) ;
#13409 = VERTEX_POINT('',#46256) ;
#13410 = VERTEX_POINT('',#46258) ;
#13411 = VERTEX_POINT('',#46262) ;
#13412 = VERTEX_POINT('',#46263) ;
#13413 = VERTEX_POINT('',#46265) ;
#13414 = VERTEX_POINT('',#46267) ;
#13415 = VERTEX_POINT('',#46271) ;
#13416 = VERTEX_POINT('',#46273) ;
#13417 = VERTEX_POINT('',#46277) ;
#13418 = VERTEX_POINT('',#46281) ;
#13419 = VERTEX_POINT('',#46287) ;
#13420 = VERTEX_POINT('',#46289) ;
#13421 = VERTEX_POINT('',#46293) ;
#13422 = VERTEX_POINT('',#46295) ;
#13423 = VERTEX_POINT('',#46299) ;
#13424 = VERTEX_POINT('',#46301) ;
#13425 = VERTEX_POINT('',#46305) ;
#13426 = VERTEX_POINT('',#46307) ;
#13427 = VERTEX_POINT('',#46311) ;
#13428 = VERTEX_POINT('',#46313) ;
#13429 = VERTEX_POINT('',#46315) ;
#13430 = VERTEX_POINT('',#46317) ;
#13431 = VERTEX_POINT('',#46319) ;
#13432 = VERTEX_POINT('',#46321) ;
#13433 = VERTEX_POINT('',#46325) ;
#13434 = VERTEX_POINT('',#46327) ;
#13435 = VERTEX_POINT('',#46329) ;
#13436 = VERTEX_POINT('',#46331) ;
#13437 = VERTEX_POINT('',#46333) ;
#13438 = VERTEX_POINT('',#46335) ;
#13439 = VERTEX_POINT('',#46337) ;
#13440 = VERTEX_POINT('',#46339) ;
#13441 = VERTEX_POINT('',#46341) ;
#13442 = VERTEX_POINT('',#46343) ;
#13443 = VERTEX_POINT('',#46345) ;
#13444 = VERTEX_POINT('',#46347) ;
#13445 = VERTEX_POINT('',#46349) ;
#13446 = VERTEX_POINT('',#46351) ;
#13447 = VERTEX_POINT('',#46353) ;
#13448 = VERTEX_POINT('',#46355) ;
#13449 = VERTEX_POINT('',#46359) ;
#13450 = VERTEX_POINT('',#46363) ;
#13451 = VERTEX_POINT('',#46364) ;
#13452 = VERTEX_POINT('',#46366) ;
#13453 = VERTEX_POINT('',#46368) ;
#13454 = VERTEX_POINT('',#46370) ;
#13455 = VERTEX_POINT('',#46372) ;
#13456 = VERTEX_POINT('',#46386) ;
#13457 = VERTEX_POINT('',#46388) ;
#13458 = VERTEX_POINT('',#46390) ;
#13459 = VERTEX_POINT('',#46400) ;
#13460 = VERTEX_POINT('',#46402) ;
#13461 = VERTEX_POINT('',#46406) ;
#13462 = VERTEX_POINT('',#46407) ;
#13463 = VERTEX_POINT('',#46409) ;
#13464 = VERTEX_POINT('',#46411) ;
#13465 = VERTEX_POINT('',#46426) ;
#13466 = VERTEX_POINT('',#46427) ;
#13467 = VERTEX_POINT('',#46429) ;
#13468 = VERTEX_POINT('',#46431) ;
#13469 = VERTEX_POINT('',#46435) ;
#13470 = VERTEX_POINT('',#46437) ;
#13471 = VERTEX_POINT('',#46441) ;
#13472 = VERTEX_POINT('',#46442) ;
#13473 = VERTEX_POINT('',#46444) ;
#13474 = VERTEX_POINT('',#46449) ;
#13475 = VERTEX_POINT('',#46450) ;
#13476 = VERTEX_POINT('',#46453) ;
#13477 = VERTEX_POINT('',#46457) ;
#13478 = VERTEX_POINT('',#46462) ;
#13479 = VERTEX_POINT('',#46467) ;
#13480 = VERTEX_POINT('',#46469) ;
#13481 = VERTEX_POINT('',#46473) ;
#13482 = VERTEX_POINT('',#46474) ;
#13483 = VERTEX_POINT('',#46476) ;
#13484 = VERTEX_POINT('',#46478) ;
#13485 = VERTEX_POINT('',#46482) ;
#13486 = VERTEX_POINT('',#46483) ;
#13487 = VERTEX_POINT('',#46485) ;
#13488 = VERTEX_POINT('',#46487) ;
#13489 = VERTEX_POINT('',#46494) ;
#13490 = VERTEX_POINT('',#46496) ;
#13491 = VERTEX_POINT('',#46500) ;
#13492 = VERTEX_POINT('',#46505) ;
#13493 = VERTEX_POINT('',#46507) ;
#13494 = VERTEX_POINT('',#46511) ;
#13495 = VERTEX_POINT('',#46512) ;
#13496 = VERTEX_POINT('',#46514) ;
#13497 = VERTEX_POINT('',#46516) ;
#13498 = VERTEX_POINT('',#46520) ;
#13499 = VERTEX_POINT('',#46521) ;
#13500 = VERTEX_POINT('',#46526) ;
#13501 = VERTEX_POINT('',#46527) ;
#13502 = VERTEX_POINT('',#46532) ;
#13503 = VERTEX_POINT('',#46534) ;
#13504 = VERTEX_POINT('',#46538) ;
#13505 = VERTEX_POINT('',#46540) ;
#13506 = VERTEX_POINT('',#46544) ;
#13507 = VERTEX_POINT('',#46546) ;
#13508 = VERTEX_POINT('',#46559) ;
#13509 = VERTEX_POINT('',#46560) ;
#13510 = VERTEX_POINT('',#46562) ;
#13511 = VERTEX_POINT('',#46564) ;
#13512 = VERTEX_POINT('',#46568) ;
#13513 = VERTEX_POINT('',#46570) ;
#13514 = VERTEX_POINT('',#46574) ;
#13515 = VERTEX_POINT('',#46578) ;
#13516 = VERTEX_POINT('',#46582) ;
#13517 = VERTEX_POINT('',#46584) ;
#13518 = VERTEX_POINT('',#46586) ;
#13519 = VERTEX_POINT('',#46588) ;
#13520 = VERTEX_POINT('',#46590) ;
#13521 = VERTEX_POINT('',#46592) ;
#13522 = VERTEX_POINT('',#46594) ;
#13523 = VERTEX_POINT('',#46596) ;
#13524 = VERTEX_POINT('',#46598) ;
#13525 = VERTEX_POINT('',#46600) ;
#13526 = VERTEX_POINT('',#46602) ;
#13527 = VERTEX_POINT('',#46604) ;
#13528 = VERTEX_POINT('',#46606) ;
#13529 = VERTEX_POINT('',#46608) ;
#13530 = VERTEX_POINT('',#46610) ;
#13531 = VERTEX_POINT('',#46612) ;
#13532 = VERTEX_POINT('',#46614) ;
#13533 = VERTEX_POINT('',#46616) ;
#13534 = VERTEX_POINT('',#46618) ;
#13535 = VERTEX_POINT('',#46620) ;
#13536 = VERTEX_POINT('',#46622) ;
#13537 = VERTEX_POINT('',#46624) ;
#13538 = VERTEX_POINT('',#46626) ;
#13539 = VERTEX_POINT('',#46628) ;
#13540 = VERTEX_POINT('',#46630) ;
#13541 = VERTEX_POINT('',#46632) ;
#13542 = VERTEX_POINT('',#46634) ;
#13543 = VERTEX_POINT('',#46636) ;
#13544 = VERTEX_POINT('',#46638) ;
#13545 = VERTEX_POINT('',#46640) ;
#13546 = VERTEX_POINT('',#46642) ;
#13547 = VERTEX_POINT('',#46644) ;
#13548 = VERTEX_POINT('',#46646) ;
#13549 = VERTEX_POINT('',#46648) ;
#13550 = VERTEX_POINT('',#46650) ;
#13551 = VERTEX_POINT('',#46652) ;
#13552 = VERTEX_POINT('',#46656) ;
#13553 = VERTEX_POINT('',#46657) ;
#13554 = VERTEX_POINT('',#46659) ;
#13555 = VERTEX_POINT('',#46661) ;
#13556 = VERTEX_POINT('',#46672) ;
#13557 = VERTEX_POINT('',#46674) ;
#13558 = VERTEX_POINT('',#46677) ;
#13559 = VERTEX_POINT('',#46679) ;
#13560 = VERTEX_POINT('',#46682) ;
#13561 = VERTEX_POINT('',#46684) ;
#13562 = VERTEX_POINT('',#46687) ;
#13563 = VERTEX_POINT('',#46689) ;
#13564 = VERTEX_POINT('',#46692) ;
#13565 = VERTEX_POINT('',#46694) ;
#13566 = VERTEX_POINT('',#46697) ;
#13567 = VERTEX_POINT('',#46699) ;
#13568 = VERTEX_POINT('',#46702) ;
#13569 = VERTEX_POINT('',#46704) ;
#13570 = VERTEX_POINT('',#46707) ;
#13571 = VERTEX_POINT('',#46709) ;
#13572 = VERTEX_POINT('',#46713) ;
#13573 = VERTEX_POINT('',#46715) ;
#13574 = VERTEX_POINT('',#46724) ;
#13575 = VERTEX_POINT('',#46726) ;
#13576 = VERTEX_POINT('',#46735) ;
#13577 = VERTEX_POINT('',#46737) ;
#13578 = VERTEX_POINT('',#46746) ;
#13579 = VERTEX_POINT('',#46748) ;
#13580 = VERTEX_POINT('',#46757) ;
#13581 = VERTEX_POINT('',#46759) ;
#13582 = VERTEX_POINT('',#46768) ;
#13583 = VERTEX_POINT('',#46770) ;
#13584 = VERTEX_POINT('',#46779) ;
#13585 = VERTEX_POINT('',#46781) ;
#13586 = VERTEX_POINT('',#46790) ;
#13587 = VERTEX_POINT('',#46792) ;
#13588 = VERTEX_POINT('',#46802) ;
#13589 = VERTEX_POINT('',#46804) ;
#13590 = VERTEX_POINT('',#46808) ;
#13591 = VERTEX_POINT('',#46810) ;
#13592 = VERTEX_POINT('',#46814) ;
#13593 = VERTEX_POINT('',#46816) ;
#13594 = VERTEX_POINT('',#46820) ;
#13595 = VERTEX_POINT('',#46822) ;
#13596 = VERTEX_POINT('',#46826) ;
#13597 = VERTEX_POINT('',#46827) ;
#13598 = VERTEX_POINT('',#46829) ;
#13599 = VERTEX_POINT('',#46831) ;
#13600 = VERTEX_POINT('',#46880) ;
#13601 = VERTEX_POINT('',#46881) ;
#13602 = VERTEX_POINT('',#46927) ;
#13603 = VERTEX_POINT('',#46928) ;
#13604 = VERTEX_POINT('',#46930) ;
#13605 = VERTEX_POINT('',#46932) ;
#13606 = VERTEX_POINT('',#46937) ;
#13607 = VERTEX_POINT('',#46941) ;
#13608 = VERTEX_POINT('',#46943) ;
#13609 = VERTEX_POINT('',#46948) ;
#13610 = VERTEX_POINT('',#46949) ;
#13611 = VERTEX_POINT('',#46951) ;
#13612 = VERTEX_POINT('',#46953) ;
#13613 = VERTEX_POINT('',#46965) ;
#13614 = VERTEX_POINT('',#46971) ;
#13615 = VERTEX_POINT('',#46973) ;
#13616 = VERTEX_POINT('',#46977) ;
#13617 = VERTEX_POINT('',#46981) ;
#13618 = VERTEX_POINT('',#46983) ;
#13619 = VERTEX_POINT('',#46989) ;
#13620 = VERTEX_POINT('',#46991) ;
#13621 = VERTEX_POINT('',#46994) ;
#13622 = VERTEX_POINT('',#46996) ;
#13623 = VERTEX_POINT('',#47004) ;
#13624 = VERTEX_POINT('',#47006) ;
#13625 = VERTEX_POINT('',#47010) ;
#13626 = VERTEX_POINT('',#47012) ;
#13627 = VERTEX_POINT('',#47016) ;
#13628 = VERTEX_POINT('',#47018) ;
#13629 = VERTEX_POINT('',#47022) ;
#13630 = VERTEX_POINT('',#47024) ;
#13631 = VERTEX_POINT('',#47028) ;
#13632 = VERTEX_POINT('',#47030) ;
#13633 = VERTEX_POINT('',#47034) ;
#13634 = VERTEX_POINT('',#47036) ;
#13635 = VERTEX_POINT('',#47040) ;
#13636 = VERTEX_POINT('',#47042) ;
#13637 = VERTEX_POINT('',#47046) ;
#13638 = VERTEX_POINT('',#47048) ;
#13639 = VERTEX_POINT('',#47052) ;
#13640 = VERTEX_POINT('',#47053) ;
#13641 = VERTEX_POINT('',#47055) ;
#13642 = VERTEX_POINT('',#47057) ;
#13643 = VERTEX_POINT('',#47067) ;
#13644 = VERTEX_POINT('',#47068) ;
#13645 = VERTEX_POINT('',#47071) ;
#13646 = VERTEX_POINT('',#47076) ;
#13647 = VERTEX_POINT('',#47078) ;
#13648 = VERTEX_POINT('',#47082) ;
#13649 = VERTEX_POINT('',#47084) ;
#13650 = VERTEX_POINT('',#47088) ;
#13651 = VERTEX_POINT('',#47090) ;
#13652 = VERTEX_POINT('',#47094) ;
#13653 = VERTEX_POINT('',#47098) ;
#13654 = VERTEX_POINT('',#47102) ;
#13655 = VERTEX_POINT('',#47104) ;
#13656 = VERTEX_POINT('',#47108) ;
#13657 = VERTEX_POINT('',#47109) ;
#13658 = VERTEX_POINT('',#47111) ;
#13659 = VERTEX_POINT('',#47113) ;
#13660 = VERTEX_POINT('',#47116) ;
#13661 = VERTEX_POINT('',#47117) ;
#13662 = VERTEX_POINT('',#47119) ;
#13663 = VERTEX_POINT('',#47121) ;
#13664 = VERTEX_POINT('',#47125) ;
#13665 = VERTEX_POINT('',#47126) ;
#13666 = VERTEX_POINT('',#47128) ;
#13667 = VERTEX_POINT('',#47130) ;
#13668 = VERTEX_POINT('',#47133) ;
#13669 = VERTEX_POINT('',#47135) ;
#13670 = VERTEX_POINT('',#47147) ;
#13671 = VERTEX_POINT('',#47151) ;
#13672 = VERTEX_POINT('',#47158) ;
#13673 = VERTEX_POINT('',#47160) ;
#13674 = VERTEX_POINT('',#47164) ;
#13675 = VERTEX_POINT('',#47168) ;
#13676 = VERTEX_POINT('',#47176) ;
#13677 = VERTEX_POINT('',#47178) ;
#13678 = VERTEX_POINT('',#47183) ;
#13679 = VERTEX_POINT('',#47187) ;
#13680 = VERTEX_POINT('',#47189) ;
#13681 = VERTEX_POINT('',#47192) ;
#13682 = VERTEX_POINT('',#47197) ;
#13683 = VERTEX_POINT('',#47203) ;
#13684 = VERTEX_POINT('',#47204) ;
#13685 = VERTEX_POINT('',#47207) ;
#13686 = VERTEX_POINT('',#47208) ;
#13687 = VERTEX_POINT('',#47211) ;
#13688 = VERTEX_POINT('',#47212) ;
#13689 = VERTEX_POINT('',#47215) ;
#13690 = VERTEX_POINT('',#47218) ;
#13691 = VERTEX_POINT('',#47223) ;
#13692 = VERTEX_POINT('',#47224) ;
#13693 = VERTEX_POINT('',#47228) ;
#13694 = VERTEX_POINT('',#47229) ;
#13695 = VERTEX_POINT('',#47231) ;
#13696 = VERTEX_POINT('',#47233) ;
#13697 = VERTEX_POINT('',#47237) ;
#13698 = VERTEX_POINT('',#47238) ;
#13699 = VERTEX_POINT('',#47242) ;
#13700 = VERTEX_POINT('',#47243) ;
#13701 = VERTEX_POINT('',#47245) ;
#13702 = VERTEX_POINT('',#47249) ;
#13703 = VERTEX_POINT('',#47251) ;
#13704 = VERTEX_POINT('',#47274) ;
#13705 = VERTEX_POINT('',#47276) ;
#13706 = VERTEX_POINT('',#47280) ;
#13707 = VERTEX_POINT('',#47282) ;
#13708 = VERTEX_POINT('',#47284) ;
#13709 = VERTEX_POINT('',#47286) ;
#13710 = VERTEX_POINT('',#47291) ;
#13711 = VERTEX_POINT('',#47293) ;
#13712 = VERTEX_POINT('',#47302) ;
#13713 = VERTEX_POINT('',#47304) ;
#13714 = VERTEX_POINT('',#47310) ;
#13715 = VERTEX_POINT('',#47315) ;
#13716 = VERTEX_POINT('',#47323) ;
#13717 = VERTEX_POINT('',#47326) ;
#13718 = VERTEX_POINT('',#47327) ;
#13719 = VERTEX_POINT('',#47329) ;
#13720 = VERTEX_POINT('',#47354) ;
#13721 = VERTEX_POINT('',#47355) ;
#13722 = VERTEX_POINT('',#47358) ;
#13723 = VERTEX_POINT('',#47359) ;
#13724 = VERTEX_POINT('',#47361) ;
#13725 = VERTEX_POINT('',#47380) ;
#13726 = VERTEX_POINT('',#47381) ;
#13727 = VERTEX_POINT('',#47402) ;
#13728 = VERTEX_POINT('',#47408) ;
#13729 = VERTEX_POINT('',#47409) ;
#13730 = VERTEX_POINT('',#47411) ;
#13731 = VERTEX_POINT('',#47414) ;
#13732 = VERTEX_POINT('',#47417) ;
#13733 = VERTEX_POINT('',#47418) ;
#13734 = VERTEX_POINT('',#47439) ;
#13735 = VERTEX_POINT('',#47460) ;
#13736 = VERTEX_POINT('',#47461) ;
#13737 = VERTEX_POINT('',#47465) ;
#13738 = VERTEX_POINT('',#47466) ;
#13739 = VERTEX_POINT('',#47468) ;
#13740 = VERTEX_POINT('',#47470) ;
#13741 = VERTEX_POINT('',#47473) ;
#13742 = VERTEX_POINT('',#47475) ;
#13743 = VERTEX_POINT('',#47480) ;
#13744 = VERTEX_POINT('',#47482) ;
#13745 = VERTEX_POINT('',#47486) ;
#13746 = VERTEX_POINT('',#47490) ;
#13747 = VERTEX_POINT('',#47495) ;
#13748 = VERTEX_POINT('',#47497) ;
#13749 = VERTEX_POINT('',#47504) ;
#13750 = VERTEX_POINT('',#47506) ;
#13751 = VERTEX_POINT('',#47513) ;
#13752 = VERTEX_POINT('',#47515) ;
#13753 = VERTEX_POINT('',#47522) ;
#13754 = VERTEX_POINT('',#47524) ;
#13755 = VERTEX_POINT('',#47527) ;
#13756 = VERTEX_POINT('',#47528) ;
#13757 = VERTEX_POINT('',#47566) ;
#13758 = VERTEX_POINT('',#47568) ;
#13759 = VERTEX_POINT('',#47574) ;
#13760 = VERTEX_POINT('',#47579) ;
#13761 = VERTEX_POINT('',#47581) ;
#13762 = VERTEX_POINT('',#47585) ;
#13763 = VERTEX_POINT('',#47587) ;
#13764 = VERTEX_POINT('',#47593) ;
#13765 = VERTEX_POINT('',#47594) ;
#13766 = VERTEX_POINT('',#47596) ;
#13767 = VERTEX_POINT('',#47607) ;
#13768 = VERTEX_POINT('',#47618) ;
#13769 = VERTEX_POINT('',#47626) ;
#13770 = VERTEX_POINT('',#47630) ;
#13771 = VERTEX_POINT('',#47632) ;
#13772 = VERTEX_POINT('',#47636) ;
#13773 = VERTEX_POINT('',#47638) ;
#13774 = VERTEX_POINT('',#47640) ;
#13775 = VERTEX_POINT('',#47642) ;
#13776 = VERTEX_POINT('',#47644) ;
#13777 = VERTEX_POINT('',#47651) ;
#13778 = VERTEX_POINT('',#47655) ;
#13779 = VERTEX_POINT('',#47657) ;
#13780 = VERTEX_POINT('',#47661) ;
#13781 = VERTEX_POINT('',#47662) ;
#13782 = VERTEX_POINT('',#47664) ;
#13783 = VERTEX_POINT('',#47668) ;
#13784 = VERTEX_POINT('',#47669) ;
#13785 = VERTEX_POINT('',#47671) ;
#13786 = VERTEX_POINT('',#47673) ;
#13787 = VERTEX_POINT('',#47675) ;
#13788 = VERTEX_POINT('',#47679) ;
#13789 = VERTEX_POINT('',#47680) ;
#13790 = VERTEX_POINT('',#47682) ;
#13791 = VERTEX_POINT('',#47686) ;
#13792 = VERTEX_POINT('',#47687) ;
#13793 = VERTEX_POINT('',#47689) ;
#13794 = VERTEX_POINT('',#47693) ;
#13795 = VERTEX_POINT('',#47694) ;
#13796 = VERTEX_POINT('',#47696) ;
#13797 = VERTEX_POINT('',#47700) ;
#13798 = VERTEX_POINT('',#47701) ;
#13799 = VERTEX_POINT('',#47703) ;
#13800 = VERTEX_POINT('',#47705) ;
#13801 = VERTEX_POINT('',#47707) ;
#13802 = VERTEX_POINT('',#47711) ;
#13803 = VERTEX_POINT('',#47712) ;
#13804 = VERTEX_POINT('',#47714) ;
#13805 = VERTEX_POINT('',#47718) ;
#13806 = VERTEX_POINT('',#47719) ;
#13807 = VERTEX_POINT('',#47721) ;
#13808 = VERTEX_POINT('',#47725) ;
#13809 = VERTEX_POINT('',#47726) ;
#13810 = VERTEX_POINT('',#47728) ;
#13811 = VERTEX_POINT('',#47732) ;
#13812 = VERTEX_POINT('',#47733) ;
#13813 = VERTEX_POINT('',#47735) ;
#13814 = VERTEX_POINT('',#47737) ;
#13815 = VERTEX_POINT('',#47739) ;
#13816 = VERTEX_POINT('',#47743) ;
#13817 = VERTEX_POINT('',#47744) ;
#13818 = VERTEX_POINT('',#47746) ;
#13819 = VERTEX_POINT('',#47750) ;
#13820 = VERTEX_POINT('',#47751) ;
#13821 = VERTEX_POINT('',#47753) ;
#13822 = VERTEX_POINT('',#47757) ;
#13823 = VERTEX_POINT('',#47758) ;
#13824 = VERTEX_POINT('',#47760) ;
#13825 = VERTEX_POINT('',#47764) ;
#13826 = VERTEX_POINT('',#47765) ;
#13827 = VERTEX_POINT('',#47767) ;
#13828 = VERTEX_POINT('',#47769) ;
#13829 = VERTEX_POINT('',#47771) ;
#13830 = VERTEX_POINT('',#47775) ;
#13831 = VERTEX_POINT('',#47776) ;
#13832 = VERTEX_POINT('',#47778) ;
#13833 = VERTEX_POINT('',#47782) ;
#13834 = VERTEX_POINT('',#47783) ;
#13835 = VERTEX_POINT('',#47785) ;
#13836 = VERTEX_POINT('',#47789) ;
#13837 = VERTEX_POINT('',#47790) ;
#13838 = VERTEX_POINT('',#47792) ;
#13839 = VERTEX_POINT('',#47796) ;
#13840 = VERTEX_POINT('',#47797) ;
#13841 = VERTEX_POINT('',#47799) ;
#13842 = VERTEX_POINT('',#47801) ;
#13843 = VERTEX_POINT('',#47803) ;
#13844 = VERTEX_POINT('',#47807) ;
#13845 = VERTEX_POINT('',#47808) ;
#13846 = VERTEX_POINT('',#47810) ;
#13847 = VERTEX_POINT('',#47814) ;
#13848 = VERTEX_POINT('',#47815) ;
#13849 = VERTEX_POINT('',#47817) ;
#13850 = VERTEX_POINT('',#47821) ;
#13851 = VERTEX_POINT('',#47822) ;
#13852 = VERTEX_POINT('',#47824) ;
#13853 = VERTEX_POINT('',#47828) ;
#13854 = VERTEX_POINT('',#47829) ;
#13855 = VERTEX_POINT('',#47831) ;
#13856 = VERTEX_POINT('',#47833) ;
#13857 = VERTEX_POINT('',#47835) ;
#13858 = VERTEX_POINT('',#47839) ;
#13859 = VERTEX_POINT('',#47840) ;
#13860 = VERTEX_POINT('',#47842) ;
#13861 = VERTEX_POINT('',#47846) ;
#13862 = VERTEX_POINT('',#47847) ;
#13863 = VERTEX_POINT('',#47849) ;
#13864 = VERTEX_POINT('',#47853) ;
#13865 = VERTEX_POINT('',#47854) ;
#13866 = VERTEX_POINT('',#47856) ;
#13867 = VERTEX_POINT('',#47860) ;
#13868 = VERTEX_POINT('',#47861) ;
#13869 = VERTEX_POINT('',#47863) ;
#13870 = VERTEX_POINT('',#47865) ;
#13871 = VERTEX_POINT('',#47867) ;
#13872 = VERTEX_POINT('',#47871) ;
#13873 = VERTEX_POINT('',#47872) ;
#13874 = VERTEX_POINT('',#47874) ;
#13875 = VERTEX_POINT('',#47878) ;
#13876 = VERTEX_POINT('',#47879) ;
#13877 = VERTEX_POINT('',#47881) ;
#13878 = VERTEX_POINT('',#47885) ;
#13879 = VERTEX_POINT('',#47886) ;
#13880 = VERTEX_POINT('',#47888) ;
#13881 = VERTEX_POINT('',#47892) ;
#13882 = VERTEX_POINT('',#47893) ;
#13883 = VERTEX_POINT('',#47895) ;
#13884 = VERTEX_POINT('',#47897) ;
#13885 = VERTEX_POINT('',#47899) ;
#13886 = VERTEX_POINT('',#47903) ;
#13887 = VERTEX_POINT('',#47904) ;
#13888 = VERTEX_POINT('',#47906) ;
#13889 = VERTEX_POINT('',#47910) ;
#13890 = VERTEX_POINT('',#47911) ;
#13891 = VERTEX_POINT('',#47913) ;
#13892 = VERTEX_POINT('',#47917) ;
#13893 = VERTEX_POINT('',#47918) ;
#13894 = VERTEX_POINT('',#47920) ;
#13895 = VERTEX_POINT('',#47924) ;
#13896 = VERTEX_POINT('',#47925) ;
#13897 = VERTEX_POINT('',#47927) ;
#13898 = VERTEX_POINT('',#47929) ;
#13899 = VERTEX_POINT('',#47931) ;
#13900 = VERTEX_POINT('',#47935) ;
#13901 = VERTEX_POINT('',#47936) ;
#13902 = VERTEX_POINT('',#47938) ;
#13903 = VERTEX_POINT('',#47942) ;
#13904 = VERTEX_POINT('',#47943) ;
#13905 = VERTEX_POINT('',#47945) ;
#13906 = VERTEX_POINT('',#47949) ;
#13907 = VERTEX_POINT('',#47950) ;
#13908 = VERTEX_POINT('',#47952) ;
#13909 = VERTEX_POINT('',#47956) ;
#13910 = VERTEX_POINT('',#47957) ;
#13911 = VERTEX_POINT('',#47959) ;
#13912 = VERTEX_POINT('',#47961) ;
#13913 = VERTEX_POINT('',#47963) ;
#13914 = VERTEX_POINT('',#47967) ;
#13915 = VERTEX_POINT('',#47968) ;
#13916 = VERTEX_POINT('',#47970) ;
#13917 = VERTEX_POINT('',#47974) ;
#13918 = VERTEX_POINT('',#47975) ;
#13919 = VERTEX_POINT('',#47977) ;
#13920 = VERTEX_POINT('',#47981) ;
#13921 = VERTEX_POINT('',#47982) ;
#13922 = VERTEX_POINT('',#47984) ;
#13923 = VERTEX_POINT('',#47988) ;
#13924 = VERTEX_POINT('',#47989) ;
#13925 = VERTEX_POINT('',#47991) ;
#13926 = VERTEX_POINT('',#47993) ;
#13927 = VERTEX_POINT('',#47995) ;
#13928 = VERTEX_POINT('',#47999) ;
#13929 = VERTEX_POINT('',#48000) ;
#13930 = VERTEX_POINT('',#48002) ;
#13931 = VERTEX_POINT('',#48006) ;
#13932 = VERTEX_POINT('',#48007) ;
#13933 = VERTEX_POINT('',#48009) ;
#13934 = VERTEX_POINT('',#48013) ;
#13935 = VERTEX_POINT('',#48014) ;
#13936 = VERTEX_POINT('',#48016) ;
#13937 = VERTEX_POINT('',#48020) ;
#13938 = VERTEX_POINT('',#48021) ;
#13939 = VERTEX_POINT('',#48023) ;
#13940 = VERTEX_POINT('',#48025) ;
#13941 = VERTEX_POINT('',#48027) ;
#13942 = VERTEX_POINT('',#48031) ;
#13943 = VERTEX_POINT('',#48032) ;
#13944 = VERTEX_POINT('',#48034) ;
#13945 = VERTEX_POINT('',#48038) ;
#13946 = VERTEX_POINT('',#48039) ;
#13947 = VERTEX_POINT('',#48041) ;
#13948 = VERTEX_POINT('',#48045) ;
#13949 = VERTEX_POINT('',#48046) ;
#13950 = VERTEX_POINT('',#48048) ;
#13951 = VERTEX_POINT('',#48052) ;
#13952 = VERTEX_POINT('',#48053) ;
#13953 = VERTEX_POINT('',#48055) ;
#13954 = VERTEX_POINT('',#48057) ;
#13955 = VERTEX_POINT('',#48059) ;
#13956 = VERTEX_POINT('',#48063) ;
#13957 = VERTEX_POINT('',#48064) ;
#13958 = VERTEX_POINT('',#48066) ;
#13959 = VERTEX_POINT('',#48070) ;
#13960 = VERTEX_POINT('',#48071) ;
#13961 = VERTEX_POINT('',#48073) ;
#13962 = VERTEX_POINT('',#48077) ;
#13963 = VERTEX_POINT('',#48078) ;
#13964 = VERTEX_POINT('',#48080) ;
#13965 = VERTEX_POINT('',#48084) ;
#13966 = VERTEX_POINT('',#48085) ;
#13967 = VERTEX_POINT('',#48087) ;
#13968 = VERTEX_POINT('',#48089) ;
#13969 = VERTEX_POINT('',#48091) ;
#13970 = VERTEX_POINT('',#48095) ;
#13971 = VERTEX_POINT('',#48096) ;
#13972 = VERTEX_POINT('',#48098) ;
#13973 = VERTEX_POINT('',#48102) ;
#13974 = VERTEX_POINT('',#48103) ;
#13975 = VERTEX_POINT('',#48105) ;
#13976 = VERTEX_POINT('',#48109) ;
#13977 = VERTEX_POINT('',#48110) ;
#13978 = VERTEX_POINT('',#48112) ;
#13979 = VERTEX_POINT('',#48116) ;
#13980 = VERTEX_POINT('',#48117) ;
#13981 = VERTEX_POINT('',#48119) ;
#13982 = VERTEX_POINT('',#48121) ;
#13983 = VERTEX_POINT('',#48123) ;
#13984 = VERTEX_POINT('',#48127) ;
#13985 = VERTEX_POINT('',#48128) ;
#13986 = VERTEX_POINT('',#48130) ;
#13987 = VERTEX_POINT('',#48134) ;
#13988 = VERTEX_POINT('',#48135) ;
#13989 = VERTEX_POINT('',#48137) ;
#13990 = VERTEX_POINT('',#48141) ;
#13991 = VERTEX_POINT('',#48142) ;
#13992 = VERTEX_POINT('',#48144) ;
#13993 = VERTEX_POINT('',#48148) ;
#13994 = VERTEX_POINT('',#48149) ;
#13995 = VERTEX_POINT('',#48151) ;
#13996 = VERTEX_POINT('',#48153) ;
#13997 = VERTEX_POINT('',#48155) ;
#13998 = VERTEX_POINT('',#48159) ;
#13999 = VERTEX_POINT('',#48160) ;
#14000 = VERTEX_POINT('',#48162) ;
#14001 = VERTEX_POINT('',#48166) ;
#14002 = VERTEX_POINT('',#48167) ;
#14003 = VERTEX_POINT('',#48169) ;
#14004 = VERTEX_POINT('',#48173) ;
#14005 = VERTEX_POINT('',#48174) ;
#14006 = VERTEX_POINT('',#48176) ;
#14007 = VERTEX_POINT('',#48180) ;
#14008 = VERTEX_POINT('',#48181) ;
#14009 = VERTEX_POINT('',#48183) ;
#14010 = VERTEX_POINT('',#48185) ;
#14011 = VERTEX_POINT('',#48187) ;
#14012 = VERTEX_POINT('',#48191) ;
#14013 = VERTEX_POINT('',#48192) ;
#14014 = VERTEX_POINT('',#48194) ;
#14015 = VERTEX_POINT('',#48198) ;
#14016 = VERTEX_POINT('',#48199) ;
#14017 = VERTEX_POINT('',#48201) ;
#14018 = VERTEX_POINT('',#48205) ;
#14019 = VERTEX_POINT('',#48206) ;
#14020 = VERTEX_POINT('',#48208) ;
#14021 = VERTEX_POINT('',#48212) ;
#14022 = VERTEX_POINT('',#48213) ;
#14023 = VERTEX_POINT('',#48215) ;
#14024 = VERTEX_POINT('',#48217) ;
#14025 = VERTEX_POINT('',#48219) ;
#14026 = VERTEX_POINT('',#48223) ;
#14027 = VERTEX_POINT('',#48224) ;
#14028 = VERTEX_POINT('',#48226) ;
#14029 = VERTEX_POINT('',#48230) ;
#14030 = VERTEX_POINT('',#48231) ;
#14031 = VERTEX_POINT('',#48233) ;
#14032 = VERTEX_POINT('',#48237) ;
#14033 = VERTEX_POINT('',#48238) ;
#14034 = VERTEX_POINT('',#48240) ;
#14035 = VERTEX_POINT('',#48244) ;
#14036 = VERTEX_POINT('',#48245) ;
#14037 = VERTEX_POINT('',#48247) ;
#14038 = VERTEX_POINT('',#48249) ;
#14039 = VERTEX_POINT('',#48251) ;
#14040 = VERTEX_POINT('',#48255) ;
#14041 = VERTEX_POINT('',#48256) ;
#14042 = VERTEX_POINT('',#48258) ;
#14043 = VERTEX_POINT('',#48262) ;
#14044 = VERTEX_POINT('',#48263) ;
#14045 = VERTEX_POINT('',#48265) ;
#14046 = VERTEX_POINT('',#48269) ;
#14047 = VERTEX_POINT('',#48270) ;
#14048 = VERTEX_POINT('',#48272) ;
#14049 = VERTEX_POINT('',#48276) ;
#14050 = VERTEX_POINT('',#48277) ;
#14051 = VERTEX_POINT('',#48279) ;
#14052 = VERTEX_POINT('',#48281) ;
#14053 = VERTEX_POINT('',#48283) ;
#14054 = VERTEX_POINT('',#48287) ;
#14055 = VERTEX_POINT('',#48288) ;
#14056 = VERTEX_POINT('',#48290) ;
#14057 = VERTEX_POINT('',#48294) ;
#14058 = VERTEX_POINT('',#48295) ;
#14059 = VERTEX_POINT('',#48297) ;
#14060 = VERTEX_POINT('',#48301) ;
#14061 = VERTEX_POINT('',#48302) ;
#14062 = VERTEX_POINT('',#48304) ;
#14063 = VERTEX_POINT('',#48308) ;
#14064 = VERTEX_POINT('',#48309) ;
#14065 = VERTEX_POINT('',#48311) ;
#14066 = VERTEX_POINT('',#48313) ;
#14067 = VERTEX_POINT('',#48315) ;
#14068 = VERTEX_POINT('',#48319) ;
#14069 = VERTEX_POINT('',#48320) ;
#14070 = VERTEX_POINT('',#48322) ;
#14071 = VERTEX_POINT('',#48326) ;
#14072 = VERTEX_POINT('',#48327) ;
#14073 = VERTEX_POINT('',#48329) ;
#14074 = VERTEX_POINT('',#48333) ;
#14075 = VERTEX_POINT('',#48334) ;
#14076 = VERTEX_POINT('',#48336) ;
#14077 = VERTEX_POINT('',#48340) ;
#14078 = VERTEX_POINT('',#48341) ;
#14079 = VERTEX_POINT('',#48343) ;
#14080 = VERTEX_POINT('',#48345) ;
#14081 = VERTEX_POINT('',#48347) ;
#14082 = VERTEX_POINT('',#48351) ;
#14083 = VERTEX_POINT('',#48352) ;
#14084 = VERTEX_POINT('',#48354) ;
#14085 = VERTEX_POINT('',#48358) ;
#14086 = VERTEX_POINT('',#48359) ;
#14087 = VERTEX_POINT('',#48361) ;
#14088 = VERTEX_POINT('',#48365) ;
#14089 = VERTEX_POINT('',#48366) ;
#14090 = VERTEX_POINT('',#48368) ;
#14091 = VERTEX_POINT('',#48372) ;
#14092 = VERTEX_POINT('',#48373) ;
#14093 = VERTEX_POINT('',#48375) ;
#14094 = VERTEX_POINT('',#48377) ;
#14095 = VERTEX_POINT('',#48379) ;
#14096 = VERTEX_POINT('',#48383) ;
#14097 = VERTEX_POINT('',#48384) ;
#14098 = VERTEX_POINT('',#48386) ;
#14099 = VERTEX_POINT('',#48390) ;
#14100 = VERTEX_POINT('',#48391) ;
#14101 = VERTEX_POINT('',#48393) ;
#14102 = VERTEX_POINT('',#48397) ;
#14103 = VERTEX_POINT('',#48398) ;
#14104 = VERTEX_POINT('',#48400) ;
#14105 = VERTEX_POINT('',#48404) ;
#14106 = VERTEX_POINT('',#48405) ;
#14107 = VERTEX_POINT('',#48407) ;
#14108 = VERTEX_POINT('',#48409) ;
#14109 = VERTEX_POINT('',#48411) ;
#14110 = VERTEX_POINT('',#48415) ;
#14111 = VERTEX_POINT('',#48416) ;
#14112 = VERTEX_POINT('',#48418) ;
#14113 = VERTEX_POINT('',#48422) ;
#14114 = VERTEX_POINT('',#48423) ;
#14115 = VERTEX_POINT('',#48425) ;
#14116 = VERTEX_POINT('',#48429) ;
#14117 = VERTEX_POINT('',#48430) ;
#14118 = VERTEX_POINT('',#48432) ;
#14119 = VERTEX_POINT('',#48436) ;
#14120 = VERTEX_POINT('',#48437) ;
#14121 = VERTEX_POINT('',#48439) ;
#14122 = VERTEX_POINT('',#48441) ;
#14123 = VERTEX_POINT('',#48443) ;
#14124 = VERTEX_POINT('',#48447) ;
#14125 = VERTEX_POINT('',#48448) ;
#14126 = VERTEX_POINT('',#48450) ;
#14127 = VERTEX_POINT('',#48454) ;
#14128 = VERTEX_POINT('',#48455) ;
#14129 = VERTEX_POINT('',#48457) ;
#14130 = VERTEX_POINT('',#48461) ;
#14131 = VERTEX_POINT('',#48462) ;
#14132 = VERTEX_POINT('',#48464) ;
#14133 = VERTEX_POINT('',#48468) ;
#14134 = VERTEX_POINT('',#48469) ;
#14135 = VERTEX_POINT('',#48471) ;
#14136 = VERTEX_POINT('',#48473) ;
#14137 = VERTEX_POINT('',#48475) ;
#14138 = VERTEX_POINT('',#48479) ;
#14139 = VERTEX_POINT('',#48480) ;
#14140 = VERTEX_POINT('',#48482) ;
#14141 = VERTEX_POINT('',#48486) ;
#14142 = VERTEX_POINT('',#48487) ;
#14143 = VERTEX_POINT('',#48489) ;
#14144 = VERTEX_POINT('',#48493) ;
#14145 = VERTEX_POINT('',#48494) ;
#14146 = VERTEX_POINT('',#48496) ;
#14147 = VERTEX_POINT('',#48500) ;
#14148 = VERTEX_POINT('',#48501) ;
#14149 = VERTEX_POINT('',#48503) ;
#14150 = VERTEX_POINT('',#48505) ;
#14151 = VERTEX_POINT('',#48507) ;
#14152 = VERTEX_POINT('',#48511) ;
#14153 = VERTEX_POINT('',#48512) ;
#14154 = VERTEX_POINT('',#48514) ;
#14155 = VERTEX_POINT('',#48518) ;
#14156 = VERTEX_POINT('',#48519) ;
#14157 = VERTEX_POINT('',#48521) ;
#14158 = VERTEX_POINT('',#48525) ;
#14159 = VERTEX_POINT('',#48526) ;
#14160 = VERTEX_POINT('',#48528) ;
#14161 = VERTEX_POINT('',#48532) ;
#14162 = VERTEX_POINT('',#48533) ;
#14163 = VERTEX_POINT('',#48535) ;
#14164 = VERTEX_POINT('',#48537) ;
#14165 = VERTEX_POINT('',#48539) ;
#14166 = VERTEX_POINT('',#48543) ;
#14167 = VERTEX_POINT('',#48544) ;
#14168 = VERTEX_POINT('',#48546) ;
#14169 = VERTEX_POINT('',#48550) ;
#14170 = VERTEX_POINT('',#48551) ;
#14171 = VERTEX_POINT('',#48553) ;
#14172 = VERTEX_POINT('',#48557) ;
#14173 = VERTEX_POINT('',#48558) ;
#14174 = VERTEX_POINT('',#48560) ;
#14175 = VERTEX_POINT('',#48564) ;
#14176 = VERTEX_POINT('',#48565) ;
#14177 = VERTEX_POINT('',#48567) ;
#14178 = VERTEX_POINT('',#48569) ;
#14179 = VERTEX_POINT('',#48571) ;
#14180 = VERTEX_POINT('',#48575) ;
#14181 = VERTEX_POINT('',#48576) ;
#14182 = VERTEX_POINT('',#48578) ;
#14183 = VERTEX_POINT('',#48582) ;
#14184 = VERTEX_POINT('',#48583) ;
#14185 = VERTEX_POINT('',#48585) ;
#14186 = VERTEX_POINT('',#48589) ;
#14187 = VERTEX_POINT('',#48590) ;
#14188 = VERTEX_POINT('',#48592) ;
#14189 = VERTEX_POINT('',#48596) ;
#14190 = VERTEX_POINT('',#48597) ;
#14191 = VERTEX_POINT('',#48599) ;
#14192 = VERTEX_POINT('',#48601) ;
#14193 = VERTEX_POINT('',#48603) ;
#14194 = VERTEX_POINT('',#48607) ;
#14195 = VERTEX_POINT('',#48608) ;
#14196 = VERTEX_POINT('',#48610) ;
#14197 = VERTEX_POINT('',#48614) ;
#14198 = VERTEX_POINT('',#48615) ;
#14199 = VERTEX_POINT('',#48617) ;
#14200 = VERTEX_POINT('',#48621) ;
#14201 = VERTEX_POINT('',#48622) ;
#14202 = VERTEX_POINT('',#48624) ;
#14203 = VERTEX_POINT('',#48628) ;
#14204 = VERTEX_POINT('',#48629) ;
#14205 = VERTEX_POINT('',#48631) ;
#14206 = VERTEX_POINT('',#48633) ;
#14207 = VERTEX_POINT('',#48635) ;
#14208 = VERTEX_POINT('',#48639) ;
#14209 = VERTEX_POINT('',#48640) ;
#14210 = VERTEX_POINT('',#48642) ;
#14211 = VERTEX_POINT('',#48646) ;
#14212 = VERTEX_POINT('',#48647) ;
#14213 = VERTEX_POINT('',#48649) ;
#14214 = VERTEX_POINT('',#48653) ;
#14215 = VERTEX_POINT('',#48654) ;
#14216 = VERTEX_POINT('',#48656) ;
#14217 = VERTEX_POINT('',#48664) ;
#14218 = VERTEX_POINT('',#48669) ;
#14219 = VERTEX_POINT('',#48674) ;
#14220 = VERTEX_POINT('',#48679) ;
#14221 = VERTEX_POINT('',#48684) ;
#14222 = VERTEX_POINT('',#48689) ;
#14223 = VERTEX_POINT('',#48694) ;
#14224 = VERTEX_POINT('',#48699) ;
#14225 = VERTEX_POINT('',#48704) ;
#14226 = VERTEX_POINT('',#48709) ;
#14227 = VERTEX_POINT('',#48714) ;
#14228 = VERTEX_POINT('',#48719) ;
#14229 = VERTEX_POINT('',#48724) ;
#14230 = VERTEX_POINT('',#48729) ;
#14231 = VERTEX_POINT('',#48734) ;
#14232 = VERTEX_POINT('',#48739) ;
#14233 = VERTEX_POINT('',#48744) ;
#14234 = VERTEX_POINT('',#48749) ;
#14235 = VERTEX_POINT('',#48754) ;
#14236 = VERTEX_POINT('',#48759) ;
#14237 = VERTEX_POINT('',#48764) ;
#14238 = VERTEX_POINT('',#48769) ;
#14239 = VERTEX_POINT('',#48774) ;
#14240 = VERTEX_POINT('',#48779) ;
#14241 = VERTEX_POINT('',#48784) ;
#14242 = VERTEX_POINT('',#48789) ;
#14243 = VERTEX_POINT('',#48794) ;
#14244 = VERTEX_POINT('',#48799) ;
#14245 = VERTEX_POINT('',#48804) ;
#14246 = VERTEX_POINT('',#48809) ;
#14247 = VERTEX_POINT('',#48814) ;
#14248 = VERTEX_POINT('',#48819) ;
#14249 = VERTEX_POINT('',#48824) ;
#14250 = VERTEX_POINT('',#48829) ;
#14251 = VERTEX_POINT('',#48834) ;
#14252 = VERTEX_POINT('',#48839) ;
#14253 = VERTEX_POINT('',#48844) ;
#14254 = VERTEX_POINT('',#48849) ;
#14255 = VERTEX_POINT('',#48854) ;
#14256 = VERTEX_POINT('',#48859) ;
#14257 = VERTEX_POINT('',#48864) ;
#14258 = VERTEX_POINT('',#48869) ;
#14259 = VERTEX_POINT('',#48874) ;
#14260 = VERTEX_POINT('',#48879) ;
#14261 = VERTEX_POINT('',#48884) ;
#14262 = VERTEX_POINT('',#48889) ;
#14263 = VERTEX_POINT('',#48894) ;
#14264 = VERTEX_POINT('',#48899) ;
#14265 = VERTEX_POINT('',#48904) ;
#14266 = VERTEX_POINT('',#48909) ;
#14267 = VERTEX_POINT('',#48914) ;
#14268 = VERTEX_POINT('',#48919) ;
#14269 = VERTEX_POINT('',#48924) ;
#14270 = VERTEX_POINT('',#48929) ;
#14271 = VERTEX_POINT('',#48934) ;
#14272 = VERTEX_POINT('',#48939) ;
#14273 = VERTEX_POINT('',#48944) ;
#14274 = VERTEX_POINT('',#48949) ;
#14275 = VERTEX_POINT('',#48954) ;
#14276 = VERTEX_POINT('',#48959) ;
#14277 = VERTEX_POINT('',#48964) ;
#14278 = VERTEX_POINT('',#48969) ;
#14279 = VERTEX_POINT('',#48974) ;
#14280 = VERTEX_POINT('',#48979) ;
#14281 = VERTEX_POINT('',#48984) ;
#14282 = VERTEX_POINT('',#48989) ;
#14283 = VERTEX_POINT('',#48994) ;
#14284 = VERTEX_POINT('',#48999) ;
#14285 = VERTEX_POINT('',#49004) ;
#14286 = VERTEX_POINT('',#49009) ;
#14287 = VERTEX_POINT('',#49014) ;
#14288 = VERTEX_POINT('',#49019) ;
#14289 = VERTEX_POINT('',#49024) ;
#14290 = VERTEX_POINT('',#49029) ;
#14291 = VERTEX_POINT('',#49034) ;
#14292 = VERTEX_POINT('',#49039) ;
#14293 = VERTEX_POINT('',#49044) ;
#14294 = VERTEX_POINT('',#49049) ;
#14295 = VERTEX_POINT('',#49054) ;
#14296 = VERTEX_POINT('',#49059) ;
#14297 = VERTEX_POINT('',#49064) ;
#14298 = VERTEX_POINT('',#49069) ;
#14299 = VERTEX_POINT('',#49074) ;
#14300 = VERTEX_POINT('',#49079) ;
#14301 = VERTEX_POINT('',#49084) ;
#14302 = VERTEX_POINT('',#49089) ;
#14303 = VERTEX_POINT('',#49094) ;
#14304 = VERTEX_POINT('',#49099) ;
#14305 = VERTEX_POINT('',#49104) ;
#14306 = VERTEX_POINT('',#49109) ;
#14307 = VERTEX_POINT('',#49114) ;
#14308 = VERTEX_POINT('',#49119) ;
#14309 = VERTEX_POINT('',#49124) ;
#14310 = VERTEX_POINT('',#49129) ;
#14311 = VERTEX_POINT('',#49134) ;
#14312 = VERTEX_POINT('',#49139) ;
#14313 = VERTEX_POINT('',#49144) ;
#14314 = VERTEX_POINT('',#49149) ;
#14315 = VERTEX_POINT('',#49154) ;
#14316 = VERTEX_POINT('',#49159) ;
#14317 = VERTEX_POINT('',#49164) ;
#14318 = VERTEX_POINT('',#49169) ;
#14319 = VERTEX_POINT('',#49174) ;
#14320 = VERTEX_POINT('',#49179) ;
#14321 = VERTEX_POINT('',#49184) ;
#14322 = VERTEX_POINT('',#49189) ;
#14323 = VERTEX_POINT('',#49194) ;
#14324 = VERTEX_POINT('',#49199) ;
#14325 = VERTEX_POINT('',#49204) ;
#14326 = VERTEX_POINT('',#49209) ;
#14327 = VERTEX_POINT('',#49214) ;
#14328 = VERTEX_POINT('',#49219) ;
#14329 = VERTEX_POINT('',#49224) ;
#14330 = VERTEX_POINT('',#49229) ;
#14331 = VERTEX_POINT('',#49234) ;
#14332 = VERTEX_POINT('',#49239) ;
#14333 = VERTEX_POINT('',#49244) ;
#14334 = VERTEX_POINT('',#49249) ;
#14335 = VERTEX_POINT('',#49254) ;
#14336 = VERTEX_POINT('',#49259) ;
#14337 = VERTEX_POINT('',#49264) ;
#14338 = VERTEX_POINT('',#49269) ;
#14339 = VERTEX_POINT('',#49274) ;
#14340 = VERTEX_POINT('',#49279) ;
#14341 = VERTEX_POINT('',#49284) ;
#14342 = VERTEX_POINT('',#49289) ;
#14343 = VERTEX_POINT('',#49294) ;
#14344 = VERTEX_POINT('',#49296) ;
#14345 = VERTEX_POINT('',#49298) ;
#14346 = VERTEX_POINT('',#49317) ;
#14347 = VERTEX_POINT('',#49320) ;
#14348 = VERTEX_POINT('',#49342) ;
#14349 = VERTEX_POINT('',#49344) ;
#14350 = VERTEX_POINT('',#49350) ;
#14351 = VERTEX_POINT('',#49371) ;
#14352 = VERTEX_POINT('',#49372) ;
#14353 = VERTEX_POINT('',#49375) ;
#14354 = VERTEX_POINT('',#49376) ;
#14355 = VERTEX_POINT('',#49383) ;
#14356 = VERTEX_POINT('',#49385) ;
#14357 = VERTEX_POINT('',#49388) ;
#14358 = VERTEX_POINT('',#49389) ;
#14359 = VERTEX_POINT('',#49430) ;
#14360 = VERTEX_POINT('',#49431) ;
#14361 = VERTEX_POINT('',#49433) ;
#14362 = VERTEX_POINT('',#49438) ;
#14363 = VERTEX_POINT('',#49440) ;
#14364 = VERTEX_POINT('',#49443) ;
#14365 = VERTEX_POINT('',#49444) ;
#14366 = VERTEX_POINT('',#49485) ;
#14367 = VERTEX_POINT('',#49490) ;
#14368 = VERTEX_POINT('',#49495) ;
#14369 = VERTEX_POINT('',#49502) ;
#14370 = VERTEX_POINT('',#49506) ;
#14371 = VERTEX_POINT('',#49508) ;
#14372 = VERTEX_POINT('',#49513) ;
#14373 = VERTEX_POINT('',#49514) ;
#14374 = VERTEX_POINT('',#49516) ;
#14375 = VERTEX_POINT('',#49518) ;
#14376 = VERTEX_POINT('',#49522) ;
#14377 = VERTEX_POINT('',#49523) ;
#14378 = VERTEX_POINT('',#49526) ;
#14379 = VERTEX_POINT('',#49530) ;
#14380 = VERTEX_POINT('',#49531) ;
#14381 = VERTEX_POINT('',#49533) ;
#14382 = VERTEX_POINT('',#49545) ;
#14383 = VERTEX_POINT('',#49548) ;
#14384 = VERTEX_POINT('',#49549) ;
#14385 = VERTEX_POINT('',#49553) ;
#14386 = VERTEX_POINT('',#49555) ;
#14387 = VERTEX_POINT('',#49595) ;
#14388 = VERTEX_POINT('',#49596) ;
#14389 = VERTEX_POINT('',#49638) ;
#14390 = VERTEX_POINT('',#49639) ;
#14391 = VERTEX_POINT('',#49677) ;
#14392 = VERTEX_POINT('',#49679) ;
#14393 = VERTEX_POINT('',#49718) ;
#14394 = VERTEX_POINT('',#49719) ;
#14395 = VERTEX_POINT('',#49725) ;
#14396 = VERTEX_POINT('',#49731) ;
#14397 = VERTEX_POINT('',#49732) ;
#14398 = VERTEX_POINT('',#49734) ;
#14399 = VERTEX_POINT('',#49736) ;
#14400 = VERTEX_POINT('',#49738) ;
#14401 = VERTEX_POINT('',#49740) ;
#14402 = VERTEX_POINT('',#49742) ;
#14403 = VERTEX_POINT('',#49744) ;
#14404 = VERTEX_POINT('',#49747) ;
#14405 = VERTEX_POINT('',#49748) ;
#14406 = VERTEX_POINT('',#49752) ;
#14407 = VERTEX_POINT('',#49756) ;
#14408 = VERTEX_POINT('',#49763) ;
#14409 = VERTEX_POINT('',#49765) ;
#14410 = VERTEX_POINT('',#49769) ;
#14411 = VERTEX_POINT('',#49771) ;
#14412 = VERTEX_POINT('',#49778) ;
#14413 = VERTEX_POINT('',#49779) ;
#14414 = VERTEX_POINT('',#49781) ;
#14415 = VERTEX_POINT('',#49783) ;
#14416 = VERTEX_POINT('',#49787) ;
#14417 = VERTEX_POINT('',#49789) ;
#14418 = VERTEX_POINT('',#49791) ;
#14419 = VERTEX_POINT('',#49793) ;
#14420 = VERTEX_POINT('',#49797) ;
#14421 = VERTEX_POINT('',#49801) ;
#14422 = VERTEX_POINT('',#49805) ;
#14423 = VERTEX_POINT('',#49806) ;
#14424 = VERTEX_POINT('',#49816) ;
#14425 = VERTEX_POINT('',#49817) ;
#14426 = VERTEX_POINT('',#49819) ;
#14427 = VERTEX_POINT('',#49821) ;
#14428 = VERTEX_POINT('',#49825) ;
#14429 = VERTEX_POINT('',#49826) ;
#14430 = VERTEX_POINT('',#49828) ;
#14431 = VERTEX_POINT('',#49830) ;
#14432 = VERTEX_POINT('',#49843) ;
#14433 = VERTEX_POINT('',#49844) ;
#14434 = VERTEX_POINT('',#49846) ;
#14435 = VERTEX_POINT('',#49848) ;
#14436 = VERTEX_POINT('',#49850) ;
#14437 = VERTEX_POINT('',#49852) ;
#14438 = VERTEX_POINT('',#49856) ;
#14439 = VERTEX_POINT('',#49858) ;
#14440 = VERTEX_POINT('',#49862) ;
#14441 = VERTEX_POINT('',#49866) ;
#14442 = VERTEX_POINT('',#49868) ;
#14443 = VERTEX_POINT('',#49874) ;
#14444 = VERTEX_POINT('',#49878) ;
#14445 = VERTEX_POINT('',#49881) ;
#14446 = VERTEX_POINT('',#49884) ;
#14447 = VERTEX_POINT('',#49888) ;
#14448 = VERTEX_POINT('',#49901) ;
#14449 = VERTEX_POINT('',#49903) ;
#14450 = VERTEX_POINT('',#49908) ;
#14451 = VERTEX_POINT('',#49909) ;
#14452 = VERTEX_POINT('',#49911) ;
#14453 = VERTEX_POINT('',#49913) ;
#14454 = VERTEX_POINT('',#49917) ;
#14455 = VERTEX_POINT('',#49918) ;
#14456 = VERTEX_POINT('',#49920) ;
#14457 = VERTEX_POINT('',#49922) ;
#14458 = VERTEX_POINT('',#49926) ;
#14459 = VERTEX_POINT('',#49929) ;
#14460 = VERTEX_POINT('',#49933) ;
#14461 = VERTEX_POINT('',#49937) ;
#14462 = VERTEX_POINT('',#49947) ;
#14463 = VERTEX_POINT('',#49949) ;
#14464 = VERTEX_POINT('',#49953) ;
#14465 = VERTEX_POINT('',#49954) ;
#14466 = VERTEX_POINT('',#49956) ;
#14467 = VERTEX_POINT('',#49958) ;
#14468 = VERTEX_POINT('',#49962) ;
#14469 = VERTEX_POINT('',#49963) ;
#14470 = VERTEX_POINT('',#49965) ;
#14471 = VERTEX_POINT('',#49967) ;
#14472 = VERTEX_POINT('',#49971) ;
#14473 = VERTEX_POINT('',#49974) ;
#14474 = VERTEX_POINT('',#49978) ;
#14475 = VERTEX_POINT('',#49982) ;
#14476 = VERTEX_POINT('',#49992) ;
#14477 = VERTEX_POINT('',#49994) ;
#14478 = VERTEX_POINT('',#49999) ;
#14479 = VERTEX_POINT('',#50000) ;
#14480 = VERTEX_POINT('',#50002) ;
#14481 = VERTEX_POINT('',#50004) ;
#14482 = VERTEX_POINT('',#50008) ;
#14483 = VERTEX_POINT('',#50009) ;
#14484 = VERTEX_POINT('',#50011) ;
#14485 = VERTEX_POINT('',#50013) ;
#14486 = VERTEX_POINT('',#50017) ;
#14487 = VERTEX_POINT('',#50020) ;
#14488 = VERTEX_POINT('',#50024) ;
#14489 = VERTEX_POINT('',#50028) ;
#14490 = VERTEX_POINT('',#50038) ;
#14491 = VERTEX_POINT('',#50040) ;
#14492 = VERTEX_POINT('',#50044) ;
#14493 = VERTEX_POINT('',#50045) ;
#14494 = VERTEX_POINT('',#50047) ;
#14495 = VERTEX_POINT('',#50049) ;
#14496 = VERTEX_POINT('',#50053) ;
#14497 = VERTEX_POINT('',#50054) ;
#14498 = VERTEX_POINT('',#50056) ;
#14499 = VERTEX_POINT('',#50058) ;
#14500 = VERTEX_POINT('',#50062) ;
#14501 = VERTEX_POINT('',#50065) ;
#14502 = VERTEX_POINT('',#50069) ;
#14503 = VERTEX_POINT('',#50073) ;
#14504 = VERTEX_POINT('',#50083) ;
#14505 = VERTEX_POINT('',#50085) ;
#14506 = VERTEX_POINT('',#50088) ;
#14507 = VERTEX_POINT('',#50093) ;
#14508 = VERTEX_POINT('',#50099) ;
#14509 = VERTEX_POINT('',#50101) ;
#14510 = VERTEX_POINT('',#50104) ;
#14511 = VERTEX_POINT('',#50109) ;
#14512 = VERTEX_POINT('',#50115) ;
#14513 = VERTEX_POINT('',#50116) ;
#14514 = VERTEX_POINT('',#50118) ;
#14515 = VERTEX_POINT('',#50141) ;
#14516 = VERTEX_POINT('',#50143) ;
#14517 = VERTEX_POINT('',#50145) ;
#14518 = VERTEX_POINT('',#50147) ;
#14519 = VERTEX_POINT('',#50149) ;
#14520 = VERTEX_POINT('',#50154) ;
#14521 = VERTEX_POINT('',#50155) ;
#14522 = VERTEX_POINT('',#50159) ;
#14523 = VERTEX_POINT('',#50160) ;
#14524 = VERTEX_POINT('',#50164) ;
#14525 = VERTEX_POINT('',#50165) ;
#14526 = VERTEX_POINT('',#50169) ;
#14527 = VERTEX_POINT('',#50170) ;
#14528 = VERTEX_POINT('',#50172) ;
#14529 = VERTEX_POINT('',#50174) ;
#14530 = VERTEX_POINT('',#50178) ;
#14531 = VERTEX_POINT('',#50179) ;
#14532 = VERTEX_POINT('',#50181) ;
#14533 = VERTEX_POINT('',#50183) ;
#14534 = VERTEX_POINT('',#50187) ;
#14535 = VERTEX_POINT('',#50188) ;
#14536 = VERTEX_POINT('',#50190) ;
#14537 = VERTEX_POINT('',#50192) ;
#14538 = VERTEX_POINT('',#50196) ;
#14539 = VERTEX_POINT('',#50197) ;
#14540 = VERTEX_POINT('',#50199) ;
#14541 = VERTEX_POINT('',#50201) ;
#14542 = VERTEX_POINT('',#50205) ;
#14543 = VERTEX_POINT('',#50206) ;
#14544 = VERTEX_POINT('',#50208) ;
#14545 = VERTEX_POINT('',#50210) ;
#14546 = VERTEX_POINT('',#50214) ;
#14547 = VERTEX_POINT('',#50215) ;
#14548 = VERTEX_POINT('',#50217) ;
#14549 = VERTEX_POINT('',#50219) ;
#14550 = VERTEX_POINT('',#50225) ;
#14551 = VERTEX_POINT('',#50226) ;
#14552 = VERTEX_POINT('',#50230) ;
#14553 = VERTEX_POINT('',#50233) ;
#14554 = VERTEX_POINT('',#50238) ;
#14555 = VERTEX_POINT('',#50243) ;
#14556 = VERTEX_POINT('',#50263) ;
#14557 = VERTEX_POINT('',#50265) ;
#14558 = VERTEX_POINT('',#50279) ;
#14559 = VERTEX_POINT('',#50294) ;
#14560 = VERTEX_POINT('',#50303) ;
#14561 = EDGE_CURVE('',#11855,#11855,#10688,.T.) ;
#14562 = EDGE_CURVE('',#11855,#11856,#5744,.T.) ;
#14563 = EDGE_CURVE('',#11856,#11856,#10689,.T.) ;
#14564 = EDGE_CURVE('',#11857,#11858,#5745,.T.) ;
#14565 = EDGE_CURVE('',#11859,#11857,#5746,.T.) ;
#14566 = EDGE_CURVE('',#11859,#11860,#5747,.T.) ;
#14567 = EDGE_CURVE('',#11861,#11860,#5748,.T.) ;
#14568 = EDGE_CURVE('',#11862,#11861,#5749,.T.) ;
#14569 = EDGE_CURVE('',#11863,#11862,#5750,.T.) ;
#14570 = EDGE_CURVE('',#11863,#11864,#5751,.T.) ;
#14571 = EDGE_CURVE('',#11858,#11864,#5752,.T.) ;
#14572 = EDGE_CURVE('',#11865,#11859,#5753,.T.) ;
#14573 = EDGE_CURVE('',#11865,#11866,#5754,.T.) ;
#14574 = EDGE_CURVE('',#11860,#11866,#5755,.T.) ;
#14575 = EDGE_CURVE('',#11862,#11867,#5756,.T.) ;
#14576 = EDGE_CURVE('',#11867,#11868,#5757,.T.) ;
#14577 = EDGE_CURVE('',#11868,#11863,#5758,.T.) ;
#14578 = EDGE_CURVE('',#11868,#11869,#5759,.T.) ;
#14579 = EDGE_CURVE('',#11864,#11869,#5760,.T.) ;
#14580 = EDGE_CURVE('',#11858,#11870,#10690,.T.) ;
#14581 = EDGE_CURVE('',#11869,#11870,#5761,.T.) ;
#14582 = EDGE_CURVE('',#11866,#11871,#5762,.T.) ;
#14583 = EDGE_CURVE('',#11871,#11861,#5763,.T.) ;
#14584 = EDGE_CURVE('',#11870,#11872,#5764,.T.) ;
#14585 = EDGE_CURVE('',#11867,#11871,#5765,.T.) ;
#14586 = EDGE_CURVE('',#11872,#11865,#5766,.T.) ;
#14587 = EDGE_CURVE('',#11873,#11873,#10691,.T.) ;
#14588 = EDGE_CURVE('',#11873,#11874,#5767,.T.) ;
#14589 = EDGE_CURVE('',#11875,#11874,#10692,.T.) ;
#14590 = EDGE_CURVE('',#11875,#11876,#5768,.T.) ;
#14591 = EDGE_CURVE('',#11876,#11877,#10693,.T.) ;
#14592 = EDGE_CURVE('',#11877,#11878,#5769,.T.) ;
#14593 = EDGE_CURVE('',#11857,#11878,#10694,.T.) ;
#14594 = EDGE_CURVE('',#11874,#11872,#10695,.T.) ;
#14595 = EDGE_CURVE('',#11879,#11879,#10696,.T.) ;
#14596 = EDGE_CURVE('',#11879,#11880,#5770,.T.) ;
#14597 = EDGE_CURVE('',#11880,#11880,#10697,.T.) ;
#14598 = EDGE_CURVE('',#11881,#11875,#5771,.T.) ;
#14599 = EDGE_CURVE('',#11881,#11882,#5772,.T.) ;
#14600 = EDGE_CURVE('',#11883,#11882,#5773,.T.) ;
#14601 = EDGE_CURVE('',#11884,#11883,#5774,.T.) ;
#14602 = EDGE_CURVE('',#11885,#11884,#5775,.T.) ;
#14603 = EDGE_CURVE('',#11885,#11886,#5776,.T.) ;
#14604 = EDGE_CURVE('',#11876,#11886,#5777,.T.) ;
#14605 = EDGE_CURVE('',#11887,#11881,#5778,.T.) ;
#14606 = EDGE_CURVE('',#11887,#11888,#5779,.T.) ;
#14607 = EDGE_CURVE('',#11882,#11888,#5780,.T.) ;
#14608 = EDGE_CURVE('',#11884,#11889,#5781,.T.) ;
#14609 = EDGE_CURVE('',#11889,#11890,#5782,.T.) ;
#14610 = EDGE_CURVE('',#11890,#11885,#5783,.T.) ;
#14611 = EDGE_CURVE('',#11890,#11891,#5784,.T.) ;
#14612 = EDGE_CURVE('',#11886,#11891,#5785,.T.) ;
#14613 = EDGE_CURVE('',#11891,#11877,#5786,.T.) ;
#14614 = EDGE_CURVE('',#11888,#11892,#5787,.T.) ;
#14615 = EDGE_CURVE('',#11892,#11883,#5788,.T.) ;
#14616 = EDGE_CURVE('',#11889,#11892,#5789,.T.) ;
#14617 = EDGE_CURVE('',#11878,#11887,#5790,.T.) ;
#14618 = EDGE_CURVE('',#11893,#11894,#10698,.T.) ;
#14619 = EDGE_CURVE('',#11893,#11895,#5791,.T.) ;
#14620 = EDGE_CURVE('',#11895,#11896,#5792,.T.) ;
#14621 = EDGE_CURVE('',#11896,#11894,#5793,.T.) ;
#14622 = EDGE_CURVE('',#11897,#11893,#1096,.T.) ;
#14623 = EDGE_CURVE('',#11898,#11897,#5794,.T.) ;
#14624 = EDGE_CURVE('',#11895,#11898,#5795,.T.) ;
#14625 = EDGE_CURVE('',#11894,#11899,#1097,.T.) ;
#14626 = EDGE_CURVE('',#11896,#11900,#5796,.T.) ;
#14627 = EDGE_CURVE('',#11899,#11900,#5797,.T.) ;
#14628 = EDGE_CURVE('',#11901,#11902,#1098,.T.) ;
#14629 = EDGE_CURVE('',#11903,#11901,#5798,.T.) ;
#14630 = EDGE_CURVE('',#11904,#11903,#5799,.T.) ;
#14631 = EDGE_CURVE('',#11902,#11904,#5800,.T.) ;
#14632 = EDGE_CURVE('',#11899,#11897,#10699,.T.) ;
#14633 = EDGE_CURVE('',#11900,#11898,#5801,.T.) ;
#14634 = EDGE_CURVE('',#11905,#11901,#10700,.T.) ;
#14635 = EDGE_CURVE('',#11905,#11906,#5802,.T.) ;
#14636 = EDGE_CURVE('',#11906,#11903,#5803,.T.) ;
#14637 = EDGE_CURVE('',#11902,#11907,#10701,.T.) ;
#14638 = EDGE_CURVE('',#11904,#11908,#5804,.T.) ;
#14639 = EDGE_CURVE('',#11908,#11907,#5805,.T.) ;
#14640 = EDGE_CURVE('',#11907,#11905,#1099,.T.) ;
#14641 = EDGE_CURVE('',#11908,#11906,#5806,.T.) ;
#14642 = EDGE_CURVE('',#11909,#11910,#10702,.T.) ;
#14643 = EDGE_CURVE('',#11909,#11911,#5807,.T.) ;
#14644 = EDGE_CURVE('',#11911,#11912,#5808,.T.) ;
#14645 = EDGE_CURVE('',#11912,#11910,#5809,.T.) ;
#14646 = EDGE_CURVE('',#11913,#11909,#1100,.T.) ;
#14647 = EDGE_CURVE('',#11914,#11913,#5810,.T.) ;
#14648 = EDGE_CURVE('',#11911,#11914,#5811,.T.) ;
#14649 = EDGE_CURVE('',#11910,#11915,#1101,.T.) ;
#14650 = EDGE_CURVE('',#11912,#11916,#5812,.T.) ;
#14651 = EDGE_CURVE('',#11915,#11916,#5813,.T.) ;
#14652 = EDGE_CURVE('',#11917,#11918,#1102,.T.) ;
#14653 = EDGE_CURVE('',#11919,#11917,#5814,.T.) ;
#14654 = EDGE_CURVE('',#11920,#11919,#5815,.T.) ;
#14655 = EDGE_CURVE('',#11918,#11920,#5816,.T.) ;
#14656 = EDGE_CURVE('',#11915,#11913,#10703,.T.) ;
#14657 = EDGE_CURVE('',#11916,#11914,#5817,.T.) ;
#14658 = EDGE_CURVE('',#11921,#11917,#10704,.T.) ;
#14659 = EDGE_CURVE('',#11921,#11922,#5818,.T.) ;
#14660 = EDGE_CURVE('',#11922,#11919,#5819,.T.) ;
#14661 = EDGE_CURVE('',#11918,#11923,#10705,.T.) ;
#14662 = EDGE_CURVE('',#11920,#11924,#5820,.T.) ;
#14663 = EDGE_CURVE('',#11924,#11923,#5821,.T.) ;
#14664 = EDGE_CURVE('',#11923,#11921,#1103,.T.) ;
#14665 = EDGE_CURVE('',#11924,#11922,#5822,.T.) ;
#14666 = EDGE_CURVE('',#11925,#11926,#10706,.T.) ;
#14667 = EDGE_CURVE('',#11925,#11927,#5823,.T.) ;
#14668 = EDGE_CURVE('',#11927,#11928,#5824,.T.) ;
#14669 = EDGE_CURVE('',#11928,#11926,#5825,.T.) ;
#14670 = EDGE_CURVE('',#11929,#11925,#1104,.T.) ;
#14671 = EDGE_CURVE('',#11930,#11929,#5826,.T.) ;
#14672 = EDGE_CURVE('',#11927,#11930,#5827,.T.) ;
#14673 = EDGE_CURVE('',#11926,#11931,#1105,.T.) ;
#14674 = EDGE_CURVE('',#11928,#11932,#5828,.T.) ;
#14675 = EDGE_CURVE('',#11931,#11932,#5829,.T.) ;
#14676 = EDGE_CURVE('',#11933,#11934,#1106,.T.) ;
#14677 = EDGE_CURVE('',#11935,#11933,#5830,.T.) ;
#14678 = EDGE_CURVE('',#11936,#11935,#5831,.T.) ;
#14679 = EDGE_CURVE('',#11934,#11936,#5832,.T.) ;
#14680 = EDGE_CURVE('',#11931,#11929,#10707,.T.) ;
#14681 = EDGE_CURVE('',#11932,#11930,#5833,.T.) ;
#14682 = EDGE_CURVE('',#11937,#11933,#10708,.T.) ;
#14683 = EDGE_CURVE('',#11937,#11938,#5834,.T.) ;
#14684 = EDGE_CURVE('',#11938,#11935,#5835,.T.) ;
#14685 = EDGE_CURVE('',#11934,#11939,#10709,.T.) ;
#14686 = EDGE_CURVE('',#11936,#11940,#5836,.T.) ;
#14687 = EDGE_CURVE('',#11940,#11939,#5837,.T.) ;
#14688 = EDGE_CURVE('',#11939,#11937,#1107,.T.) ;
#14689 = EDGE_CURVE('',#11940,#11938,#5838,.T.) ;
#14690 = EDGE_CURVE('',#11941,#11942,#10710,.T.) ;
#14691 = EDGE_CURVE('',#11941,#11943,#5839,.T.) ;
#14692 = EDGE_CURVE('',#11943,#11944,#5840,.T.) ;
#14693 = EDGE_CURVE('',#11944,#11942,#5841,.T.) ;
#14694 = EDGE_CURVE('',#11945,#11941,#1108,.T.) ;
#14695 = EDGE_CURVE('',#11946,#11945,#5842,.T.) ;
#14696 = EDGE_CURVE('',#11943,#11946,#5843,.T.) ;
#14697 = EDGE_CURVE('',#11942,#11947,#1109,.T.) ;
#14698 = EDGE_CURVE('',#11944,#11948,#5844,.T.) ;
#14699 = EDGE_CURVE('',#11947,#11948,#5845,.T.) ;
#14700 = EDGE_CURVE('',#11949,#11950,#1110,.T.) ;
#14701 = EDGE_CURVE('',#11951,#11949,#5846,.T.) ;
#14702 = EDGE_CURVE('',#11952,#11951,#5847,.T.) ;
#14703 = EDGE_CURVE('',#11950,#11952,#5848,.T.) ;
#14704 = EDGE_CURVE('',#11947,#11945,#10711,.T.) ;
#14705 = EDGE_CURVE('',#11948,#11946,#5849,.T.) ;
#14706 = EDGE_CURVE('',#11953,#11949,#10712,.T.) ;
#14707 = EDGE_CURVE('',#11953,#11954,#5850,.T.) ;
#14708 = EDGE_CURVE('',#11954,#11951,#5851,.T.) ;
#14709 = EDGE_CURVE('',#11950,#11955,#10713,.T.) ;
#14710 = EDGE_CURVE('',#11952,#11956,#5852,.T.) ;
#14711 = EDGE_CURVE('',#11956,#11955,#5853,.T.) ;
#14712 = EDGE_CURVE('',#11955,#11953,#1111,.T.) ;
#14713 = EDGE_CURVE('',#11956,#11954,#5854,.T.) ;
#14714 = EDGE_CURVE('',#11957,#11957,#10714,.T.) ;
#14715 = EDGE_CURVE('',#11957,#11958,#5855,.T.) ;
#14716 = EDGE_CURVE('',#11958,#11958,#10715,.T.) ;
#14717 = EDGE_CURVE('',#11959,#11959,#10716,.T.) ;
#14718 = EDGE_CURVE('',#11959,#11960,#5856,.T.) ;
#14719 = EDGE_CURVE('',#11960,#11960,#10717,.T.) ;
#14720 = EDGE_CURVE('',#11961,#11961,#10718,.T.) ;
#14721 = EDGE_CURVE('',#11961,#11959,#5857,.T.) ;
#14722 = EDGE_CURVE('',#11958,#11962,#5858,.T.) ;
#14723 = EDGE_CURVE('',#11962,#11962,#10719,.T.) ;
#14724 = EDGE_CURVE('',#11963,#11964,#5859,.T.) ;
#14725 = EDGE_CURVE('',#11965,#11963,#5860,.T.) ;
#14726 = EDGE_CURVE('',#11966,#11965,#5861,.T.) ;
#14727 = EDGE_CURVE('',#11964,#11966,#5862,.T.) ;
#14728 = EDGE_CURVE('',#11964,#11967,#5863,.T.) ;
#14729 = EDGE_CURVE('',#11968,#11966,#5864,.T.) ;
#14730 = EDGE_CURVE('',#11968,#11967,#5865,.T.) ;
#14731 = EDGE_CURVE('',#11969,#11963,#5866,.T.) ;
#14732 = EDGE_CURVE('',#11969,#11970,#5867,.T.) ;
#14733 = EDGE_CURVE('',#11965,#11970,#5868,.T.) ;
#14734 = EDGE_CURVE('',#11971,#11967,#5869,.T.) ;
#14735 = EDGE_CURVE('',#11972,#11971,#5870,.T.) ;
#14736 = EDGE_CURVE('',#11973,#11972,#5871,.T.) ;
#14737 = EDGE_CURVE('',#11973,#11974,#5872,.T.) ;
#14738 = EDGE_CURVE('',#11969,#11974,#5873,.T.) ;
#14739 = EDGE_CURVE('',#11975,#11970,#5874,.T.) ;
#14740 = EDGE_CURVE('',#11976,#11975,#5875,.T.) ;
#14741 = EDGE_CURVE('',#11977,#11976,#5876,.T.) ;
#14742 = EDGE_CURVE('',#11977,#11978,#5877,.T.) ;
#14743 = EDGE_CURVE('',#11968,#11978,#5878,.T.) ;
#14744 = EDGE_CURVE('',#11976,#11973,#5879,.T.) ;
#14745 = EDGE_CURVE('',#11972,#11977,#5880,.T.) ;
#14746 = EDGE_CURVE('',#11978,#11971,#5881,.T.) ;
#14747 = EDGE_CURVE('',#11974,#11975,#5882,.T.) ;
#14748 = EDGE_CURVE('',#11979,#11979,#10720,.T.) ;
#14749 = EDGE_CURVE('',#11979,#11980,#5883,.T.) ;
#14750 = EDGE_CURVE('',#11980,#11980,#10721,.T.) ;
#14751 = EDGE_CURVE('',#11981,#11981,#10722,.T.) ;
#14752 = EDGE_CURVE('',#11982,#11982,#10723,.T.) ;
#14753 = EDGE_CURVE('',#11982,#11981,#5884,.T.) ;
#14754 = EDGE_CURVE('',#11983,#11984,#5885,.T.) ;
#14755 = EDGE_CURVE('',#11983,#11985,#5886,.T.) ;
#14756 = EDGE_CURVE('',#11985,#11986,#5887,.T.) ;
#14757 = EDGE_CURVE('',#11986,#11984,#5888,.T.) ;
#14758 = EDGE_CURVE('',#11987,#11988,#5889,.T.) ;
#14759 = EDGE_CURVE('',#11987,#11989,#5890,.T.) ;
#14760 = EDGE_CURVE('',#11989,#11990,#5891,.T.) ;
#14761 = EDGE_CURVE('',#11990,#11988,#5892,.T.) ;
#14762 = EDGE_CURVE('',#11985,#11990,#5893,.T.) ;
#14763 = EDGE_CURVE('',#11986,#11989,#5894,.T.) ;
#14764 = EDGE_CURVE('',#11987,#11984,#10724,.T.) ;
#14765 = EDGE_CURVE('',#11983,#11988,#10725,.T.) ;
#14766 = EDGE_CURVE('',#11991,#11992,#5895,.T.) ;
#14767 = EDGE_CURVE('',#11993,#11991,#5896,.T.) ;
#14768 = EDGE_CURVE('',#11994,#11993,#5897,.T.) ;
#14769 = EDGE_CURVE('',#11992,#11994,#5898,.T.) ;
#14770 = EDGE_CURVE('',#11995,#11996,#5899,.T.) ;
#14771 = EDGE_CURVE('',#11997,#11995,#5900,.T.) ;
#14772 = EDGE_CURVE('',#11998,#11997,#5901,.T.) ;
#14773 = EDGE_CURVE('',#11996,#11998,#5902,.T.) ;
#14774 = EDGE_CURVE('',#11999,#12000,#5903,.T.) ;
#14775 = EDGE_CURVE('',#12001,#11999,#5904,.T.) ;
#14776 = EDGE_CURVE('',#12002,#12001,#5905,.T.) ;
#14777 = EDGE_CURVE('',#12000,#12002,#5906,.T.) ;
#14778 = EDGE_CURVE('',#12003,#12004,#5907,.T.) ;
#14779 = EDGE_CURVE('',#12005,#12003,#5908,.T.) ;
#14780 = EDGE_CURVE('',#12006,#12005,#5909,.T.) ;
#14781 = EDGE_CURVE('',#12004,#12006,#5910,.T.) ;
#14782 = EDGE_CURVE('',#12007,#12008,#5911,.T.) ;
#14783 = EDGE_CURVE('',#12009,#12007,#5912,.T.) ;
#14784 = EDGE_CURVE('',#12010,#12009,#5913,.T.) ;
#14785 = EDGE_CURVE('',#12008,#12010,#5914,.T.) ;
#14786 = EDGE_CURVE('',#12011,#12012,#5915,.T.) ;
#14787 = EDGE_CURVE('',#12013,#12011,#5916,.T.) ;
#14788 = EDGE_CURVE('',#12014,#12013,#5917,.T.) ;
#14789 = EDGE_CURVE('',#12012,#12014,#5918,.T.) ;
#14790 = EDGE_CURVE('',#12015,#12016,#5919,.T.) ;
#14791 = EDGE_CURVE('',#12017,#12015,#5920,.T.) ;
#14792 = EDGE_CURVE('',#12018,#12017,#5921,.T.) ;
#14793 = EDGE_CURVE('',#12016,#12018,#5922,.T.) ;
#14794 = EDGE_CURVE('',#12019,#12020,#5923,.T.) ;
#14795 = EDGE_CURVE('',#12021,#12019,#5924,.T.) ;
#14796 = EDGE_CURVE('',#12021,#12022,#5925,.T.) ;
#14797 = EDGE_CURVE('',#12020,#12022,#5926,.T.) ;
#14798 = EDGE_CURVE('',#12023,#12024,#5927,.T.) ;
#14799 = EDGE_CURVE('',#12025,#12023,#5928,.T.) ;
#14800 = EDGE_CURVE('',#12026,#12025,#5929,.T.) ;
#14801 = EDGE_CURVE('',#12024,#12026,#5930,.T.) ;
#14802 = EDGE_CURVE('',#12027,#12028,#5931,.T.) ;
#14803 = EDGE_CURVE('',#12029,#12027,#5932,.T.) ;
#14804 = EDGE_CURVE('',#12030,#12029,#5933,.T.) ;
#14805 = EDGE_CURVE('',#12028,#12030,#5934,.T.) ;
#14806 = EDGE_CURVE('',#12031,#12032,#5935,.T.) ;
#14807 = EDGE_CURVE('',#12033,#12031,#5936,.T.) ;
#14808 = EDGE_CURVE('',#12034,#12033,#5937,.T.) ;
#14809 = EDGE_CURVE('',#12032,#12034,#5938,.T.) ;
#14810 = EDGE_CURVE('',#12035,#12036,#5939,.T.) ;
#14811 = EDGE_CURVE('',#12037,#12035,#5940,.T.) ;
#14812 = EDGE_CURVE('',#12038,#12037,#5941,.T.) ;
#14813 = EDGE_CURVE('',#12036,#12038,#5942,.T.) ;
#14814 = EDGE_CURVE('',#12039,#12040,#5943,.T.) ;
#14815 = EDGE_CURVE('',#12022,#12039,#5944,.T.) ;
#14816 = EDGE_CURVE('',#12040,#12021,#5945,.T.) ;
#14817 = EDGE_CURVE('',#12041,#12042,#5946,.T.) ;
#14818 = EDGE_CURVE('',#12018,#12041,#5947,.T.) ;
#14819 = EDGE_CURVE('',#12042,#12017,#5948,.T.) ;
#14820 = EDGE_CURVE('',#12043,#12016,#10726,.T.) ;
#14821 = EDGE_CURVE('',#12043,#12044,#5949,.T.) ;
#14822 = EDGE_CURVE('',#12015,#12044,#10727,.T.) ;
#14823 = EDGE_CURVE('',#12045,#12042,#10728,.T.) ;
#14824 = EDGE_CURVE('',#12045,#12046,#5950,.T.) ;
#14825 = EDGE_CURVE('',#12041,#12046,#10729,.T.) ;
#14826 = EDGE_CURVE('',#12047,#12036,#10730,.T.) ;
#14827 = EDGE_CURVE('',#12047,#12048,#5951,.T.) ;
#14828 = EDGE_CURVE('',#12035,#12048,#10731,.T.) ;
#14829 = EDGE_CURVE('',#12049,#12013,#5952,.T.) ;
#14830 = EDGE_CURVE('',#12049,#12050,#5953,.T.) ;
#14831 = EDGE_CURVE('',#12014,#12050,#5954,.T.) ;
#14832 = EDGE_CURVE('',#12051,#12032,#5955,.T.) ;
#14833 = EDGE_CURVE('',#12052,#12051,#5956,.T.) ;
#14834 = EDGE_CURVE('',#12031,#12052,#5957,.T.) ;
#14835 = EDGE_CURVE('',#12053,#12009,#5958,.T.) ;
#14836 = EDGE_CURVE('',#12053,#12054,#5959,.T.) ;
#14837 = EDGE_CURVE('',#12010,#12054,#5960,.T.) ;
#14838 = EDGE_CURVE('',#12055,#12028,#5961,.T.) ;
#14839 = EDGE_CURVE('',#12056,#12055,#5962,.T.) ;
#14840 = EDGE_CURVE('',#12027,#12056,#5963,.T.) ;
#14841 = EDGE_CURVE('',#12057,#12005,#5964,.T.) ;
#14842 = EDGE_CURVE('',#12057,#12058,#5965,.T.) ;
#14843 = EDGE_CURVE('',#12006,#12058,#5966,.T.) ;
#14844 = EDGE_CURVE('',#12059,#12024,#5967,.T.) ;
#14845 = EDGE_CURVE('',#12060,#12059,#5968,.T.) ;
#14846 = EDGE_CURVE('',#12023,#12060,#5969,.T.) ;
#14847 = EDGE_CURVE('',#12061,#12001,#5970,.T.) ;
#14848 = EDGE_CURVE('',#12061,#12062,#5971,.T.) ;
#14849 = EDGE_CURVE('',#12002,#12062,#5972,.T.) ;
#14850 = EDGE_CURVE('',#12063,#11997,#5973,.T.) ;
#14851 = EDGE_CURVE('',#12063,#12064,#5974,.T.) ;
#14852 = EDGE_CURVE('',#11998,#12064,#5975,.T.) ;
#14853 = EDGE_CURVE('',#12046,#12065,#5976,.T.) ;
#14854 = EDGE_CURVE('',#12065,#12066,#5977,.T.) ;
#14855 = EDGE_CURVE('',#12066,#12067,#10732,.T.) ;
#14856 = EDGE_CURVE('',#12067,#12068,#5978,.T.) ;
#14857 = EDGE_CURVE('',#12068,#12069,#5979,.T.) ;
#14858 = EDGE_CURVE('',#12069,#12070,#10733,.T.) ;
#14859 = EDGE_CURVE('',#12070,#12071,#5980,.T.) ;
#14860 = EDGE_CURVE('',#12071,#12072,#5981,.T.) ;
#14861 = EDGE_CURVE('',#12072,#12073,#10734,.T.) ;
#14862 = EDGE_CURVE('',#12073,#12074,#5982,.T.) ;
#14863 = EDGE_CURVE('',#12074,#12075,#5983,.T.) ;
#14864 = EDGE_CURVE('',#12075,#12076,#5984,.T.) ;
#14865 = EDGE_CURVE('',#12076,#12077,#10735,.T.) ;
#14866 = EDGE_CURVE('',#12077,#12078,#5985,.T.) ;
#14867 = EDGE_CURVE('',#12078,#12079,#5986,.T.) ;
#14868 = EDGE_CURVE('',#12079,#12080,#10736,.T.) ;
#14869 = EDGE_CURVE('',#12080,#12081,#5987,.T.) ;
#14870 = EDGE_CURVE('',#12081,#12082,#5988,.T.) ;
#14871 = EDGE_CURVE('',#12082,#12083,#10737,.T.) ;
#14872 = EDGE_CURVE('',#12083,#12084,#5989,.T.) ;
#14873 = EDGE_CURVE('',#12084,#12085,#5990,.T.) ;
#14874 = EDGE_CURVE('',#12085,#12086,#10738,.T.) ;
#14875 = EDGE_CURVE('',#12086,#12087,#5991,.T.) ;
#14876 = EDGE_CURVE('',#12087,#12088,#5992,.T.) ;
#14877 = EDGE_CURVE('',#12088,#12089,#10739,.T.) ;
#14878 = EDGE_CURVE('',#12089,#12090,#5993,.T.) ;
#14879 = EDGE_CURVE('',#12090,#12091,#5994,.T.) ;
#14880 = EDGE_CURVE('',#12091,#12092,#10740,.T.) ;
#14881 = EDGE_CURVE('',#12092,#12093,#5995,.T.) ;
#14882 = EDGE_CURVE('',#12093,#12094,#5996,.T.) ;
#14883 = EDGE_CURVE('',#12094,#12095,#10741,.T.) ;
#14884 = EDGE_CURVE('',#12095,#12096,#5997,.T.) ;
#14885 = EDGE_CURVE('',#12096,#12097,#5998,.T.) ;
#14886 = EDGE_CURVE('',#12097,#12098,#5999,.T.) ;
#14887 = EDGE_CURVE('',#12098,#12099,#10742,.T.) ;
#14888 = EDGE_CURVE('',#12099,#12100,#6000,.T.) ;
#14889 = EDGE_CURVE('',#12100,#12101,#6001,.T.) ;
#14890 = EDGE_CURVE('',#12101,#12102,#10743,.T.) ;
#14891 = EDGE_CURVE('',#12102,#12103,#6002,.T.) ;
#14892 = EDGE_CURVE('',#12103,#12104,#6003,.T.) ;
#14893 = EDGE_CURVE('',#12104,#12105,#10744,.T.) ;
#14894 = EDGE_CURVE('',#12105,#12106,#6004,.T.) ;
#14895 = EDGE_CURVE('',#12106,#12107,#6005,.T.) ;
#14896 = EDGE_CURVE('',#12107,#12108,#10745,.T.) ;
#14897 = EDGE_CURVE('',#12108,#12109,#6006,.T.) ;
#14898 = EDGE_CURVE('',#12109,#12110,#6007,.T.) ;
#14899 = EDGE_CURVE('',#12110,#12111,#10746,.T.) ;
#14900 = EDGE_CURVE('',#12111,#12112,#6008,.T.) ;
#14901 = EDGE_CURVE('',#12112,#12113,#6009,.T.) ;
#14902 = EDGE_CURVE('',#12113,#12114,#10747,.T.) ;
#14903 = EDGE_CURVE('',#12114,#12115,#6010,.T.) ;
#14904 = EDGE_CURVE('',#12115,#12116,#6011,.T.) ;
#14905 = EDGE_CURVE('',#12116,#12117,#10748,.T.) ;
#14906 = EDGE_CURVE('',#12117,#12118,#6012,.T.) ;
#14907 = EDGE_CURVE('',#12118,#12119,#6013,.T.) ;
#14908 = EDGE_CURVE('',#12119,#12120,#6014,.T.) ;
#14909 = EDGE_CURVE('',#12120,#12121,#10749,.T.) ;
#14910 = EDGE_CURVE('',#12121,#12122,#6015,.T.) ;
#14911 = EDGE_CURVE('',#12122,#12123,#6016,.T.) ;
#14912 = EDGE_CURVE('',#12123,#12124,#10750,.T.) ;
#14913 = EDGE_CURVE('',#12124,#12125,#6017,.T.) ;
#14914 = EDGE_CURVE('',#12125,#12126,#6018,.T.) ;
#14915 = EDGE_CURVE('',#12126,#12127,#10751,.T.) ;
#14916 = EDGE_CURVE('',#12127,#12128,#6019,.T.) ;
#14917 = EDGE_CURVE('',#12128,#12129,#6020,.T.) ;
#14918 = EDGE_CURVE('',#12129,#12040,#10752,.T.) ;
#14919 = EDGE_CURVE('',#12019,#12130,#10753,.T.) ;
#14920 = EDGE_CURVE('',#12130,#12131,#6021,.T.) ;
#14921 = EDGE_CURVE('',#12131,#12132,#6022,.T.) ;
#14922 = EDGE_CURVE('',#12132,#12133,#10754,.T.) ;
#14923 = EDGE_CURVE('',#12133,#12134,#6023,.T.) ;
#14924 = EDGE_CURVE('',#12134,#12135,#6024,.T.) ;
#14925 = EDGE_CURVE('',#12135,#12136,#10755,.T.) ;
#14926 = EDGE_CURVE('',#12136,#12137,#6025,.T.) ;
#14927 = EDGE_CURVE('',#12137,#12138,#6026,.T.) ;
#14928 = EDGE_CURVE('',#12138,#12139,#6027,.T.) ;
#14929 = EDGE_CURVE('',#12139,#12140,#10756,.T.) ;
#14930 = EDGE_CURVE('',#12140,#12141,#6028,.T.) ;
#14931 = EDGE_CURVE('',#12141,#12142,#6029,.T.) ;
#14932 = EDGE_CURVE('',#12142,#12143,#10757,.T.) ;
#14933 = EDGE_CURVE('',#12143,#12144,#6030,.T.) ;
#14934 = EDGE_CURVE('',#12144,#12043,#6031,.T.) ;
#14935 = EDGE_CURVE('',#12048,#12037,#6032,.T.) ;
#14936 = EDGE_CURVE('',#12052,#12145,#10758,.T.) ;
#14937 = EDGE_CURVE('',#12145,#12033,#6033,.T.) ;
#14938 = EDGE_CURVE('',#12056,#12146,#10759,.T.) ;
#14939 = EDGE_CURVE('',#12146,#12029,#6034,.T.) ;
#14940 = EDGE_CURVE('',#12060,#12025,#10760,.T.) ;
#14941 = EDGE_CURVE('',#12054,#12147,#6035,.T.) ;
#14942 = EDGE_CURVE('',#12147,#12008,#6036,.T.) ;
#14943 = EDGE_CURVE('',#12058,#12148,#6037,.T.) ;
#14944 = EDGE_CURVE('',#12148,#12004,#6038,.T.) ;
#14945 = EDGE_CURVE('',#12062,#12149,#6039,.T.) ;
#14946 = EDGE_CURVE('',#12149,#12000,#6040,.T.) ;
#14947 = EDGE_CURVE('',#12064,#12150,#6041,.T.) ;
#14948 = EDGE_CURVE('',#12150,#11996,#6042,.T.) ;
#14949 = EDGE_CURVE('',#12050,#12151,#6043,.T.) ;
#14950 = EDGE_CURVE('',#12151,#12152,#6044,.T.) ;
#14951 = EDGE_CURVE('',#12152,#12012,#10761,.T.) ;
#14952 = EDGE_CURVE('',#12153,#12154,#6045,.T.) ;
#14953 = EDGE_CURVE('',#12154,#12155,#10762,.T.) ;
#14954 = EDGE_CURVE('',#12155,#12153,#6046,.T.) ;
#14955 = EDGE_CURVE('',#12156,#12157,#6047,.T.) ;
#14956 = EDGE_CURVE('',#12157,#12158,#6048,.T.) ;
#14957 = EDGE_CURVE('',#12158,#12159,#6049,.T.) ;
#14958 = EDGE_CURVE('',#12159,#12156,#6050,.T.) ;
#14959 = EDGE_CURVE('',#12160,#12161,#6051,.T.) ;
#14960 = EDGE_CURVE('',#12161,#12162,#6052,.T.) ;
#14961 = EDGE_CURVE('',#12162,#12163,#6053,.T.) ;
#14962 = EDGE_CURVE('',#12163,#12160,#6054,.T.) ;
#14963 = EDGE_CURVE('',#12164,#12165,#6055,.T.) ;
#14964 = EDGE_CURVE('',#12165,#12166,#6056,.T.) ;
#14965 = EDGE_CURVE('',#12166,#12167,#6057,.T.) ;
#14966 = EDGE_CURVE('',#12167,#12164,#6058,.T.) ;
#14967 = EDGE_CURVE('',#12168,#12169,#6059,.T.) ;
#14968 = EDGE_CURVE('',#12169,#12170,#6060,.T.) ;
#14969 = EDGE_CURVE('',#12170,#12171,#6061,.T.) ;
#14970 = EDGE_CURVE('',#12171,#12168,#6062,.T.) ;
#14971 = EDGE_CURVE('',#12172,#12173,#6063,.T.) ;
#14972 = EDGE_CURVE('',#12173,#12174,#6064,.T.) ;
#14973 = EDGE_CURVE('',#12174,#12175,#10763,.T.) ;
#14974 = EDGE_CURVE('',#12175,#12172,#6065,.T.) ;
#14975 = EDGE_CURVE('',#12176,#12177,#6066,.T.) ;
#14976 = EDGE_CURVE('',#12177,#12178,#6067,.T.) ;
#14977 = EDGE_CURVE('',#12178,#12179,#10764,.T.) ;
#14978 = EDGE_CURVE('',#12179,#12176,#6068,.T.) ;
#14979 = EDGE_CURVE('',#12180,#12181,#6069,.T.) ;
#14980 = EDGE_CURVE('',#12181,#12182,#6070,.T.) ;
#14981 = EDGE_CURVE('',#12182,#12183,#6071,.T.) ;
#14982 = EDGE_CURVE('',#12183,#12184,#10765,.T.) ;
#14983 = EDGE_CURVE('',#12184,#12180,#6072,.T.) ;
#14984 = EDGE_CURVE('',#12185,#12186,#6073,.T.) ;
#14985 = EDGE_CURVE('',#12186,#12187,#10766,.T.) ;
#14986 = EDGE_CURVE('',#12187,#12185,#6074,.T.) ;
#14987 = EDGE_CURVE('',#12188,#12189,#10767,.T.) ;
#14988 = EDGE_CURVE('',#12189,#12190,#6075,.T.) ;
#14989 = EDGE_CURVE('',#12190,#12191,#6076,.T.) ;
#14990 = EDGE_CURVE('',#12191,#12188,#6077,.T.) ;
#14991 = EDGE_CURVE('',#12192,#12193,#6078,.T.) ;
#14992 = EDGE_CURVE('',#12193,#12194,#6079,.T.) ;
#14993 = EDGE_CURVE('',#12194,#12195,#6080,.T.) ;
#14994 = EDGE_CURVE('',#12195,#12192,#6081,.T.) ;
#14995 = EDGE_CURVE('',#12196,#12197,#6082,.T.) ;
#14996 = EDGE_CURVE('',#12197,#12198,#6083,.T.) ;
#14997 = EDGE_CURVE('',#12198,#12199,#6084,.T.) ;
#14998 = EDGE_CURVE('',#12199,#12196,#6085,.T.) ;
#14999 = EDGE_CURVE('',#12200,#12201,#6086,.T.) ;
#15000 = EDGE_CURVE('',#12201,#12202,#6087,.T.) ;
#15001 = EDGE_CURVE('',#12202,#12203,#6088,.T.) ;
#15002 = EDGE_CURVE('',#12203,#12200,#6089,.T.) ;
#15003 = EDGE_CURVE('',#12204,#12205,#6090,.T.) ;
#15004 = EDGE_CURVE('',#12205,#12206,#6091,.T.) ;
#15005 = EDGE_CURVE('',#12206,#12207,#6092,.T.) ;
#15006 = EDGE_CURVE('',#12207,#12204,#6093,.T.) ;
#15007 = EDGE_CURVE('',#12208,#12209,#6094,.T.) ;
#15008 = EDGE_CURVE('',#12209,#12210,#6095,.T.) ;
#15009 = EDGE_CURVE('',#12210,#12211,#6096,.T.) ;
#15010 = EDGE_CURVE('',#12211,#12208,#6097,.T.) ;
#15011 = EDGE_CURVE('',#12212,#12213,#6098,.T.) ;
#15012 = EDGE_CURVE('',#12213,#12214,#6099,.T.) ;
#15013 = EDGE_CURVE('',#12214,#12215,#10768,.T.) ;
#15014 = EDGE_CURVE('',#12215,#12212,#6100,.T.) ;
#15015 = EDGE_CURVE('',#12216,#12217,#6101,.T.) ;
#15016 = EDGE_CURVE('',#12217,#12218,#6102,.T.) ;
#15017 = EDGE_CURVE('',#12218,#12219,#6103,.T.) ;
#15018 = EDGE_CURVE('',#12219,#12216,#6104,.T.) ;
#15019 = EDGE_CURVE('',#12220,#12221,#6105,.T.) ;
#15020 = EDGE_CURVE('',#12221,#12222,#6106,.T.) ;
#15021 = EDGE_CURVE('',#12222,#12223,#6107,.T.) ;
#15022 = EDGE_CURVE('',#12223,#12220,#6108,.T.) ;
#15023 = EDGE_CURVE('',#12224,#12225,#6109,.T.) ;
#15024 = EDGE_CURVE('',#12225,#12226,#10769,.T.) ;
#15025 = EDGE_CURVE('',#12226,#12224,#6110,.T.) ;
#15026 = EDGE_CURVE('',#12227,#12228,#6111,.T.) ;
#15027 = EDGE_CURVE('',#12228,#12229,#6112,.T.) ;
#15028 = EDGE_CURVE('',#12229,#12230,#10770,.T.) ;
#15029 = EDGE_CURVE('',#12230,#12231,#6113,.T.) ;
#15030 = EDGE_CURVE('',#12231,#12227,#6114,.T.) ;
#15031 = EDGE_CURVE('',#12232,#12233,#6115,.T.) ;
#15032 = EDGE_CURVE('',#12233,#12234,#10771,.T.) ;
#15033 = EDGE_CURVE('',#12234,#12232,#6116,.T.) ;
#15034 = EDGE_CURVE('',#12235,#12236,#6117,.T.) ;
#15035 = EDGE_CURVE('',#12236,#12237,#6118,.T.) ;
#15036 = EDGE_CURVE('',#12237,#12238,#6119,.T.) ;
#15037 = EDGE_CURVE('',#12238,#12235,#6120,.T.) ;
#15038 = EDGE_CURVE('',#12239,#12240,#6121,.T.) ;
#15039 = EDGE_CURVE('',#12240,#12241,#10772,.T.) ;
#15040 = EDGE_CURVE('',#12241,#12239,#6122,.T.) ;
#15041 = EDGE_CURVE('',#12242,#12243,#6123,.T.) ;
#15042 = EDGE_CURVE('',#12243,#12244,#6124,.T.) ;
#15043 = EDGE_CURVE('',#12244,#12245,#10773,.T.) ;
#15044 = EDGE_CURVE('',#12245,#12242,#6125,.T.) ;
#15045 = EDGE_CURVE('',#12246,#12247,#6126,.T.) ;
#15046 = EDGE_CURVE('',#12247,#12248,#6127,.T.) ;
#15047 = EDGE_CURVE('',#12248,#12249,#6128,.T.) ;
#15048 = EDGE_CURVE('',#12249,#12246,#6129,.T.) ;
#15049 = EDGE_CURVE('',#12250,#12251,#6130,.T.) ;
#15050 = EDGE_CURVE('',#12251,#12252,#6131,.T.) ;
#15051 = EDGE_CURVE('',#12252,#12253,#6132,.T.) ;
#15052 = EDGE_CURVE('',#12253,#12250,#6133,.T.) ;
#15053 = EDGE_CURVE('',#12254,#12255,#6134,.T.) ;
#15054 = EDGE_CURVE('',#12255,#12256,#6135,.T.) ;
#15055 = EDGE_CURVE('',#12256,#12257,#6136,.T.) ;
#15056 = EDGE_CURVE('',#12257,#12254,#6137,.T.) ;
#15057 = EDGE_CURVE('',#12258,#12259,#6138,.T.) ;
#15058 = EDGE_CURVE('',#12259,#12260,#6139,.T.) ;
#15059 = EDGE_CURVE('',#12260,#12261,#6140,.T.) ;
#15060 = EDGE_CURVE('',#12261,#12258,#6141,.T.) ;
#15061 = EDGE_CURVE('',#12262,#12263,#6142,.T.) ;
#15062 = EDGE_CURVE('',#12263,#12264,#6143,.T.) ;
#15063 = EDGE_CURVE('',#12264,#12265,#6144,.T.) ;
#15064 = EDGE_CURVE('',#12265,#12262,#6145,.T.) ;
#15065 = EDGE_CURVE('',#12266,#12267,#6146,.T.) ;
#15066 = EDGE_CURVE('',#12267,#12268,#6147,.T.) ;
#15067 = EDGE_CURVE('',#12268,#12269,#6148,.T.) ;
#15068 = EDGE_CURVE('',#12269,#12266,#6149,.T.) ;
#15069 = EDGE_CURVE('',#12270,#12271,#6150,.T.) ;
#15070 = EDGE_CURVE('',#12271,#12272,#6151,.T.) ;
#15071 = EDGE_CURVE('',#12272,#12270,#10774,.T.) ;
#15072 = EDGE_CURVE('',#12273,#12274,#6152,.T.) ;
#15073 = EDGE_CURVE('',#12274,#12275,#6153,.T.) ;
#15074 = EDGE_CURVE('',#12275,#12276,#6154,.T.) ;
#15075 = EDGE_CURVE('',#12276,#12273,#6155,.T.) ;
#15076 = EDGE_CURVE('',#12277,#12278,#10775,.T.) ;
#15077 = EDGE_CURVE('',#12278,#12279,#6156,.T.) ;
#15078 = EDGE_CURVE('',#12279,#12280,#6157,.T.) ;
#15079 = EDGE_CURVE('',#12280,#12277,#6158,.T.) ;
#15080 = EDGE_CURVE('',#12281,#12282,#6159,.T.) ;
#15081 = EDGE_CURVE('',#12282,#12283,#6160,.T.) ;
#15082 = EDGE_CURVE('',#12283,#12284,#6161,.T.) ;
#15083 = EDGE_CURVE('',#12284,#12281,#6162,.T.) ;
#15084 = EDGE_CURVE('',#12285,#12286,#6163,.T.) ;
#15085 = EDGE_CURVE('',#12286,#12287,#6164,.T.) ;
#15086 = EDGE_CURVE('',#12287,#12288,#6165,.T.) ;
#15087 = EDGE_CURVE('',#12288,#12285,#6166,.T.) ;
#15088 = EDGE_CURVE('',#12289,#12290,#6167,.T.) ;
#15089 = EDGE_CURVE('',#12290,#12291,#6168,.T.) ;
#15090 = EDGE_CURVE('',#12291,#12292,#6169,.T.) ;
#15091 = EDGE_CURVE('',#12292,#12289,#6170,.T.) ;
#15092 = EDGE_CURVE('',#12293,#12294,#6171,.T.) ;
#15093 = EDGE_CURVE('',#12294,#12295,#6172,.T.) ;
#15094 = EDGE_CURVE('',#12295,#12296,#6173,.T.) ;
#15095 = EDGE_CURVE('',#12296,#12293,#6174,.T.) ;
#15096 = EDGE_CURVE('',#12297,#12298,#6175,.T.) ;
#15097 = EDGE_CURVE('',#12298,#12299,#6176,.T.) ;
#15098 = EDGE_CURVE('',#12299,#12300,#6177,.T.) ;
#15099 = EDGE_CURVE('',#12300,#12297,#6178,.T.) ;
#15100 = EDGE_CURVE('',#12301,#12302,#6179,.T.) ;
#15101 = EDGE_CURVE('',#12302,#12303,#6180,.T.) ;
#15102 = EDGE_CURVE('',#12303,#12304,#6181,.T.) ;
#15103 = EDGE_CURVE('',#12304,#12301,#6182,.T.) ;
#15104 = EDGE_CURVE('',#12305,#12306,#6183,.T.) ;
#15105 = EDGE_CURVE('',#12306,#12307,#6184,.T.) ;
#15106 = EDGE_CURVE('',#12307,#12308,#6185,.T.) ;
#15107 = EDGE_CURVE('',#12308,#12305,#6186,.T.) ;
#15108 = EDGE_CURVE('',#12309,#12310,#6187,.T.) ;
#15109 = EDGE_CURVE('',#12310,#12311,#6188,.T.) ;
#15110 = EDGE_CURVE('',#12311,#12312,#6189,.T.) ;
#15111 = EDGE_CURVE('',#12312,#12309,#6190,.T.) ;
#15112 = EDGE_CURVE('',#12313,#12314,#6191,.T.) ;
#15113 = EDGE_CURVE('',#12314,#12315,#6192,.T.) ;
#15114 = EDGE_CURVE('',#12315,#12316,#6193,.T.) ;
#15115 = EDGE_CURVE('',#12316,#12313,#6194,.T.) ;
#15116 = EDGE_CURVE('',#11994,#12317,#10776,.T.) ;
#15117 = EDGE_CURVE('',#12317,#12318,#6195,.T.) ;
#15118 = EDGE_CURVE('',#12318,#12319,#6196,.T.) ;
#15119 = EDGE_CURVE('',#12319,#11992,#6197,.T.) ;
#15120 = EDGE_CURVE('',#12320,#11993,#10777,.T.) ;
#15121 = EDGE_CURVE('',#12320,#12317,#6198,.T.) ;
#15122 = EDGE_CURVE('',#12044,#12321,#6199,.T.) ;
#15123 = EDGE_CURVE('',#12321,#12322,#6200,.T.) ;
#15124 = EDGE_CURVE('',#12322,#12323,#10778,.T.) ;
#15125 = EDGE_CURVE('',#12323,#12324,#6201,.T.) ;
#15126 = EDGE_CURVE('',#12324,#12325,#6202,.T.) ;
#15127 = EDGE_CURVE('',#12325,#12326,#10779,.T.) ;
#15128 = EDGE_CURVE('',#12326,#12327,#6203,.T.) ;
#15129 = EDGE_CURVE('',#12327,#12328,#6204,.T.) ;
#15130 = EDGE_CURVE('',#12328,#12329,#6205,.T.) ;
#15131 = EDGE_CURVE('',#12329,#12330,#10780,.T.) ;
#15132 = EDGE_CURVE('',#12330,#12331,#6206,.T.) ;
#15133 = EDGE_CURVE('',#12331,#12332,#6207,.T.) ;
#15134 = EDGE_CURVE('',#12332,#12333,#10781,.T.) ;
#15135 = EDGE_CURVE('',#12333,#12334,#6208,.T.) ;
#15136 = EDGE_CURVE('',#12334,#12335,#6209,.T.) ;
#15137 = EDGE_CURVE('',#12335,#12020,#10782,.T.) ;
#15138 = EDGE_CURVE('',#12039,#12336,#10783,.T.) ;
#15139 = EDGE_CURVE('',#12336,#12337,#6210,.T.) ;
#15140 = EDGE_CURVE('',#12337,#12338,#6211,.T.) ;
#15141 = EDGE_CURVE('',#12338,#12339,#10784,.T.) ;
#15142 = EDGE_CURVE('',#12339,#12340,#6212,.T.) ;
#15143 = EDGE_CURVE('',#12340,#12341,#6213,.T.) ;
#15144 = EDGE_CURVE('',#12341,#12342,#10785,.T.) ;
#15145 = EDGE_CURVE('',#12342,#12343,#6214,.T.) ;
#15146 = EDGE_CURVE('',#12343,#12344,#6215,.T.) ;
#15147 = EDGE_CURVE('',#12344,#12345,#10786,.T.) ;
#15148 = EDGE_CURVE('',#12345,#12346,#6216,.T.) ;
#15149 = EDGE_CURVE('',#12346,#12347,#6217,.T.) ;
#15150 = EDGE_CURVE('',#12347,#12348,#6218,.T.) ;
#15151 = EDGE_CURVE('',#12348,#12349,#10787,.T.) ;
#15152 = EDGE_CURVE('',#12349,#12350,#6219,.T.) ;
#15153 = EDGE_CURVE('',#12350,#12351,#6220,.T.) ;
#15154 = EDGE_CURVE('',#12351,#12352,#10788,.T.) ;
#15155 = EDGE_CURVE('',#12352,#12353,#6221,.T.) ;
#15156 = EDGE_CURVE('',#12353,#12354,#6222,.T.) ;
#15157 = EDGE_CURVE('',#12354,#12355,#10789,.T.) ;
#15158 = EDGE_CURVE('',#12355,#12356,#6223,.T.) ;
#15159 = EDGE_CURVE('',#12356,#12357,#6224,.T.) ;
#15160 = EDGE_CURVE('',#12357,#12358,#10790,.T.) ;
#15161 = EDGE_CURVE('',#12358,#12359,#6225,.T.) ;
#15162 = EDGE_CURVE('',#12359,#12360,#6226,.T.) ;
#15163 = EDGE_CURVE('',#12360,#12361,#10791,.T.) ;
#15164 = EDGE_CURVE('',#12361,#12362,#6227,.T.) ;
#15165 = EDGE_CURVE('',#12362,#12363,#6228,.T.) ;
#15166 = EDGE_CURVE('',#12363,#12364,#10792,.T.) ;
#15167 = EDGE_CURVE('',#12364,#12365,#6229,.T.) ;
#15168 = EDGE_CURVE('',#12365,#12366,#6230,.T.) ;
#15169 = EDGE_CURVE('',#12366,#12367,#10793,.T.) ;
#15170 = EDGE_CURVE('',#12367,#12368,#6231,.T.) ;
#15171 = EDGE_CURVE('',#12368,#12369,#6232,.T.) ;
#15172 = EDGE_CURVE('',#12369,#12370,#6233,.T.) ;
#15173 = EDGE_CURVE('',#12370,#12371,#10794,.T.) ;
#15174 = EDGE_CURVE('',#12371,#12372,#6234,.T.) ;
#15175 = EDGE_CURVE('',#12372,#12373,#6235,.T.) ;
#15176 = EDGE_CURVE('',#12373,#12374,#10795,.T.) ;
#15177 = EDGE_CURVE('',#12374,#12375,#6236,.T.) ;
#15178 = EDGE_CURVE('',#12375,#12376,#6237,.T.) ;
#15179 = EDGE_CURVE('',#12376,#12377,#10796,.T.) ;
#15180 = EDGE_CURVE('',#12377,#12378,#6238,.T.) ;
#15181 = EDGE_CURVE('',#12378,#12379,#6239,.T.) ;
#15182 = EDGE_CURVE('',#12379,#12380,#10797,.T.) ;
#15183 = EDGE_CURVE('',#12380,#12381,#6240,.T.) ;
#15184 = EDGE_CURVE('',#12381,#12382,#6241,.T.) ;
#15185 = EDGE_CURVE('',#12382,#12383,#10798,.T.) ;
#15186 = EDGE_CURVE('',#12383,#12384,#6242,.T.) ;
#15187 = EDGE_CURVE('',#12384,#12385,#6243,.T.) ;
#15188 = EDGE_CURVE('',#12385,#12386,#10799,.T.) ;
#15189 = EDGE_CURVE('',#12386,#12387,#6244,.T.) ;
#15190 = EDGE_CURVE('',#12387,#12388,#6245,.T.) ;
#15191 = EDGE_CURVE('',#12388,#12389,#10800,.T.) ;
#15192 = EDGE_CURVE('',#12389,#12390,#6246,.T.) ;
#15193 = EDGE_CURVE('',#12390,#12391,#6247,.T.) ;
#15194 = EDGE_CURVE('',#12391,#12392,#6248,.T.) ;
#15195 = EDGE_CURVE('',#12392,#12393,#10801,.T.) ;
#15196 = EDGE_CURVE('',#12393,#12394,#6249,.T.) ;
#15197 = EDGE_CURVE('',#12394,#12395,#6250,.T.) ;
#15198 = EDGE_CURVE('',#12395,#12396,#10802,.T.) ;
#15199 = EDGE_CURVE('',#12396,#12397,#6251,.T.) ;
#15200 = EDGE_CURVE('',#12397,#12398,#6252,.T.) ;
#15201 = EDGE_CURVE('',#12398,#12399,#10803,.T.) ;
#15202 = EDGE_CURVE('',#12399,#12400,#6253,.T.) ;
#15203 = EDGE_CURVE('',#12400,#12045,#6254,.T.) ;
#15204 = EDGE_CURVE('',#12007,#12401,#6255,.T.) ;
#15205 = EDGE_CURVE('',#12401,#12053,#6256,.T.) ;
#15206 = EDGE_CURVE('',#12003,#12402,#6257,.T.) ;
#15207 = EDGE_CURVE('',#12402,#12057,#6258,.T.) ;
#15208 = EDGE_CURVE('',#11999,#12403,#6259,.T.) ;
#15209 = EDGE_CURVE('',#12403,#12061,#6260,.T.) ;
#15210 = EDGE_CURVE('',#11995,#12404,#6261,.T.) ;
#15211 = EDGE_CURVE('',#12404,#12063,#6262,.T.) ;
#15212 = EDGE_CURVE('',#12011,#12405,#10804,.T.) ;
#15213 = EDGE_CURVE('',#12405,#12406,#6263,.T.) ;
#15214 = EDGE_CURVE('',#12406,#12049,#6264,.T.) ;
#15215 = EDGE_CURVE('',#12034,#12407,#6265,.T.) ;
#15216 = EDGE_CURVE('',#12407,#12051,#10805,.T.) ;
#15217 = EDGE_CURVE('',#12030,#12408,#6266,.T.) ;
#15218 = EDGE_CURVE('',#12408,#12055,#10806,.T.) ;
#15219 = EDGE_CURVE('',#12026,#12059,#10807,.T.) ;
#15220 = EDGE_CURVE('',#11991,#12409,#6267,.T.) ;
#15221 = EDGE_CURVE('',#12409,#12410,#6268,.T.) ;
#15222 = EDGE_CURVE('',#12410,#12320,#6269,.T.) ;
#15223 = EDGE_CURVE('',#12038,#12047,#6270,.T.) ;
#15224 = EDGE_CURVE('',#12411,#12412,#6271,.T.) ;
#15225 = EDGE_CURVE('',#12412,#12413,#10808,.T.) ;
#15226 = EDGE_CURVE('',#12413,#12414,#6272,.T.) ;
#15227 = EDGE_CURVE('',#12414,#12415,#6273,.T.) ;
#15228 = EDGE_CURVE('',#12415,#12411,#6274,.T.) ;
#15229 = EDGE_CURVE('',#12416,#12417,#6275,.T.) ;
#15230 = EDGE_CURVE('',#12417,#12418,#6276,.T.) ;
#15231 = EDGE_CURVE('',#12418,#12419,#6277,.T.) ;
#15232 = EDGE_CURVE('',#12419,#12416,#6278,.T.) ;
#15233 = EDGE_CURVE('',#12420,#12421,#6279,.T.) ;
#15234 = EDGE_CURVE('',#12421,#12422,#6280,.T.) ;
#15235 = EDGE_CURVE('',#12422,#12423,#6281,.T.) ;
#15236 = EDGE_CURVE('',#12423,#12420,#6282,.T.) ;
#15237 = EDGE_CURVE('',#12424,#12425,#6283,.T.) ;
#15238 = EDGE_CURVE('',#12425,#12426,#6284,.T.) ;
#15239 = EDGE_CURVE('',#12426,#12427,#6285,.T.) ;
#15240 = EDGE_CURVE('',#12427,#12424,#6286,.T.) ;
#15241 = EDGE_CURVE('',#12428,#12429,#6287,.T.) ;
#15242 = EDGE_CURVE('',#12429,#12430,#6288,.T.) ;
#15243 = EDGE_CURVE('',#12430,#12431,#6289,.T.) ;
#15244 = EDGE_CURVE('',#12431,#12428,#6290,.T.) ;
#15245 = EDGE_CURVE('',#12432,#12433,#6291,.T.) ;
#15246 = EDGE_CURVE('',#12433,#12434,#10809,.T.) ;
#15247 = EDGE_CURVE('',#12434,#12432,#6292,.T.) ;
#15248 = EDGE_CURVE('',#12435,#12436,#6293,.T.) ;
#15249 = EDGE_CURVE('',#12436,#12437,#6294,.T.) ;
#15250 = EDGE_CURVE('',#12437,#12438,#6295,.T.) ;
#15251 = EDGE_CURVE('',#12438,#12435,#6296,.T.) ;
#15252 = EDGE_CURVE('',#12439,#12440,#6297,.T.) ;
#15253 = EDGE_CURVE('',#12440,#12441,#6298,.T.) ;
#15254 = EDGE_CURVE('',#12441,#12442,#6299,.T.) ;
#15255 = EDGE_CURVE('',#12442,#12439,#6300,.T.) ;
#15256 = EDGE_CURVE('',#12443,#12444,#6301,.T.) ;
#15257 = EDGE_CURVE('',#12444,#12445,#6302,.T.) ;
#15258 = EDGE_CURVE('',#12445,#12446,#6303,.T.) ;
#15259 = EDGE_CURVE('',#12446,#12443,#6304,.T.) ;
#15260 = EDGE_CURVE('',#12447,#12448,#6305,.T.) ;
#15261 = EDGE_CURVE('',#12448,#12449,#6306,.T.) ;
#15262 = EDGE_CURVE('',#12449,#12450,#6307,.T.) ;
#15263 = EDGE_CURVE('',#12450,#12447,#6308,.T.) ;
#15264 = EDGE_CURVE('',#12451,#12452,#6309,.T.) ;
#15265 = EDGE_CURVE('',#12452,#12453,#6310,.T.) ;
#15266 = EDGE_CURVE('',#12453,#12454,#6311,.T.) ;
#15267 = EDGE_CURVE('',#12454,#12451,#6312,.T.) ;
#15268 = EDGE_CURVE('',#12455,#12456,#6313,.T.) ;
#15269 = EDGE_CURVE('',#12456,#12457,#6314,.T.) ;
#15270 = EDGE_CURVE('',#12457,#12458,#6315,.T.) ;
#15271 = EDGE_CURVE('',#12458,#12455,#6316,.T.) ;
#15272 = EDGE_CURVE('',#12459,#12460,#6317,.T.) ;
#15273 = EDGE_CURVE('',#12460,#12461,#6318,.T.) ;
#15274 = EDGE_CURVE('',#12461,#12462,#6319,.T.) ;
#15275 = EDGE_CURVE('',#12462,#12459,#10810,.T.) ;
#15276 = EDGE_CURVE('',#12463,#12464,#6320,.T.) ;
#15277 = EDGE_CURVE('',#12464,#12465,#10811,.T.) ;
#15278 = EDGE_CURVE('',#12465,#12466,#6321,.T.) ;
#15279 = EDGE_CURVE('',#12466,#12463,#6322,.T.) ;
#15280 = EDGE_CURVE('',#12467,#12468,#6323,.T.) ;
#15281 = EDGE_CURVE('',#12468,#12469,#6324,.T.) ;
#15282 = EDGE_CURVE('',#12469,#12470,#10812,.T.) ;
#15283 = EDGE_CURVE('',#12470,#12471,#6325,.T.) ;
#15284 = EDGE_CURVE('',#12471,#12467,#6326,.T.) ;
#15285 = EDGE_CURVE('',#12472,#12473,#6327,.T.) ;
#15286 = EDGE_CURVE('',#12473,#12474,#10813,.T.) ;
#15287 = EDGE_CURVE('',#12474,#12472,#6328,.T.) ;
#15288 = EDGE_CURVE('',#12475,#12476,#6329,.T.) ;
#15289 = EDGE_CURVE('',#12476,#12477,#6330,.T.) ;
#15290 = EDGE_CURVE('',#12477,#12478,#6331,.T.) ;
#15291 = EDGE_CURVE('',#12478,#12475,#6332,.T.) ;
#15292 = EDGE_CURVE('',#12479,#12480,#6333,.T.) ;
#15293 = EDGE_CURVE('',#12480,#12481,#10814,.T.) ;
#15294 = EDGE_CURVE('',#12481,#12479,#6334,.T.) ;
#15295 = EDGE_CURVE('',#12482,#12483,#6335,.T.) ;
#15296 = EDGE_CURVE('',#12483,#12484,#6336,.T.) ;
#15297 = EDGE_CURVE('',#12484,#12485,#6337,.T.) ;
#15298 = EDGE_CURVE('',#12485,#12482,#6338,.T.) ;
#15299 = EDGE_CURVE('',#12486,#12487,#6339,.T.) ;
#15300 = EDGE_CURVE('',#12487,#12488,#6340,.T.) ;
#15301 = EDGE_CURVE('',#12488,#12489,#6341,.T.) ;
#15302 = EDGE_CURVE('',#12489,#12486,#6342,.T.) ;
#15303 = EDGE_CURVE('',#12490,#12491,#6343,.T.) ;
#15304 = EDGE_CURVE('',#12491,#12492,#6344,.T.) ;
#15305 = EDGE_CURVE('',#12492,#12493,#6345,.T.) ;
#15306 = EDGE_CURVE('',#12493,#12490,#6346,.T.) ;
#15307 = EDGE_CURVE('',#12494,#12495,#6347,.T.) ;
#15308 = EDGE_CURVE('',#12495,#12496,#6348,.T.) ;
#15309 = EDGE_CURVE('',#12496,#12497,#6349,.T.) ;
#15310 = EDGE_CURVE('',#12497,#12494,#6350,.T.) ;
#15311 = EDGE_CURVE('',#12498,#12499,#6351,.T.) ;
#15312 = EDGE_CURVE('',#12499,#12500,#10815,.T.) ;
#15313 = EDGE_CURVE('',#12500,#12501,#6352,.T.) ;
#15314 = EDGE_CURVE('',#12501,#12498,#6353,.T.) ;
#15315 = EDGE_CURVE('',#12502,#12503,#6354,.T.) ;
#15316 = EDGE_CURVE('',#12503,#12504,#6355,.T.) ;
#15317 = EDGE_CURVE('',#12504,#12505,#6356,.T.) ;
#15318 = EDGE_CURVE('',#12505,#12502,#10816,.T.) ;
#15319 = EDGE_CURVE('',#12506,#12507,#6357,.T.) ;
#15320 = EDGE_CURVE('',#12507,#12508,#6358,.T.) ;
#15321 = EDGE_CURVE('',#12508,#12509,#6359,.T.) ;
#15322 = EDGE_CURVE('',#12509,#12506,#6360,.T.) ;
#15323 = EDGE_CURVE('',#12510,#12511,#6361,.T.) ;
#15324 = EDGE_CURVE('',#12511,#12512,#6362,.T.) ;
#15325 = EDGE_CURVE('',#12512,#12513,#6363,.T.) ;
#15326 = EDGE_CURVE('',#12513,#12510,#6364,.T.) ;
#15327 = EDGE_CURVE('',#12514,#12515,#6365,.T.) ;
#15328 = EDGE_CURVE('',#12515,#12516,#6366,.T.) ;
#15329 = EDGE_CURVE('',#12516,#12517,#6367,.T.) ;
#15330 = EDGE_CURVE('',#12517,#12514,#6368,.T.) ;
#15331 = EDGE_CURVE('',#12518,#12519,#10817,.T.) ;
#15332 = EDGE_CURVE('',#12519,#12520,#6369,.T.) ;
#15333 = EDGE_CURVE('',#12520,#12518,#6370,.T.) ;
#15334 = EDGE_CURVE('',#12521,#12522,#6371,.T.) ;
#15335 = EDGE_CURVE('',#12522,#12523,#6372,.T.) ;
#15336 = EDGE_CURVE('',#12523,#12524,#6373,.T.) ;
#15337 = EDGE_CURVE('',#12524,#12521,#6374,.T.) ;
#15338 = EDGE_CURVE('',#12525,#12526,#6375,.T.) ;
#15339 = EDGE_CURVE('',#12526,#12527,#6376,.T.) ;
#15340 = EDGE_CURVE('',#12527,#12528,#6377,.T.) ;
#15341 = EDGE_CURVE('',#12528,#12525,#6378,.T.) ;
#15342 = EDGE_CURVE('',#12529,#12530,#6379,.T.) ;
#15343 = EDGE_CURVE('',#12530,#12531,#6380,.T.) ;
#15344 = EDGE_CURVE('',#12531,#12532,#6381,.T.) ;
#15345 = EDGE_CURVE('',#12532,#12529,#6382,.T.) ;
#15346 = EDGE_CURVE('',#12533,#12534,#6383,.T.) ;
#15347 = EDGE_CURVE('',#12534,#12535,#6384,.T.) ;
#15348 = EDGE_CURVE('',#12535,#12536,#6385,.T.) ;
#15349 = EDGE_CURVE('',#12536,#12533,#6386,.T.) ;
#15350 = EDGE_CURVE('',#12537,#12538,#6387,.T.) ;
#15351 = EDGE_CURVE('',#12538,#12539,#6388,.T.) ;
#15352 = EDGE_CURVE('',#12539,#12540,#6389,.T.) ;
#15353 = EDGE_CURVE('',#12540,#12537,#6390,.T.) ;
#15354 = EDGE_CURVE('',#12541,#12542,#6391,.T.) ;
#15355 = EDGE_CURVE('',#12542,#12543,#6392,.T.) ;
#15356 = EDGE_CURVE('',#12543,#12544,#6393,.T.) ;
#15357 = EDGE_CURVE('',#12544,#12541,#6394,.T.) ;
#15358 = EDGE_CURVE('',#12545,#12546,#6395,.T.) ;
#15359 = EDGE_CURVE('',#12546,#12547,#6396,.T.) ;
#15360 = EDGE_CURVE('',#12547,#12548,#6397,.T.) ;
#15361 = EDGE_CURVE('',#12548,#12545,#6398,.T.) ;
#15362 = EDGE_CURVE('',#12549,#12550,#6399,.T.) ;
#15363 = EDGE_CURVE('',#12550,#12551,#6400,.T.) ;
#15364 = EDGE_CURVE('',#12551,#12552,#6401,.T.) ;
#15365 = EDGE_CURVE('',#12552,#12549,#6402,.T.) ;
#15366 = EDGE_CURVE('',#12553,#12554,#6403,.T.) ;
#15367 = EDGE_CURVE('',#12554,#12555,#6404,.T.) ;
#15368 = EDGE_CURVE('',#12555,#12556,#6405,.T.) ;
#15369 = EDGE_CURVE('',#12556,#12553,#6406,.T.) ;
#15370 = EDGE_CURVE('',#12557,#12558,#6407,.T.) ;
#15371 = EDGE_CURVE('',#12558,#12559,#10818,.T.) ;
#15372 = EDGE_CURVE('',#12559,#12557,#6408,.T.) ;
#15373 = EDGE_CURVE('',#12560,#12561,#6409,.T.) ;
#15374 = EDGE_CURVE('',#12561,#12562,#10819,.T.) ;
#15375 = EDGE_CURVE('',#12562,#12560,#6410,.T.) ;
#15376 = EDGE_CURVE('',#12563,#12564,#6411,.T.) ;
#15377 = EDGE_CURVE('',#12564,#12565,#10820,.T.) ;
#15378 = EDGE_CURVE('',#12565,#12566,#6412,.T.) ;
#15379 = EDGE_CURVE('',#12566,#12563,#6413,.T.) ;
#15380 = EDGE_CURVE('',#12567,#12568,#6414,.T.) ;
#15381 = EDGE_CURVE('',#12568,#12569,#10821,.T.) ;
#15382 = EDGE_CURVE('',#12569,#12570,#6415,.T.) ;
#15383 = EDGE_CURVE('',#12570,#12567,#6416,.T.) ;
#15384 = EDGE_CURVE('',#12571,#12572,#6417,.T.) ;
#15385 = EDGE_CURVE('',#12572,#12573,#6418,.T.) ;
#15386 = EDGE_CURVE('',#12573,#12574,#6419,.T.) ;
#15387 = EDGE_CURVE('',#12574,#12571,#6420,.T.) ;
#15388 = EDGE_CURVE('',#12129,#12336,#6421,.T.) ;
#15389 = EDGE_CURVE('',#12335,#12130,#6422,.T.) ;
#15390 = EDGE_CURVE('',#12065,#12400,#6423,.T.) ;
#15391 = EDGE_CURVE('',#12180,#12411,#6424,.T.) ;
#15392 = EDGE_CURVE('',#12412,#12184,#6425,.T.) ;
#15393 = EDGE_CURVE('',#12164,#12545,#6426,.T.) ;
#15394 = EDGE_CURVE('',#12546,#12167,#6427,.T.) ;
#15395 = EDGE_CURVE('',#12160,#12549,#6428,.T.) ;
#15396 = EDGE_CURVE('',#12550,#12163,#6429,.T.) ;
#15397 = EDGE_CURVE('',#12406,#12151,#6430,.T.) ;
#15398 = EDGE_CURVE('',#12152,#12405,#6431,.T.) ;
#15399 = EDGE_CURVE('',#12571,#12168,#6432,.T.) ;
#15400 = EDGE_CURVE('',#12169,#12574,#6433,.T.) ;
#15401 = EDGE_CURVE('',#12156,#12553,#6434,.T.) ;
#15402 = EDGE_CURVE('',#12554,#12159,#6435,.T.) ;
#15403 = EDGE_CURVE('',#12382,#12083,#6436,.T.) ;
#15404 = EDGE_CURVE('',#12084,#12381,#6437,.T.) ;
#15405 = EDGE_CURVE('',#12560,#12185,#6438,.T.) ;
#15406 = EDGE_CURVE('',#12186,#12562,#6439,.T.) ;
#15407 = EDGE_CURVE('',#12563,#12176,#6440,.T.) ;
#15408 = EDGE_CURVE('',#12177,#12566,#6441,.T.) ;
#15409 = EDGE_CURVE('',#12567,#12172,#6442,.T.) ;
#15410 = EDGE_CURVE('',#12173,#12570,#6443,.T.) ;
#15411 = EDGE_CURVE('',#12066,#12399,#6444,.T.) ;
#15412 = EDGE_CURVE('',#12085,#12380,#6445,.T.) ;
#15413 = EDGE_CURVE('',#12153,#12557,#6446,.T.) ;
#15414 = EDGE_CURVE('',#12558,#12155,#6447,.T.) ;
#15415 = EDGE_CURVE('',#12154,#12559,#6448,.T.) ;
#15416 = EDGE_CURVE('',#12556,#12157,#6449,.T.) ;
#15417 = EDGE_CURVE('',#12170,#12573,#6450,.T.) ;
#15418 = EDGE_CURVE('',#12398,#12067,#6451,.T.) ;
#15419 = EDGE_CURVE('',#12174,#12569,#6452,.T.) ;
#15420 = EDGE_CURVE('',#12552,#12161,#6453,.T.) ;
#15421 = EDGE_CURVE('',#12178,#12565,#6454,.T.) ;
#15422 = EDGE_CURVE('',#12548,#12165,#6455,.T.) ;
#15423 = EDGE_CURVE('',#12415,#12181,#6456,.T.) ;
#15424 = EDGE_CURVE('',#12561,#12187,#6457,.T.) ;
#15425 = EDGE_CURVE('',#12082,#12383,#6458,.T.) ;
#15426 = EDGE_CURVE('',#12379,#12086,#6459,.T.) ;
#15427 = EDGE_CURVE('',#12341,#12124,#6460,.T.) ;
#15428 = EDGE_CURVE('',#12125,#12340,#6461,.T.) ;
#15429 = EDGE_CURVE('',#12068,#12397,#6462,.T.) ;
#15430 = EDGE_CURVE('',#12126,#12339,#6463,.T.) ;
#15431 = EDGE_CURVE('',#12319,#12409,#6464,.T.) ;
#15432 = EDGE_CURVE('',#12410,#12318,#6465,.T.) ;
#15433 = EDGE_CURVE('',#12150,#12404,#6466,.T.) ;
#15434 = EDGE_CURVE('',#12149,#12403,#6467,.T.) ;
#15435 = EDGE_CURVE('',#12148,#12402,#6468,.T.) ;
#15436 = EDGE_CURVE('',#12525,#12297,#6469,.T.) ;
#15437 = EDGE_CURVE('',#12298,#12528,#6470,.T.) ;
#15438 = EDGE_CURVE('',#12529,#12301,#6471,.T.) ;
#15439 = EDGE_CURVE('',#12302,#12532,#6472,.T.) ;
#15440 = EDGE_CURVE('',#12533,#12305,#6473,.T.) ;
#15441 = EDGE_CURVE('',#12306,#12536,#6474,.T.) ;
#15442 = EDGE_CURVE('',#12537,#12309,#6475,.T.) ;
#15443 = EDGE_CURVE('',#12310,#12540,#6476,.T.) ;
#15444 = EDGE_CURVE('',#12541,#12313,#6477,.T.) ;
#15445 = EDGE_CURVE('',#12314,#12544,#6478,.T.) ;
#15446 = EDGE_CURVE('',#12069,#12396,#6479,.T.) ;
#15447 = EDGE_CURVE('',#12147,#12401,#6480,.T.) ;
#15448 = EDGE_CURVE('',#12171,#12572,#6481,.T.) ;
#15449 = EDGE_CURVE('',#12395,#12070,#6482,.T.) ;
#15450 = EDGE_CURVE('',#12543,#12315,#6483,.T.) ;
#15451 = EDGE_CURVE('',#12539,#12311,#6484,.T.) ;
#15452 = EDGE_CURVE('',#12535,#12307,#6485,.T.) ;
#15453 = EDGE_CURVE('',#12531,#12303,#6486,.T.) ;
#15454 = EDGE_CURVE('',#12338,#12127,#6487,.T.) ;
#15455 = EDGE_CURVE('',#12527,#12299,#6488,.T.) ;
#15456 = EDGE_CURVE('',#12322,#12143,#6489,.T.) ;
#15457 = EDGE_CURVE('',#12144,#12321,#6490,.T.) ;
#15458 = EDGE_CURVE('',#12376,#12089,#6491,.T.) ;
#15459 = EDGE_CURVE('',#12090,#12375,#6492,.T.) ;
#15460 = EDGE_CURVE('',#12166,#12547,#6493,.T.) ;
#15461 = EDGE_CURVE('',#12162,#12551,#6494,.T.) ;
#15462 = EDGE_CURVE('',#12182,#12414,#6495,.T.) ;
#15463 = EDGE_CURVE('',#12158,#12555,#6496,.T.) ;
#15464 = EDGE_CURVE('',#12416,#12281,#6497,.T.) ;
#15465 = EDGE_CURVE('',#12282,#12419,#6498,.T.) ;
#15466 = EDGE_CURVE('',#12285,#12428,#6499,.T.) ;
#15467 = EDGE_CURVE('',#12429,#12288,#6500,.T.) ;
#15468 = EDGE_CURVE('',#12542,#12316,#6501,.T.) ;
#15469 = EDGE_CURVE('',#12289,#12424,#6502,.T.) ;
#15470 = EDGE_CURVE('',#12425,#12292,#6503,.T.) ;
#15471 = EDGE_CURVE('',#12293,#12420,#6504,.T.) ;
#15472 = EDGE_CURVE('',#12421,#12296,#6505,.T.) ;
#15473 = EDGE_CURVE('',#12091,#12374,#6506,.T.) ;
#15474 = EDGE_CURVE('',#12568,#12175,#6507,.T.) ;
#15475 = EDGE_CURVE('',#12294,#12423,#6508,.T.) ;
#15476 = EDGE_CURVE('',#12427,#12290,#6509,.T.) ;
#15477 = EDGE_CURVE('',#12142,#12323,#6510,.T.) ;
#15478 = EDGE_CURVE('',#12183,#12413,#6511,.T.) ;
#15479 = EDGE_CURVE('',#12088,#12377,#6512,.T.) ;
#15480 = EDGE_CURVE('',#12373,#12092,#6513,.T.) ;
#15481 = EDGE_CURVE('',#12431,#12286,#6514,.T.) ;
#15482 = EDGE_CURVE('',#12418,#12283,#6515,.T.) ;
#15483 = EDGE_CURVE('',#12344,#12121,#6516,.T.) ;
#15484 = EDGE_CURVE('',#12122,#12343,#6517,.T.) ;
#15485 = EDGE_CURVE('',#12071,#12394,#6518,.T.) ;
#15486 = EDGE_CURVE('',#12518,#12270,#6519,.T.) ;
#15487 = EDGE_CURVE('',#12271,#12520,#6520,.T.) ;
#15488 = EDGE_CURVE('',#12300,#12526,#6521,.T.) ;
#15489 = EDGE_CURVE('',#12304,#12530,#6522,.T.) ;
#15490 = EDGE_CURVE('',#12308,#12534,#6523,.T.) ;
#15491 = EDGE_CURVE('',#12123,#12342,#6524,.T.) ;
#15492 = EDGE_CURVE('',#12506,#12258,#6525,.T.) ;
#15493 = EDGE_CURVE('',#12259,#12509,#6526,.T.) ;
#15494 = EDGE_CURVE('',#12510,#12262,#6527,.T.) ;
#15495 = EDGE_CURVE('',#12263,#12513,#6528,.T.) ;
#15496 = EDGE_CURVE('',#12514,#12266,#6529,.T.) ;
#15497 = EDGE_CURVE('',#12267,#12517,#6530,.T.) ;
#15498 = EDGE_CURVE('',#12521,#12273,#6531,.T.) ;
#15499 = EDGE_CURVE('',#12274,#12524,#6532,.T.) ;
#15500 = EDGE_CURVE('',#12277,#12502,#6533,.T.) ;
#15501 = EDGE_CURVE('',#12503,#12280,#6534,.T.) ;
#15502 = EDGE_CURVE('',#12072,#12393,#6535,.T.) ;
#15503 = EDGE_CURVE('',#12312,#12538,#6536,.T.) ;
#15504 = EDGE_CURVE('',#12295,#12422,#6537,.T.) ;
#15505 = EDGE_CURVE('',#12392,#12073,#6538,.T.) ;
#15506 = EDGE_CURVE('',#12272,#12519,#6539,.T.) ;
#15507 = EDGE_CURVE('',#12505,#12278,#6540,.T.) ;
#15508 = EDGE_CURVE('',#12523,#12275,#6541,.T.) ;
#15509 = EDGE_CURVE('',#12516,#12268,#6542,.T.) ;
#15510 = EDGE_CURVE('',#12512,#12264,#6543,.T.) ;
#15511 = EDGE_CURVE('',#12508,#12260,#6544,.T.) ;
#15512 = EDGE_CURVE('',#12325,#12140,#6545,.T.) ;
#15513 = EDGE_CURVE('',#12141,#12324,#6546,.T.) ;
#15514 = EDGE_CURVE('',#12242,#12498,#6547,.T.) ;
#15515 = EDGE_CURVE('',#12499,#12245,#6548,.T.) ;
#15516 = EDGE_CURVE('',#12246,#12443,#6549,.T.) ;
#15517 = EDGE_CURVE('',#12444,#12249,#6550,.T.) ;
#15518 = EDGE_CURVE('',#12250,#12439,#6551,.T.) ;
#15519 = EDGE_CURVE('',#12440,#12253,#6552,.T.) ;
#15520 = EDGE_CURVE('',#12522,#12276,#6553,.T.) ;
#15521 = EDGE_CURVE('',#12254,#12435,#6554,.T.) ;
#15522 = EDGE_CURVE('',#12436,#12257,#6555,.T.) ;
#15523 = EDGE_CURVE('',#12093,#12372,#6556,.T.) ;
#15524 = EDGE_CURVE('',#12432,#12239,#6557,.T.) ;
#15525 = EDGE_CURVE('',#12240,#12434,#6558,.T.) ;
#15526 = EDGE_CURVE('',#12284,#12417,#6559,.T.) ;
#15527 = EDGE_CURVE('',#12287,#12430,#6560,.T.) ;
#15528 = EDGE_CURVE('',#12291,#12426,#6561,.T.) ;
#15529 = EDGE_CURVE('',#12094,#12371,#6562,.T.) ;
#15530 = EDGE_CURVE('',#12564,#12179,#6563,.T.) ;
#15531 = EDGE_CURVE('',#12255,#12438,#6564,.T.) ;
#15532 = EDGE_CURVE('',#12407,#12145,#6565,.T.) ;
#15533 = EDGE_CURVE('',#12139,#12326,#6566,.T.) ;
#15534 = EDGE_CURVE('',#12442,#12251,#6567,.T.) ;
#15535 = EDGE_CURVE('',#12446,#12247,#6568,.T.) ;
#15536 = EDGE_CURVE('',#12501,#12243,#6569,.T.) ;
#15537 = EDGE_CURVE('',#12433,#12241,#6570,.T.) ;
#15538 = EDGE_CURVE('',#12370,#12095,#6571,.T.) ;
#15539 = EDGE_CURVE('',#12074,#12391,#6572,.T.) ;
#15540 = EDGE_CURVE('',#12279,#12504,#6573,.T.) ;
#15541 = EDGE_CURVE('',#12261,#12507,#6574,.T.) ;
#15542 = EDGE_CURVE('',#12120,#12345,#6575,.T.) ;
#15543 = EDGE_CURVE('',#12119,#12346,#6576,.T.) ;
#15544 = EDGE_CURVE('',#12265,#12511,#6577,.T.) ;
#15545 = EDGE_CURVE('',#12269,#12515,#6578,.T.) ;
#15546 = EDGE_CURVE('',#12348,#12117,#6579,.T.) ;
#15547 = EDGE_CURVE('',#12118,#12347,#6580,.T.) ;
#15548 = EDGE_CURVE('',#12455,#12200,#6581,.T.) ;
#15549 = EDGE_CURVE('',#12201,#12458,#6582,.T.) ;
#15550 = EDGE_CURVE('',#12451,#12196,#6583,.T.) ;
#15551 = EDGE_CURVE('',#12197,#12454,#6584,.T.) ;
#15552 = EDGE_CURVE('',#12188,#12459,#6585,.T.) ;
#15553 = EDGE_CURVE('',#12460,#12191,#6586,.T.) ;
#15554 = EDGE_CURVE('',#12447,#12192,#6587,.T.) ;
#15555 = EDGE_CURVE('',#12193,#12450,#6588,.T.) ;
#15556 = EDGE_CURVE('',#12076,#12389,#6589,.T.) ;
#15557 = EDGE_CURVE('',#12075,#12390,#6590,.T.) ;
#15558 = EDGE_CURVE('',#12256,#12437,#6591,.T.) ;
#15559 = EDGE_CURVE('',#12448,#12195,#6592,.T.) ;
#15560 = EDGE_CURVE('',#12388,#12077,#6593,.T.) ;
#15561 = EDGE_CURVE('',#12449,#12194,#6594,.T.) ;
#15562 = EDGE_CURVE('',#12116,#12349,#6595,.T.) ;
#15563 = EDGE_CURVE('',#12462,#12189,#6596,.T.) ;
#15564 = EDGE_CURVE('',#12453,#12198,#6597,.T.) ;
#15565 = EDGE_CURVE('',#12457,#12202,#6598,.T.) ;
#15566 = EDGE_CURVE('',#12096,#12369,#6599,.T.) ;
#15567 = EDGE_CURVE('',#12244,#12500,#6600,.T.) ;
#15568 = EDGE_CURVE('',#12248,#12445,#6601,.T.) ;
#15569 = EDGE_CURVE('',#12138,#12327,#6602,.T.) ;
#15570 = EDGE_CURVE('',#12252,#12441,#6603,.T.) ;
#15571 = EDGE_CURVE('',#12329,#12136,#6604,.T.) ;
#15572 = EDGE_CURVE('',#12137,#12328,#6605,.T.) ;
#15573 = EDGE_CURVE('',#12098,#12367,#6606,.T.) ;
#15574 = EDGE_CURVE('',#12097,#12368,#6607,.T.) ;
#15575 = EDGE_CURVE('',#12212,#12463,#6608,.T.) ;
#15576 = EDGE_CURVE('',#12464,#12215,#6609,.T.) ;
#15577 = EDGE_CURVE('',#12208,#12490,#6610,.T.) ;
#15578 = EDGE_CURVE('',#12491,#12211,#6611,.T.) ;
#15579 = EDGE_CURVE('',#12204,#12494,#6612,.T.) ;
#15580 = EDGE_CURVE('',#12495,#12207,#6613,.T.) ;
#15581 = EDGE_CURVE('',#12205,#12497,#6614,.T.) ;
#15582 = EDGE_CURVE('',#12493,#12209,#6615,.T.) ;
#15583 = EDGE_CURVE('',#12408,#12146,#6616,.T.) ;
#15584 = EDGE_CURVE('',#12466,#12213,#6617,.T.) ;
#15585 = EDGE_CURVE('',#12214,#12465,#6618,.T.) ;
#15586 = EDGE_CURVE('',#12366,#12099,#6619,.T.) ;
#15587 = EDGE_CURVE('',#12078,#12387,#6620,.T.) ;
#15588 = EDGE_CURVE('',#12351,#12114,#6621,.T.) ;
#15589 = EDGE_CURVE('',#12115,#12350,#6622,.T.) ;
#15590 = EDGE_CURVE('',#12479,#12224,#6623,.T.) ;
#15591 = EDGE_CURVE('',#12225,#12481,#6624,.T.) ;
#15592 = EDGE_CURVE('',#12482,#12216,#6625,.T.) ;
#15593 = EDGE_CURVE('',#12217,#12485,#6626,.T.) ;
#15594 = EDGE_CURVE('',#12079,#12386,#6627,.T.) ;
#15595 = EDGE_CURVE('',#12486,#12220,#6628,.T.) ;
#15596 = EDGE_CURVE('',#12221,#12489,#6629,.T.) ;
#15597 = EDGE_CURVE('',#12190,#12461,#6630,.T.) ;
#15598 = EDGE_CURVE('',#12203,#12456,#6631,.T.) ;
#15599 = EDGE_CURVE('',#12199,#12452,#6632,.T.) ;
#15600 = EDGE_CURVE('',#12206,#12496,#6633,.T.) ;
#15601 = EDGE_CURVE('',#12488,#12222,#6634,.T.) ;
#15602 = EDGE_CURVE('',#12385,#12080,#6635,.T.) ;
#15603 = EDGE_CURVE('',#12484,#12218,#6636,.T.) ;
#15604 = EDGE_CURVE('',#12113,#12352,#6637,.T.) ;
#15605 = EDGE_CURVE('',#12480,#12226,#6638,.T.) ;
#15606 = EDGE_CURVE('',#12100,#12365,#6639,.T.) ;
#15607 = EDGE_CURVE('',#12210,#12492,#6640,.T.) ;
#15608 = EDGE_CURVE('',#12101,#12364,#6641,.T.) ;
#15609 = EDGE_CURVE('',#12232,#12472,#6642,.T.) ;
#15610 = EDGE_CURVE('',#12473,#12234,#6643,.T.) ;
#15611 = EDGE_CURVE('',#12332,#12133,#6644,.T.) ;
#15612 = EDGE_CURVE('',#12134,#12331,#6645,.T.) ;
#15613 = EDGE_CURVE('',#12235,#12475,#6646,.T.) ;
#15614 = EDGE_CURVE('',#12476,#12238,#6647,.T.) ;
#15615 = EDGE_CURVE('',#12487,#12223,#6648,.T.) ;
#15616 = EDGE_CURVE('',#12135,#12330,#6649,.T.) ;
#15617 = EDGE_CURVE('',#12236,#12478,#6650,.T.) ;
#15618 = EDGE_CURVE('',#12132,#12333,#6651,.T.) ;
#15619 = EDGE_CURVE('',#12233,#12474,#6652,.T.) ;
#15620 = EDGE_CURVE('',#12363,#12102,#6653,.T.) ;
#15621 = EDGE_CURVE('',#12081,#12384,#6654,.T.) ;
#15622 = EDGE_CURVE('',#12354,#12111,#6655,.T.) ;
#15623 = EDGE_CURVE('',#12112,#12353,#6656,.T.) ;
#15624 = EDGE_CURVE('',#12467,#12227,#6657,.T.) ;
#15625 = EDGE_CURVE('',#12228,#12471,#6658,.T.) ;
#15626 = EDGE_CURVE('',#12219,#12483,#6659,.T.) ;
#15627 = EDGE_CURVE('',#12237,#12477,#6660,.T.) ;
#15628 = EDGE_CURVE('',#12229,#12470,#6661,.T.) ;
#15629 = EDGE_CURVE('',#12110,#12355,#6662,.T.) ;
#15630 = EDGE_CURVE('',#12103,#12362,#6663,.T.) ;
#15631 = EDGE_CURVE('',#12131,#12334,#6664,.T.) ;
#15632 = EDGE_CURVE('',#12104,#12361,#6665,.T.) ;
#15633 = EDGE_CURVE('',#12468,#12231,#6666,.T.) ;
#15634 = EDGE_CURVE('',#12469,#12230,#6667,.T.) ;
#15635 = EDGE_CURVE('',#12360,#12105,#6668,.T.) ;
#15636 = EDGE_CURVE('',#12087,#12378,#6669,.T.) ;
#15637 = EDGE_CURVE('',#12106,#12359,#6670,.T.) ;
#15638 = EDGE_CURVE('',#12107,#12358,#6671,.T.) ;
#15639 = EDGE_CURVE('',#12357,#12108,#6672,.T.) ;
#15640 = EDGE_CURVE('',#12109,#12356,#6673,.T.) ;
#15641 = EDGE_CURVE('',#12128,#12337,#6674,.T.) ;
#15642 = EDGE_CURVE('',#12575,#12576,#10822,.T.) ;
#15643 = EDGE_CURVE('',#12576,#12575,#10823,.T.) ;
#15644 = EDGE_CURVE('',#12577,#12578,#10824,.T.) ;
#15645 = EDGE_CURVE('',#12578,#12577,#10825,.T.) ;
#15646 = EDGE_CURVE('',#12579,#12580,#10826,.T.) ;
#15647 = EDGE_CURVE('',#12580,#12579,#10827,.T.) ;
#15648 = EDGE_CURVE('',#12581,#12582,#10828,.T.) ;
#15649 = EDGE_CURVE('',#12582,#12581,#10829,.T.) ;
#15650 = EDGE_CURVE('',#12583,#12584,#10830,.T.) ;
#15651 = EDGE_CURVE('',#12584,#12583,#10831,.T.) ;
#15652 = EDGE_CURVE('',#12585,#12586,#10832,.T.) ;
#15653 = EDGE_CURVE('',#12586,#12585,#10833,.T.) ;
#15654 = EDGE_CURVE('',#12587,#12588,#10834,.T.) ;
#15655 = EDGE_CURVE('',#12588,#12587,#10835,.T.) ;
#15656 = EDGE_CURVE('',#12589,#12590,#10836,.T.) ;
#15657 = EDGE_CURVE('',#12590,#12591,#10837,.T.) ;
#15658 = EDGE_CURVE('',#12591,#12589,#10838,.T.) ;
#15659 = EDGE_CURVE('',#12592,#12593,#10839,.T.) ;
#15660 = EDGE_CURVE('',#12593,#12594,#10840,.T.) ;
#15661 = EDGE_CURVE('',#12594,#12595,#10841,.T.) ;
#15662 = EDGE_CURVE('',#12595,#12592,#10842,.T.) ;
#15663 = EDGE_CURVE('',#12596,#12597,#10843,.T.) ;
#15664 = EDGE_CURVE('',#12597,#12598,#10844,.T.) ;
#15665 = EDGE_CURVE('',#12598,#12599,#10845,.T.) ;
#15666 = EDGE_CURVE('',#12599,#12596,#10846,.T.) ;
#15667 = EDGE_CURVE('',#12600,#12601,#10847,.T.) ;
#15668 = EDGE_CURVE('',#12601,#12602,#10848,.T.) ;
#15669 = EDGE_CURVE('',#12602,#12603,#10849,.T.) ;
#15670 = EDGE_CURVE('',#12603,#12600,#10850,.T.) ;
#15671 = EDGE_CURVE('',#12604,#12605,#10851,.T.) ;
#15672 = EDGE_CURVE('',#12605,#12606,#10852,.T.) ;
#15673 = EDGE_CURVE('',#12606,#12607,#10853,.T.) ;
#15674 = EDGE_CURVE('',#12607,#12604,#10854,.T.) ;
#15675 = EDGE_CURVE('',#12608,#12609,#10855,.T.) ;
#15676 = EDGE_CURVE('',#12609,#12610,#10856,.T.) ;
#15677 = EDGE_CURVE('',#12610,#12611,#10857,.T.) ;
#15678 = EDGE_CURVE('',#12611,#12608,#10858,.T.) ;
#15679 = EDGE_CURVE('',#12612,#12613,#10859,.T.) ;
#15680 = EDGE_CURVE('',#12613,#12614,#10860,.T.) ;
#15681 = EDGE_CURVE('',#12614,#12615,#10861,.T.) ;
#15682 = EDGE_CURVE('',#12615,#12612,#10862,.T.) ;
#15683 = EDGE_CURVE('',#12616,#12617,#10863,.T.) ;
#15684 = EDGE_CURVE('',#12617,#12618,#10864,.T.) ;
#15685 = EDGE_CURVE('',#12618,#12619,#10865,.T.) ;
#15686 = EDGE_CURVE('',#12619,#12616,#10866,.T.) ;
#15687 = EDGE_CURVE('',#12620,#12621,#10867,.T.) ;
#15688 = EDGE_CURVE('',#12621,#12622,#10868,.T.) ;
#15689 = EDGE_CURVE('',#12622,#12623,#10869,.T.) ;
#15690 = EDGE_CURVE('',#12623,#12620,#10870,.T.) ;
#15691 = EDGE_CURVE('',#12624,#12625,#10871,.T.) ;
#15692 = EDGE_CURVE('',#12625,#12626,#10872,.T.) ;
#15693 = EDGE_CURVE('',#12626,#12627,#10873,.T.) ;
#15694 = EDGE_CURVE('',#12627,#12624,#10874,.T.) ;
#15695 = EDGE_CURVE('',#12628,#12629,#10875,.T.) ;
#15696 = EDGE_CURVE('',#12629,#12630,#10876,.T.) ;
#15697 = EDGE_CURVE('',#12630,#12631,#10877,.T.) ;
#15698 = EDGE_CURVE('',#12631,#12628,#10878,.T.) ;
#15699 = EDGE_CURVE('',#12632,#12633,#10879,.T.) ;
#15700 = EDGE_CURVE('',#12633,#12634,#10880,.T.) ;
#15701 = EDGE_CURVE('',#12634,#12635,#10881,.T.) ;
#15702 = EDGE_CURVE('',#12635,#12632,#10882,.T.) ;
#15703 = EDGE_CURVE('',#12636,#12637,#10883,.T.) ;
#15704 = EDGE_CURVE('',#12637,#12638,#10884,.T.) ;
#15705 = EDGE_CURVE('',#12638,#12639,#10885,.T.) ;
#15706 = EDGE_CURVE('',#12639,#12636,#10886,.T.) ;
#15707 = EDGE_CURVE('',#12640,#12641,#10887,.T.) ;
#15708 = EDGE_CURVE('',#12641,#12642,#10888,.T.) ;
#15709 = EDGE_CURVE('',#12642,#12643,#10889,.T.) ;
#15710 = EDGE_CURVE('',#12643,#12640,#10890,.T.) ;
#15711 = EDGE_CURVE('',#12644,#12645,#10891,.T.) ;
#15712 = EDGE_CURVE('',#12645,#12646,#10892,.T.) ;
#15713 = EDGE_CURVE('',#12646,#12644,#10893,.T.) ;
#15714 = EDGE_CURVE('',#12647,#12648,#10894,.T.) ;
#15715 = EDGE_CURVE('',#12648,#12647,#10895,.T.) ;
#15716 = EDGE_CURVE('',#12649,#12650,#10896,.T.) ;
#15717 = EDGE_CURVE('',#12650,#12649,#10897,.T.) ;
#15718 = EDGE_CURVE('',#12651,#12652,#10898,.T.) ;
#15719 = EDGE_CURVE('',#12652,#12651,#10899,.T.) ;
#15720 = EDGE_CURVE('',#12653,#12654,#10900,.T.) ;
#15721 = EDGE_CURVE('',#12654,#12653,#10901,.T.) ;
#15722 = EDGE_CURVE('',#12655,#12656,#10902,.T.) ;
#15723 = EDGE_CURVE('',#12656,#12655,#10903,.T.) ;
#15724 = EDGE_CURVE('',#12657,#12658,#10904,.T.) ;
#15725 = EDGE_CURVE('',#12658,#12657,#10905,.T.) ;
#15726 = EDGE_CURVE('',#12576,#12659,#362,.T.) ;
#15727 = EDGE_CURVE('',#12659,#12575,#363,.T.) ;
#15728 = EDGE_CURVE('',#12659,#12660,#6675,.T.) ;
#15729 = EDGE_CURVE('',#12578,#12660,#364,.T.) ;
#15730 = EDGE_CURVE('',#12660,#12577,#365,.T.) ;
#15731 = EDGE_CURVE('',#12660,#12661,#6676,.T.) ;
#15732 = EDGE_CURVE('',#12580,#12661,#366,.T.) ;
#15733 = EDGE_CURVE('',#12661,#12579,#367,.T.) ;
#15734 = EDGE_CURVE('',#12661,#12662,#6677,.T.) ;
#15735 = EDGE_CURVE('',#12582,#12662,#368,.T.) ;
#15736 = EDGE_CURVE('',#12662,#12581,#369,.T.) ;
#15737 = EDGE_CURVE('',#12662,#12663,#6678,.T.) ;
#15738 = EDGE_CURVE('',#12584,#12663,#370,.T.) ;
#15739 = EDGE_CURVE('',#12663,#12583,#371,.T.) ;
#15740 = EDGE_CURVE('',#12663,#12664,#6679,.T.) ;
#15741 = EDGE_CURVE('',#12586,#12664,#372,.T.) ;
#15742 = EDGE_CURVE('',#12664,#12585,#373,.T.) ;
#15743 = EDGE_CURVE('',#12664,#12665,#6680,.T.) ;
#15744 = EDGE_CURVE('',#12588,#12665,#374,.T.) ;
#15745 = EDGE_CURVE('',#12665,#12587,#375,.T.) ;
#15746 = EDGE_CURVE('',#12665,#12666,#6681,.T.) ;
#15747 = EDGE_CURVE('',#12590,#12666,#376,.T.) ;
#15748 = EDGE_CURVE('',#12666,#12589,#377,.T.) ;
#15749 = EDGE_CURVE('',#12591,#12593,#6682,.T.) ;
#15750 = EDGE_CURVE('',#12594,#12592,#378,.T.) ;
#15751 = EDGE_CURVE('',#12595,#12597,#6683,.T.) ;
#15752 = EDGE_CURVE('',#12598,#12596,#379,.T.) ;
#15753 = EDGE_CURVE('',#12599,#12601,#6684,.T.) ;
#15754 = EDGE_CURVE('',#12602,#12600,#380,.T.) ;
#15755 = EDGE_CURVE('',#12603,#12605,#6685,.T.) ;
#15756 = EDGE_CURVE('',#12606,#12604,#381,.T.) ;
#15757 = EDGE_CURVE('',#12607,#12609,#6686,.T.) ;
#15758 = EDGE_CURVE('',#12610,#12608,#382,.T.) ;
#15759 = EDGE_CURVE('',#12611,#12613,#6687,.T.) ;
#15760 = EDGE_CURVE('',#12614,#12612,#383,.T.) ;
#15761 = EDGE_CURVE('',#12615,#12617,#6688,.T.) ;
#15762 = EDGE_CURVE('',#12618,#12616,#384,.T.) ;
#15763 = EDGE_CURVE('',#12619,#12621,#6689,.T.) ;
#15764 = EDGE_CURVE('',#12622,#12620,#385,.T.) ;
#15765 = EDGE_CURVE('',#12623,#12625,#6690,.T.) ;
#15766 = EDGE_CURVE('',#12626,#12624,#386,.T.) ;
#15767 = EDGE_CURVE('',#12627,#12629,#6691,.T.) ;
#15768 = EDGE_CURVE('',#12630,#12628,#387,.T.) ;
#15769 = EDGE_CURVE('',#12631,#12633,#6692,.T.) ;
#15770 = EDGE_CURVE('',#12634,#12632,#388,.T.) ;
#15771 = EDGE_CURVE('',#12635,#12637,#6693,.T.) ;
#15772 = EDGE_CURVE('',#12638,#12636,#389,.T.) ;
#15773 = EDGE_CURVE('',#12639,#12641,#6694,.T.) ;
#15774 = EDGE_CURVE('',#12642,#12640,#390,.T.) ;
#15775 = EDGE_CURVE('',#12643,#12645,#6695,.T.) ;
#15776 = EDGE_CURVE('',#12667,#12644,#391,.T.) ;
#15777 = EDGE_CURVE('',#12646,#12667,#392,.T.) ;
#15778 = EDGE_CURVE('',#12667,#12668,#6696,.T.) ;
#15779 = EDGE_CURVE('',#12648,#12668,#393,.T.) ;
#15780 = EDGE_CURVE('',#12668,#12647,#394,.T.) ;
#15781 = EDGE_CURVE('',#12668,#12669,#6697,.T.) ;
#15782 = EDGE_CURVE('',#12650,#12669,#395,.T.) ;
#15783 = EDGE_CURVE('',#12669,#12649,#396,.T.) ;
#15784 = EDGE_CURVE('',#12669,#12670,#6698,.T.) ;
#15785 = EDGE_CURVE('',#12652,#12670,#397,.T.) ;
#15786 = EDGE_CURVE('',#12670,#12651,#398,.T.) ;
#15787 = EDGE_CURVE('',#12670,#12671,#6699,.T.) ;
#15788 = EDGE_CURVE('',#12654,#12671,#399,.T.) ;
#15789 = EDGE_CURVE('',#12671,#12653,#400,.T.) ;
#15790 = EDGE_CURVE('',#12671,#12672,#6700,.T.) ;
#15791 = EDGE_CURVE('',#12656,#12672,#401,.T.) ;
#15792 = EDGE_CURVE('',#12672,#12655,#402,.T.) ;
#15793 = EDGE_CURVE('',#12672,#12673,#6701,.T.) ;
#15794 = EDGE_CURVE('',#12658,#12673,#403,.T.) ;
#15795 = EDGE_CURVE('',#12673,#12657,#404,.T.) ;
#15796 = EDGE_CURVE('',#12673,#12659,#6702,.T.) ;
#15797 = EDGE_CURVE('',#12674,#12674,#10906,.T.) ;
#15798 = EDGE_CURVE('',#12674,#12675,#6703,.T.) ;
#15799 = EDGE_CURVE('',#12675,#12675,#10907,.T.) ;
#15800 = EDGE_CURVE('',#12676,#12676,#10908,.T.) ;
#15801 = EDGE_CURVE('',#12676,#12677,#6704,.T.) ;
#15802 = EDGE_CURVE('',#12677,#12677,#10909,.T.) ;
#15803 = EDGE_CURVE('',#12678,#12678,#10910,.T.) ;
#15804 = EDGE_CURVE('',#12678,#12679,#6705,.T.) ;
#15805 = EDGE_CURVE('',#12679,#12679,#10911,.T.) ;
#15806 = EDGE_CURVE('',#12680,#12680,#10912,.T.) ;
#15807 = EDGE_CURVE('',#12680,#12681,#6706,.T.) ;
#15808 = EDGE_CURVE('',#12681,#12681,#10913,.T.) ;
#15809 = EDGE_CURVE('',#12682,#12682,#10914,.T.) ;
#15810 = EDGE_CURVE('',#12682,#12683,#6707,.T.) ;
#15811 = EDGE_CURVE('',#12683,#12683,#10915,.T.) ;
#15812 = EDGE_CURVE('',#12684,#12684,#10916,.T.) ;
#15813 = EDGE_CURVE('',#12684,#12685,#6708,.T.) ;
#15814 = EDGE_CURVE('',#12685,#12685,#10917,.T.) ;
#15815 = EDGE_CURVE('',#12686,#12687,#6709,.T.) ;
#15816 = EDGE_CURVE('',#12687,#12688,#10918,.T.) ;
#15817 = EDGE_CURVE('',#12688,#12689,#6710,.T.) ;
#15818 = EDGE_CURVE('',#12689,#12686,#10919,.T.) ;
#15819 = EDGE_CURVE('',#12690,#12691,#6711,.T.) ;
#15820 = EDGE_CURVE('',#12690,#12692,#6712,.T.) ;
#15821 = EDGE_CURVE('',#12692,#12693,#6713,.T.) ;
#15822 = EDGE_CURVE('',#12693,#12691,#6714,.T.) ;
#15823 = EDGE_CURVE('',#12689,#12693,#6715,.T.) ;
#15824 = EDGE_CURVE('',#12692,#12694,#6716,.T.) ;
#15825 = EDGE_CURVE('',#12694,#12695,#6717,.T.) ;
#15826 = EDGE_CURVE('',#12695,#12686,#6718,.T.) ;
#15827 = EDGE_CURVE('',#12694,#12696,#6719,.T.) ;
#15828 = EDGE_CURVE('',#12696,#12697,#6720,.T.) ;
#15829 = EDGE_CURVE('',#12697,#12695,#6721,.T.) ;
#15830 = EDGE_CURVE('',#12691,#12688,#6722,.T.) ;
#15831 = EDGE_CURVE('',#12696,#12690,#6723,.T.) ;
#15832 = EDGE_CURVE('',#12687,#12697,#6724,.T.) ;
#15833 = EDGE_CURVE('',#12698,#12698,#10920,.T.) ;
#15834 = EDGE_CURVE('',#12698,#12699,#6725,.T.) ;
#15835 = EDGE_CURVE('',#12699,#12699,#10921,.T.) ;
#15836 = EDGE_CURVE('',#12700,#12700,#10922,.T.) ;
#15837 = EDGE_CURVE('',#12700,#12701,#6726,.T.) ;
#15838 = EDGE_CURVE('',#12701,#12701,#10923,.T.) ;
#15839 = EDGE_CURVE('',#12702,#12703,#6727,.T.) ;
#15840 = EDGE_CURVE('',#12703,#12704,#10924,.T.) ;
#15841 = EDGE_CURVE('',#12704,#12705,#6728,.T.) ;
#15842 = EDGE_CURVE('',#12705,#12702,#10925,.T.) ;
#15843 = EDGE_CURVE('',#12706,#12707,#6729,.T.) ;
#15844 = EDGE_CURVE('',#12706,#12708,#6730,.T.) ;
#15845 = EDGE_CURVE('',#12708,#12709,#6731,.T.) ;
#15846 = EDGE_CURVE('',#12709,#12707,#6732,.T.) ;
#15847 = EDGE_CURVE('',#12705,#12709,#6733,.T.) ;
#15848 = EDGE_CURVE('',#12708,#12710,#6734,.T.) ;
#15849 = EDGE_CURVE('',#12710,#12711,#6735,.T.) ;
#15850 = EDGE_CURVE('',#12711,#12702,#6736,.T.) ;
#15851 = EDGE_CURVE('',#12710,#12712,#6737,.T.) ;
#15852 = EDGE_CURVE('',#12712,#12713,#6738,.T.) ;
#15853 = EDGE_CURVE('',#12713,#12711,#6739,.T.) ;
#15854 = EDGE_CURVE('',#12707,#12704,#6740,.T.) ;
#15855 = EDGE_CURVE('',#12712,#12706,#6741,.T.) ;
#15856 = EDGE_CURVE('',#12703,#12713,#6742,.T.) ;
#15857 = EDGE_CURVE('',#12714,#12714,#10926,.T.) ;
#15858 = EDGE_CURVE('',#12714,#12715,#6743,.T.) ;
#15859 = EDGE_CURVE('',#12715,#12715,#10927,.T.) ;
#15860 = EDGE_CURVE('',#12716,#12716,#10928,.T.) ;
#15861 = EDGE_CURVE('',#12716,#12717,#6744,.T.) ;
#15862 = EDGE_CURVE('',#12717,#12717,#10929,.T.) ;
#15863 = EDGE_CURVE('',#12718,#12718,#10930,.T.) ;
#15864 = EDGE_CURVE('',#12718,#12719,#6745,.T.) ;
#15865 = EDGE_CURVE('',#12719,#12719,#10931,.T.) ;
#15866 = EDGE_CURVE('',#12720,#12720,#10932,.T.) ;
#15867 = EDGE_CURVE('',#12720,#12721,#6746,.T.) ;
#15868 = EDGE_CURVE('',#12721,#12721,#10933,.T.) ;
#15869 = EDGE_CURVE('',#12722,#12723,#6747,.T.) ;
#15870 = EDGE_CURVE('',#12723,#12724,#6748,.T.) ;
#15871 = EDGE_CURVE('',#12724,#12725,#6749,.T.) ;
#15872 = EDGE_CURVE('',#12726,#12725,#6750,.T.) ;
#15873 = EDGE_CURVE('',#12726,#12722,#6751,.T.) ;
#15874 = EDGE_CURVE('',#12727,#12727,#10934,.T.) ;
#15875 = EDGE_CURVE('',#12728,#12728,#10935,.T.) ;
#15876 = EDGE_CURVE('',#12728,#12729,#6752,.T.) ;
#15877 = EDGE_CURVE('',#12729,#12729,#10936,.T.) ;
#15878 = EDGE_CURVE('',#12730,#12730,#10937,.T.) ;
#15879 = EDGE_CURVE('',#12730,#12727,#6753,.T.) ;
#15880 = EDGE_CURVE('',#12731,#12732,#6754,.T.) ;
#15881 = EDGE_CURVE('',#12731,#12733,#6755,.T.) ;
#15882 = EDGE_CURVE('',#12734,#12733,#6756,.T.) ;
#15883 = EDGE_CURVE('',#12732,#12734,#6757,.T.) ;
#15884 = EDGE_CURVE('',#12732,#12735,#6758,.T.) ;
#15885 = EDGE_CURVE('',#12736,#12734,#6759,.T.) ;
#15886 = EDGE_CURVE('',#12735,#12736,#6760,.T.) ;
#15887 = EDGE_CURVE('',#12735,#12737,#6761,.T.) ;
#15888 = EDGE_CURVE('',#12738,#12736,#6762,.T.) ;
#15889 = EDGE_CURVE('',#12737,#12738,#6763,.T.) ;
#15890 = EDGE_CURVE('',#12737,#12731,#6764,.T.) ;
#15891 = EDGE_CURVE('',#12733,#12738,#6765,.T.) ;
#15892 = EDGE_CURVE('',#12739,#12740,#6766,.T.) ;
#15893 = EDGE_CURVE('',#12740,#12741,#6767,.T.) ;
#15894 = EDGE_CURVE('',#12741,#12742,#6768,.T.) ;
#15895 = EDGE_CURVE('',#12742,#12739,#6769,.T.) ;
#15896 = EDGE_CURVE('',#12743,#12742,#6770,.T.) ;
#15897 = EDGE_CURVE('',#12744,#12741,#6771,.T.) ;
#15898 = EDGE_CURVE('',#12743,#12744,#6772,.T.) ;
#15899 = EDGE_CURVE('',#12745,#12740,#6773,.T.) ;
#15900 = EDGE_CURVE('',#12746,#12739,#6774,.T.) ;
#15901 = EDGE_CURVE('',#12745,#12746,#6775,.T.) ;
#15902 = EDGE_CURVE('',#12744,#12747,#6776,.T.) ;
#15903 = EDGE_CURVE('',#12748,#12747,#6777,.T.) ;
#15904 = EDGE_CURVE('',#12749,#12748,#6778,.T.) ;
#15905 = EDGE_CURVE('',#12749,#12743,#6779,.T.) ;
#15906 = EDGE_CURVE('',#12750,#12751,#6780,.T.) ;
#15907 = EDGE_CURVE('',#12750,#12752,#6781,.T.) ;
#15908 = EDGE_CURVE('',#12752,#12753,#6782,.T.) ;
#15909 = EDGE_CURVE('',#12751,#12753,#6783,.T.) ;
#15910 = EDGE_CURVE('',#12754,#12754,#10938,.T.) ;
#15911 = EDGE_CURVE('',#12755,#12756,#6784,.T.) ;
#15912 = EDGE_CURVE('',#12756,#12757,#6785,.T.) ;
#15913 = EDGE_CURVE('',#12757,#12758,#6786,.T.) ;
#15914 = EDGE_CURVE('',#12758,#12755,#6787,.T.) ;
#15915 = EDGE_CURVE('',#12759,#12750,#10939,.T.) ;
#15916 = EDGE_CURVE('',#12760,#12759,#6788,.T.) ;
#15917 = EDGE_CURVE('',#12760,#12761,#6789,.T.) ;
#15918 = EDGE_CURVE('',#12762,#12761,#6790,.T.) ;
#15919 = EDGE_CURVE('',#12755,#12762,#6791,.T.) ;
#15920 = EDGE_CURVE('',#12763,#12758,#6792,.T.) ;
#15921 = EDGE_CURVE('',#12764,#12763,#6793,.T.) ;
#15922 = EDGE_CURVE('',#12764,#12752,#6794,.T.) ;
#15923 = EDGE_CURVE('',#12765,#12766,#6795,.T.) ;
#15924 = EDGE_CURVE('',#12767,#12765,#6796,.T.) ;
#15925 = EDGE_CURVE('',#12767,#12757,#6797,.T.) ;
#15926 = EDGE_CURVE('',#12756,#12768,#6798,.T.) ;
#15927 = EDGE_CURVE('',#12769,#12768,#6799,.T.) ;
#15928 = EDGE_CURVE('',#12770,#12769,#6800,.T.) ;
#15929 = EDGE_CURVE('',#12766,#12770,#6801,.T.) ;
#15930 = EDGE_CURVE('',#12763,#12767,#6802,.T.) ;
#15931 = EDGE_CURVE('',#12766,#12771,#6803,.T.) ;
#15932 = EDGE_CURVE('',#12771,#12772,#10940,.T.) ;
#15933 = EDGE_CURVE('',#12772,#12773,#6804,.T.) ;
#15934 = EDGE_CURVE('',#12766,#12773,#6805,.T.) ;
#15935 = EDGE_CURVE('',#12753,#12774,#6806,.T.) ;
#15936 = EDGE_CURVE('',#12774,#12775,#6807,.T.) ;
#15937 = EDGE_CURVE('',#12775,#12751,#10941,.T.) ;
#15938 = EDGE_CURVE('',#12776,#12772,#6808,.T.) ;
#15939 = EDGE_CURVE('',#12777,#12776,#6809,.T.) ;
#15940 = EDGE_CURVE('',#12777,#12773,#6810,.T.) ;
#15941 = EDGE_CURVE('',#12778,#12779,#6811,.T.) ;
#15942 = EDGE_CURVE('',#12780,#12778,#6812,.T.) ;
#15943 = EDGE_CURVE('',#12781,#12780,#6813,.T.) ;
#15944 = EDGE_CURVE('',#12779,#12781,#6814,.T.) ;
#15945 = EDGE_CURVE('',#12782,#12783,#6815,.T.) ;
#15946 = EDGE_CURVE('',#12784,#12782,#6816,.T.) ;
#15947 = EDGE_CURVE('',#12785,#12784,#6817,.T.) ;
#15948 = EDGE_CURVE('',#12783,#12785,#6818,.T.) ;
#15949 = EDGE_CURVE('',#12786,#12787,#6819,.T.) ;
#15950 = EDGE_CURVE('',#12786,#12788,#6820,.T.) ;
#15951 = EDGE_CURVE('',#12789,#12788,#6821,.T.) ;
#15952 = EDGE_CURVE('',#12789,#12787,#6822,.T.) ;
#15953 = EDGE_CURVE('',#12774,#12790,#6823,.T.) ;
#15954 = EDGE_CURVE('',#12791,#12790,#6824,.T.) ;
#15955 = EDGE_CURVE('',#12775,#12791,#6825,.T.) ;
#15956 = EDGE_CURVE('',#12792,#12793,#6826,.T.) ;
#15957 = EDGE_CURVE('',#12794,#12792,#6827,.T.) ;
#15958 = EDGE_CURVE('',#12794,#12795,#6828,.T.) ;
#15959 = EDGE_CURVE('',#12795,#12793,#10942,.T.) ;
#15960 = EDGE_CURVE('',#12795,#12796,#6829,.T.) ;
#15961 = EDGE_CURVE('',#12797,#12796,#6830,.T.) ;
#15962 = EDGE_CURVE('',#12793,#12797,#6831,.T.) ;
#15963 = EDGE_CURVE('',#12793,#12795,#10943,.T.) ;
#15964 = EDGE_CURVE('',#12798,#12799,#6832,.T.) ;
#15965 = EDGE_CURVE('',#12800,#12799,#6833,.T.) ;
#15966 = EDGE_CURVE('',#12800,#12801,#6834,.T.) ;
#15967 = EDGE_CURVE('',#12801,#12802,#6835,.T.) ;
#15968 = EDGE_CURVE('',#12802,#12803,#6836,.T.) ;
#15969 = EDGE_CURVE('',#12792,#12803,#6837,.T.) ;
#15970 = EDGE_CURVE('',#12804,#12797,#6838,.T.) ;
#15971 = EDGE_CURVE('',#12787,#12804,#6839,.T.) ;
#15972 = EDGE_CURVE('',#12789,#12805,#6840,.T.) ;
#15973 = EDGE_CURVE('',#12806,#12805,#6841,.T.) ;
#15974 = EDGE_CURVE('',#12807,#12806,#6842,.T.) ;
#15975 = EDGE_CURVE('',#12808,#12807,#6843,.T.) ;
#15976 = EDGE_CURVE('',#12809,#12808,#6844,.T.) ;
#15977 = EDGE_CURVE('',#12809,#12810,#6845,.T.) ;
#15978 = EDGE_CURVE('',#12810,#12798,#6846,.T.) ;
#15979 = EDGE_CURVE('',#12811,#12812,#6847,.T.) ;
#15980 = EDGE_CURVE('',#12813,#12811,#6848,.T.) ;
#15981 = EDGE_CURVE('',#12813,#12725,#6849,.T.) ;
#15982 = EDGE_CURVE('',#12724,#12814,#6850,.T.) ;
#15983 = EDGE_CURVE('',#12815,#12814,#6851,.T.) ;
#15984 = EDGE_CURVE('',#12815,#12790,#6852,.T.) ;
#15985 = EDGE_CURVE('',#12812,#12764,#6853,.T.) ;
#15986 = EDGE_CURVE('',#12807,#12816,#10944,.T.) ;
#15987 = EDGE_CURVE('',#12817,#12816,#6854,.T.) ;
#15988 = EDGE_CURVE('',#12808,#12817,#6855,.T.) ;
#15989 = EDGE_CURVE('',#12818,#12804,#6856,.T.) ;
#15990 = EDGE_CURVE('',#12786,#12818,#6857,.T.) ;
#15991 = EDGE_CURVE('',#12788,#12819,#6858,.T.) ;
#15992 = EDGE_CURVE('',#12805,#12819,#6859,.T.) ;
#15993 = EDGE_CURVE('',#12785,#12820,#6860,.T.) ;
#15994 = EDGE_CURVE('',#12821,#12820,#6861,.T.) ;
#15995 = EDGE_CURVE('',#12783,#12821,#6862,.T.) ;
#15996 = EDGE_CURVE('',#12822,#12821,#6863,.T.) ;
#15997 = EDGE_CURVE('',#12782,#12822,#6864,.T.) ;
#15998 = EDGE_CURVE('',#12781,#12823,#6865,.T.) ;
#15999 = EDGE_CURVE('',#12824,#12823,#6866,.T.) ;
#16000 = EDGE_CURVE('',#12779,#12824,#6867,.T.) ;
#16001 = EDGE_CURVE('',#12825,#12824,#6868,.T.) ;
#16002 = EDGE_CURVE('',#12778,#12825,#6869,.T.) ;
#16003 = EDGE_CURVE('',#12796,#12818,#6870,.T.) ;
#16004 = EDGE_CURVE('',#12820,#12826,#6871,.T.) ;
#16005 = EDGE_CURVE('',#12826,#12822,#6872,.T.) ;
#16006 = EDGE_CURVE('',#12803,#12827,#6873,.T.) ;
#16007 = EDGE_CURVE('',#12827,#12794,#6874,.T.) ;
#16008 = EDGE_CURVE('',#12828,#12828,#10945,.T.) ;
#16009 = EDGE_CURVE('',#12829,#12829,#10946,.T.) ;
#16010 = EDGE_CURVE('',#12819,#12830,#6875,.T.) ;
#16011 = EDGE_CURVE('',#12830,#12806,#6876,.T.) ;
#16012 = EDGE_CURVE('',#12823,#12831,#6877,.T.) ;
#16013 = EDGE_CURVE('',#12831,#12825,#6878,.T.) ;
#16014 = EDGE_CURVE('',#12832,#12811,#6879,.T.) ;
#16015 = EDGE_CURVE('',#12832,#12833,#6880,.T.) ;
#16016 = EDGE_CURVE('',#12813,#12833,#6881,.T.) ;
#16017 = EDGE_CURVE('',#12812,#12765,#6882,.T.) ;
#16018 = EDGE_CURVE('',#12832,#12765,#6883,.T.) ;
#16019 = EDGE_CURVE('',#12816,#12830,#6884,.T.) ;
#16020 = EDGE_CURVE('',#12816,#12807,#10947,.T.) ;
#16021 = EDGE_CURVE('',#12784,#12826,#6885,.T.) ;
#16022 = EDGE_CURVE('',#12780,#12831,#6886,.T.) ;
#16023 = EDGE_CURVE('',#12834,#12834,#10948,.T.) ;
#16024 = EDGE_CURVE('',#12835,#12835,#10949,.T.) ;
#16025 = EDGE_CURVE('',#12836,#12836,#10950,.T.) ;
#16026 = EDGE_CURVE('',#12837,#12837,#10951,.T.) ;
#16027 = EDGE_CURVE('',#12807,#12836,#6887,.T.) ;
#16028 = EDGE_CURVE('',#12834,#12793,#6888,.T.) ;
#16029 = EDGE_CURVE('',#12837,#12829,#6889,.T.) ;
#16030 = EDGE_CURVE('',#12828,#12835,#6890,.T.) ;
#16031 = EDGE_CURVE('',#12799,#12838,#6891,.T.) ;
#16032 = EDGE_CURVE('',#12838,#12839,#6892,.T.) ;
#16033 = EDGE_CURVE('',#12839,#12800,#6893,.T.) ;
#16034 = EDGE_CURVE('',#12840,#12841,#6894,.T.) ;
#16035 = EDGE_CURVE('',#12842,#12841,#6895,.T.) ;
#16036 = EDGE_CURVE('',#12843,#12842,#6896,.T.) ;
#16037 = EDGE_CURVE('',#12840,#12843,#6897,.T.) ;
#16038 = EDGE_CURVE('',#12844,#12845,#6898,.T.) ;
#16039 = EDGE_CURVE('',#12846,#12845,#6899,.T.) ;
#16040 = EDGE_CURVE('',#12847,#12846,#6900,.T.) ;
#16041 = EDGE_CURVE('',#12844,#12847,#6901,.T.) ;
#16042 = EDGE_CURVE('',#12843,#12844,#6902,.T.) ;
#16043 = EDGE_CURVE('',#12847,#12840,#6903,.T.) ;
#16044 = EDGE_CURVE('',#12848,#12849,#6904,.T.) ;
#16045 = EDGE_CURVE('',#12848,#12842,#6905,.T.) ;
#16046 = EDGE_CURVE('',#12841,#12849,#6906,.T.) ;
#16047 = EDGE_CURVE('',#12801,#12846,#6907,.T.) ;
#16048 = EDGE_CURVE('',#12845,#12802,#6908,.T.) ;
#16049 = EDGE_CURVE('',#12849,#12839,#6909,.T.) ;
#16050 = EDGE_CURVE('',#12827,#12848,#6910,.T.) ;
#16051 = EDGE_CURVE('',#12850,#12851,#6911,.T.) ;
#16052 = EDGE_CURVE('',#12851,#12852,#6912,.T.) ;
#16053 = EDGE_CURVE('',#12852,#12853,#6913,.T.) ;
#16054 = EDGE_CURVE('',#12853,#12850,#6914,.T.) ;
#16055 = EDGE_CURVE('',#12770,#12760,#6915,.T.) ;
#16056 = EDGE_CURVE('',#12771,#12759,#6916,.T.) ;
#16057 = EDGE_CURVE('',#12768,#12762,#6917,.T.) ;
#16058 = EDGE_CURVE('',#12761,#12769,#6918,.T.) ;
#16059 = EDGE_CURVE('',#12854,#12855,#6919,.T.) ;
#16060 = EDGE_CURVE('',#12855,#12856,#6920,.T.) ;
#16061 = EDGE_CURVE('',#12856,#12857,#6921,.T.) ;
#16062 = EDGE_CURVE('',#12857,#12854,#6922,.T.) ;
#16063 = EDGE_CURVE('',#12853,#12854,#6923,.T.) ;
#16064 = EDGE_CURVE('',#12850,#12857,#6924,.T.) ;
#16065 = EDGE_CURVE('',#12852,#12855,#6925,.T.) ;
#16066 = EDGE_CURVE('',#12851,#12856,#6926,.T.) ;
#16067 = EDGE_CURVE('',#12858,#12858,#10952,.T.) ;
#16068 = EDGE_CURVE('',#12859,#12859,#10953,.T.) ;
#16069 = EDGE_CURVE('',#12860,#12860,#10954,.T.) ;
#16070 = EDGE_CURVE('',#12859,#12861,#6927,.T.) ;
#16071 = EDGE_CURVE('',#12861,#12861,#10955,.T.) ;
#16072 = EDGE_CURVE('',#12754,#12860,#6928,.T.) ;
#16073 = EDGE_CURVE('',#12862,#12862,#10956,.T.) ;
#16074 = EDGE_CURVE('',#12863,#12863,#10957,.T.) ;
#16075 = EDGE_CURVE('',#12864,#12864,#10958,.T.) ;
#16076 = EDGE_CURVE('',#12863,#12862,#6929,.T.) ;
#16077 = EDGE_CURVE('',#12858,#12864,#6930,.T.) ;
#16078 = EDGE_CURVE('',#12865,#12866,#6931,.T.) ;
#16079 = EDGE_CURVE('',#12866,#12749,#10959,.T.) ;
#16080 = EDGE_CURVE('',#12776,#12748,#10960,.T.) ;
#16081 = EDGE_CURVE('',#12865,#12791,#10961,.T.) ;
#16082 = EDGE_CURVE('',#12815,#12865,#6932,.T.) ;
#16083 = EDGE_CURVE('',#12833,#12726,#6933,.T.) ;
#16084 = EDGE_CURVE('',#12747,#12777,#6934,.T.) ;
#16085 = EDGE_CURVE('',#12722,#12867,#6935,.T.) ;
#16086 = EDGE_CURVE('',#12868,#12867,#6936,.T.) ;
#16087 = EDGE_CURVE('',#12723,#12868,#6937,.T.) ;
#16088 = EDGE_CURVE('',#12814,#12866,#6938,.T.) ;
#16089 = EDGE_CURVE('',#12746,#12868,#6939,.T.) ;
#16090 = EDGE_CURVE('',#12867,#12745,#6940,.T.) ;
#16091 = EDGE_CURVE('',#12726,#12747,#6941,.T.) ;
#16092 = EDGE_CURVE('',#12869,#12809,#6942,.T.) ;
#16093 = EDGE_CURVE('',#12817,#12869,#6943,.T.) ;
#16094 = EDGE_CURVE('',#12838,#12870,#6944,.T.) ;
#16095 = EDGE_CURVE('',#12870,#12871,#6945,.T.) ;
#16096 = EDGE_CURVE('',#12871,#12869,#6946,.T.) ;
#16097 = EDGE_CURVE('',#12872,#12873,#6947,.T.) ;
#16098 = EDGE_CURVE('',#12874,#12873,#6948,.T.) ;
#16099 = EDGE_CURVE('',#12875,#12874,#6949,.T.) ;
#16100 = EDGE_CURVE('',#12872,#12875,#6950,.T.) ;
#16101 = EDGE_CURVE('',#12876,#12877,#6951,.T.) ;
#16102 = EDGE_CURVE('',#12878,#12877,#6952,.T.) ;
#16103 = EDGE_CURVE('',#12879,#12878,#6953,.T.) ;
#16104 = EDGE_CURVE('',#12876,#12879,#6954,.T.) ;
#16105 = EDGE_CURVE('',#12873,#12871,#6955,.T.) ;
#16106 = EDGE_CURVE('',#12879,#12872,#6956,.T.) ;
#16107 = EDGE_CURVE('',#12810,#12878,#6957,.T.) ;
#16108 = EDGE_CURVE('',#12870,#12874,#6958,.T.) ;
#16109 = EDGE_CURVE('',#12875,#12876,#6959,.T.) ;
#16110 = EDGE_CURVE('',#12877,#12798,#6960,.T.) ;
#16111 = EDGE_CURVE('',#12880,#12881,#10962,.T.) ;
#16112 = EDGE_CURVE('',#12882,#12880,#6961,.T.) ;
#16113 = EDGE_CURVE('',#12883,#12882,#10963,.T.) ;
#16114 = EDGE_CURVE('',#12881,#12883,#6962,.T.) ;
#16115 = EDGE_CURVE('',#12884,#12883,#6963,.T.) ;
#16116 = EDGE_CURVE('',#12884,#12885,#6964,.T.) ;
#16117 = EDGE_CURVE('',#12885,#12881,#6965,.T.) ;
#16118 = EDGE_CURVE('',#12886,#12882,#6966,.T.) ;
#16119 = EDGE_CURVE('',#12886,#12884,#6967,.T.) ;
#16120 = EDGE_CURVE('',#12887,#12880,#6968,.T.) ;
#16121 = EDGE_CURVE('',#12887,#12886,#6969,.T.) ;
#16122 = EDGE_CURVE('',#12885,#12887,#6970,.T.) ;
#16123 = EDGE_CURVE('',#12888,#12889,#6971,.T.) ;
#16124 = EDGE_CURVE('',#12890,#12888,#6972,.T.) ;
#16125 = EDGE_CURVE('',#12891,#12890,#6973,.T.) ;
#16126 = EDGE_CURVE('',#12889,#12891,#6974,.T.) ;
#16127 = EDGE_CURVE('',#12892,#12893,#10964,.T.) ;
#16128 = EDGE_CURVE('',#12891,#12893,#6975,.T.) ;
#16129 = EDGE_CURVE('',#12890,#12892,#6976,.T.) ;
#16130 = EDGE_CURVE('',#12894,#12892,#6977,.T.) ;
#16131 = EDGE_CURVE('',#12888,#12894,#6978,.T.) ;
#16132 = EDGE_CURVE('',#12895,#12894,#10965,.T.) ;
#16133 = EDGE_CURVE('',#12889,#12895,#6979,.T.) ;
#16134 = EDGE_CURVE('',#12893,#12895,#6980,.T.) ;
#16135 = EDGE_CURVE('',#12896,#12897,#10966,.T.) ;
#16136 = EDGE_CURVE('',#12896,#12897,#6981,.T.) ;
#16137 = EDGE_CURVE('',#12898,#12899,#10967,.T.) ;
#16138 = EDGE_CURVE('',#12898,#12899,#6982,.T.) ;
#16139 = EDGE_CURVE('',#12897,#12898,#6983,.T.) ;
#16140 = EDGE_CURVE('',#12899,#12896,#6984,.T.) ;
#16141 = EDGE_CURVE('',#12900,#12901,#6985,.T.) ;
#16142 = EDGE_CURVE('',#12902,#12900,#6986,.T.) ;
#16143 = EDGE_CURVE('',#12903,#12902,#6987,.T.) ;
#16144 = EDGE_CURVE('',#12901,#12903,#6988,.T.) ;
#16145 = EDGE_CURVE('',#12901,#12904,#6989,.T.) ;
#16146 = EDGE_CURVE('',#12905,#12903,#6990,.T.) ;
#16147 = EDGE_CURVE('',#12904,#12905,#6991,.T.) ;
#16148 = EDGE_CURVE('',#12904,#12900,#10968,.T.) ;
#16149 = EDGE_CURVE('',#12902,#12905,#10969,.T.) ;
#16150 = EDGE_CURVE('',#12906,#12907,#6992,.T.) ;
#16151 = EDGE_CURVE('',#12907,#12908,#10970,.T.) ;
#16152 = EDGE_CURVE('',#12908,#12906,#6993,.T.) ;
#16153 = EDGE_CURVE('',#12909,#12906,#6994,.T.) ;
#16154 = EDGE_CURVE('',#12908,#12910,#6995,.T.) ;
#16155 = EDGE_CURVE('',#12910,#12909,#6996,.T.) ;
#16156 = EDGE_CURVE('',#12911,#12909,#6997,.T.) ;
#16157 = EDGE_CURVE('',#12910,#12911,#10971,.T.) ;
#16158 = EDGE_CURVE('',#12907,#12911,#6998,.T.) ;
#16159 = EDGE_CURVE('',#12912,#12913,#6999,.T.) ;
#16160 = EDGE_CURVE('',#12914,#12912,#7000,.T.) ;
#16161 = EDGE_CURVE('',#12915,#12914,#7001,.T.) ;
#16162 = EDGE_CURVE('',#12913,#12915,#7002,.T.) ;
#16163 = EDGE_CURVE('',#12916,#12912,#7003,.T.) ;
#16164 = EDGE_CURVE('',#12917,#12916,#7004,.T.) ;
#16165 = EDGE_CURVE('',#12914,#12917,#7005,.T.) ;
#16166 = EDGE_CURVE('',#12913,#12916,#10972,.T.) ;
#16167 = EDGE_CURVE('',#12917,#12915,#10973,.T.) ;
#16168 = EDGE_CURVE('',#12918,#12919,#7006,.T.) ;
#16169 = EDGE_CURVE('',#12920,#12919,#7007,.T.) ;
#16170 = EDGE_CURVE('',#12920,#12918,#10974,.T.) ;
#16171 = EDGE_CURVE('',#12921,#12922,#7008,.T.) ;
#16172 = EDGE_CURVE('',#12922,#12923,#10975,.T.) ;
#16173 = EDGE_CURVE('',#12923,#12921,#7009,.T.) ;
#16174 = EDGE_CURVE('',#12922,#12918,#7010,.T.) ;
#16175 = EDGE_CURVE('',#12923,#12920,#7011,.T.) ;
#16176 = EDGE_CURVE('',#12919,#12921,#7012,.T.) ;
#16177 = EDGE_CURVE('',#12924,#12925,#7013,.T.) ;
#16178 = EDGE_CURVE('',#12926,#12924,#7014,.T.) ;
#16179 = EDGE_CURVE('',#12927,#12926,#7015,.T.) ;
#16180 = EDGE_CURVE('',#12925,#12927,#7016,.T.) ;
#16181 = EDGE_CURVE('',#12928,#12924,#10976,.T.) ;
#16182 = EDGE_CURVE('',#12929,#12928,#7017,.T.) ;
#16183 = EDGE_CURVE('',#12926,#12929,#10977,.T.) ;
#16184 = EDGE_CURVE('',#12928,#12925,#7018,.T.) ;
#16185 = EDGE_CURVE('',#12929,#12927,#7019,.T.) ;
#16186 = EDGE_CURVE('',#12930,#12931,#7020,.T.) ;
#16187 = EDGE_CURVE('',#12932,#12931,#7021,.T.) ;
#16188 = EDGE_CURVE('',#12932,#12930,#10978,.T.) ;
#16189 = EDGE_CURVE('',#12933,#12934,#7022,.T.) ;
#16190 = EDGE_CURVE('',#12934,#12935,#10979,.T.) ;
#16191 = EDGE_CURVE('',#12935,#12933,#7023,.T.) ;
#16192 = EDGE_CURVE('',#12934,#12930,#7024,.T.) ;
#16193 = EDGE_CURVE('',#12935,#12932,#7025,.T.) ;
#16194 = EDGE_CURVE('',#12931,#12933,#7026,.T.) ;
#16195 = EDGE_CURVE('',#12936,#12937,#7027,.T.) ;
#16196 = EDGE_CURVE('',#12938,#12936,#7028,.T.) ;
#16197 = EDGE_CURVE('',#12939,#12938,#7029,.T.) ;
#16198 = EDGE_CURVE('',#12937,#12939,#7030,.T.) ;
#16199 = EDGE_CURVE('',#12939,#12937,#10980,.T.) ;
#16200 = EDGE_CURVE('',#12936,#12938,#10981,.T.) ;
#16201 = EDGE_CURVE('',#12940,#12941,#7031,.T.) ;
#16202 = EDGE_CURVE('',#12942,#12941,#10982,.T.) ;
#16203 = EDGE_CURVE('',#12942,#12943,#7032,.T.) ;
#16204 = EDGE_CURVE('',#12940,#12943,#10983,.T.) ;
#16205 = EDGE_CURVE('',#12943,#12940,#7033,.T.) ;
#16206 = EDGE_CURVE('',#12941,#12942,#7034,.T.) ;
#16207 = EDGE_CURVE('',#12944,#12945,#7035,.T.) ;
#16208 = EDGE_CURVE('',#12946,#12944,#7036,.T.) ;
#16209 = EDGE_CURVE('',#12947,#12946,#7037,.T.) ;
#16210 = EDGE_CURVE('',#12945,#12947,#7038,.T.) ;
#16211 = EDGE_CURVE('',#12946,#12947,#10984,.T.) ;
#16212 = EDGE_CURVE('',#12945,#12944,#10985,.T.) ;
#16213 = EDGE_CURVE('',#12948,#12949,#7039,.T.) ;
#16214 = EDGE_CURVE('',#12950,#12949,#10986,.T.) ;
#16215 = EDGE_CURVE('',#12950,#12951,#7040,.T.) ;
#16216 = EDGE_CURVE('',#12948,#12951,#10987,.T.) ;
#16217 = EDGE_CURVE('',#12949,#12950,#7041,.T.) ;
#16218 = EDGE_CURVE('',#12951,#12948,#7042,.T.) ;
#16219 = EDGE_CURVE('',#12952,#12953,#7043,.T.) ;
#16220 = EDGE_CURVE('',#12954,#12952,#7044,.T.) ;
#16221 = EDGE_CURVE('',#12955,#12954,#7045,.T.) ;
#16222 = EDGE_CURVE('',#12953,#12955,#7046,.T.) ;
#16223 = EDGE_CURVE('',#12952,#12954,#10988,.T.) ;
#16224 = EDGE_CURVE('',#12955,#12953,#10989,.T.) ;
#16225 = EDGE_CURVE('',#12956,#12957,#7047,.T.) ;
#16226 = EDGE_CURVE('',#12957,#12958,#7048,.T.) ;
#16227 = EDGE_CURVE('',#12958,#12959,#7049,.T.) ;
#16228 = EDGE_CURVE('',#12956,#12959,#7050,.T.) ;
#16229 = EDGE_CURVE('',#12957,#12960,#7051,.T.) ;
#16230 = EDGE_CURVE('',#12960,#12961,#7052,.T.) ;
#16231 = EDGE_CURVE('',#12961,#12958,#7053,.T.) ;
#16232 = EDGE_CURVE('',#12962,#12956,#7054,.T.) ;
#16233 = EDGE_CURVE('',#12959,#12963,#7055,.T.) ;
#16234 = EDGE_CURVE('',#12962,#12963,#7056,.T.) ;
#16235 = EDGE_CURVE('',#12960,#12962,#7057,.T.) ;
#16236 = EDGE_CURVE('',#12963,#12961,#7058,.T.) ;
#16237 = EDGE_CURVE('',#12964,#12965,#7059,.T.) ;
#16238 = EDGE_CURVE('',#12966,#12964,#7060,.T.) ;
#16239 = EDGE_CURVE('',#12967,#12966,#7061,.T.) ;
#16240 = EDGE_CURVE('',#12965,#12967,#7062,.T.) ;
#16241 = EDGE_CURVE('',#12968,#12969,#7063,.T.) ;
#16242 = EDGE_CURVE('',#12970,#12968,#7064,.T.) ;
#16243 = EDGE_CURVE('',#12971,#12970,#7065,.T.) ;
#16244 = EDGE_CURVE('',#12969,#12971,#7066,.T.) ;
#16245 = EDGE_CURVE('',#12965,#12968,#7067,.T.) ;
#16246 = EDGE_CURVE('',#12964,#12969,#7068,.T.) ;
#16247 = EDGE_CURVE('',#12967,#12970,#7069,.T.) ;
#16248 = EDGE_CURVE('',#12966,#12971,#7070,.T.) ;
#16249 = EDGE_CURVE('',#12972,#12973,#7071,.T.) ;
#16250 = EDGE_CURVE('',#12974,#12972,#7072,.T.) ;
#16251 = EDGE_CURVE('',#12975,#12974,#7073,.T.) ;
#16252 = EDGE_CURVE('',#12973,#12975,#7074,.T.) ;
#16253 = EDGE_CURVE('',#12976,#12972,#7075,.T.) ;
#16254 = EDGE_CURVE('',#12976,#12977,#7076,.T.) ;
#16255 = EDGE_CURVE('',#12974,#12977,#7077,.T.) ;
#16256 = EDGE_CURVE('',#12978,#12976,#7078,.T.) ;
#16257 = EDGE_CURVE('',#12979,#12978,#7079,.T.) ;
#16258 = EDGE_CURVE('',#12977,#12979,#7080,.T.) ;
#16259 = EDGE_CURVE('',#12979,#12980,#7081,.T.) ;
#16260 = EDGE_CURVE('',#12980,#12981,#7082,.T.) ;
#16261 = EDGE_CURVE('',#12981,#12982,#7083,.T.) ;
#16262 = EDGE_CURVE('',#12982,#12983,#7084,.T.) ;
#16263 = EDGE_CURVE('',#12983,#12984,#7085,.T.) ;
#16264 = EDGE_CURVE('',#12985,#12984,#7086,.T.) ;
#16265 = EDGE_CURVE('',#12985,#12986,#7087,.T.) ;
#16266 = EDGE_CURVE('',#12987,#12986,#7088,.T.) ;
#16267 = EDGE_CURVE('',#12987,#12975,#7089,.T.) ;
#16268 = EDGE_CURVE('',#12988,#12978,#7090,.T.) ;
#16269 = EDGE_CURVE('',#12988,#12980,#7091,.T.) ;
#16270 = EDGE_CURVE('',#12989,#12987,#7092,.T.) ;
#16271 = EDGE_CURVE('',#12973,#12989,#7093,.T.) ;
#16272 = EDGE_CURVE('',#12990,#12989,#7094,.T.) ;
#16273 = EDGE_CURVE('',#12990,#12991,#7095,.T.) ;
#16274 = EDGE_CURVE('',#12992,#12991,#7096,.T.) ;
#16275 = EDGE_CURVE('',#12992,#12993,#7097,.T.) ;
#16276 = EDGE_CURVE('',#12993,#12994,#7098,.T.) ;
#16277 = EDGE_CURVE('',#12994,#12995,#7099,.T.) ;
#16278 = EDGE_CURVE('',#12995,#12988,#7100,.T.) ;
#16279 = EDGE_CURVE('',#12991,#12985,#7101,.T.) ;
#16280 = EDGE_CURVE('',#12986,#12990,#7102,.T.) ;
#16281 = EDGE_CURVE('',#12984,#12992,#7103,.T.) ;
#16282 = EDGE_CURVE('',#12983,#12993,#7104,.T.) ;
#16283 = EDGE_CURVE('',#12994,#12982,#7105,.T.) ;
#16284 = EDGE_CURVE('',#12981,#12995,#7106,.T.) ;
#16285 = EDGE_CURVE('',#12996,#12997,#7107,.T.) ;
#16286 = EDGE_CURVE('',#12997,#12998,#10990,.T.) ;
#16287 = EDGE_CURVE('',#12998,#12999,#7108,.T.) ;
#16288 = EDGE_CURVE('',#12999,#12996,#10991,.T.) ;
#16289 = EDGE_CURVE('',#12997,#12998,#7109,.T.) ;
#16290 = EDGE_CURVE('',#12999,#12996,#7110,.T.) ;
#16291 = EDGE_CURVE('',#13000,#13001,#10992,.T.) ;
#16292 = EDGE_CURVE('',#13001,#13000,#7111,.T.) ;
#16293 = EDGE_CURVE('',#13002,#13000,#7112,.T.) ;
#16294 = EDGE_CURVE('',#13003,#13002,#7113,.T.) ;
#16295 = EDGE_CURVE('',#13001,#13003,#7114,.T.) ;
#16296 = EDGE_CURVE('',#13004,#13003,#10993,.T.) ;
#16297 = EDGE_CURVE('',#13004,#13005,#7115,.T.) ;
#16298 = EDGE_CURVE('',#13006,#13005,#10994,.T.) ;
#16299 = EDGE_CURVE('',#13006,#13007,#7116,.T.) ;
#16300 = EDGE_CURVE('',#13007,#13008,#10995,.T.) ;
#16301 = EDGE_CURVE('',#13008,#13009,#7117,.T.) ;
#16302 = EDGE_CURVE('',#13010,#13009,#10996,.T.) ;
#16303 = EDGE_CURVE('',#13010,#13011,#7118,.T.) ;
#16304 = EDGE_CURVE('',#13002,#13011,#10997,.T.) ;
#16305 = EDGE_CURVE('',#13008,#13007,#7119,.T.) ;
#16306 = EDGE_CURVE('',#13009,#13006,#7120,.T.) ;
#16307 = EDGE_CURVE('',#13005,#13010,#7121,.T.) ;
#16308 = EDGE_CURVE('',#13011,#13004,#7122,.T.) ;
#16309 = EDGE_CURVE('',#13012,#13013,#7123,.T.) ;
#16310 = EDGE_CURVE('',#13013,#13014,#7124,.T.) ;
#16311 = EDGE_CURVE('',#13014,#13015,#7125,.T.) ;
#16312 = EDGE_CURVE('',#13015,#13012,#7126,.T.) ;
#16313 = EDGE_CURVE('',#13016,#13017,#7127,.T.) ;
#16314 = EDGE_CURVE('',#13017,#13018,#7128,.T.) ;
#16315 = EDGE_CURVE('',#13018,#13019,#7129,.T.) ;
#16316 = EDGE_CURVE('',#13019,#13016,#7130,.T.) ;
#16317 = EDGE_CURVE('',#13015,#13018,#7131,.T.) ;
#16318 = EDGE_CURVE('',#13012,#13017,#7132,.T.) ;
#16319 = EDGE_CURVE('',#13014,#13019,#7133,.T.) ;
#16320 = EDGE_CURVE('',#13013,#13016,#7134,.T.) ;
#16321 = EDGE_CURVE('',#13020,#13021,#11,.T.) ;
#16322 = EDGE_CURVE('',#13021,#13020,#12,.T.) ;
#16323 = EDGE_CURVE('',#13021,#13022,#7135,.T.) ;
#16324 = EDGE_CURVE('',#13023,#13022,#13,.T.) ;
#16325 = EDGE_CURVE('',#13022,#13023,#14,.T.) ;
#16326 = EDGE_CURVE('',#13024,#13024,#10998,.T.) ;
#16327 = EDGE_CURVE('',#13025,#13025,#10999,.T.) ;
#16328 = EDGE_CURVE('',#13024,#13026,#7136,.T.) ;
#16329 = EDGE_CURVE('',#13026,#13026,#11000,.T.) ;
#16330 = EDGE_CURVE('',#13027,#13027,#11001,.T.) ;
#16331 = EDGE_CURVE('',#13027,#13025,#7137,.T.) ;
#16332 = EDGE_CURVE('',#13028,#13029,#15,.T.) ;
#16333 = EDGE_CURVE('',#13029,#13028,#16,.T.) ;
#16334 = EDGE_CURVE('',#13029,#13030,#7138,.T.) ;
#16335 = EDGE_CURVE('',#13031,#13030,#17,.T.) ;
#16336 = EDGE_CURVE('',#13030,#13031,#18,.T.) ;
#16337 = EDGE_CURVE('',#13032,#13032,#11002,.T.) ;
#16338 = EDGE_CURVE('',#13033,#13033,#11003,.T.) ;
#16339 = EDGE_CURVE('',#13032,#13034,#7139,.T.) ;
#16340 = EDGE_CURVE('',#13034,#13034,#11004,.T.) ;
#16341 = EDGE_CURVE('',#13035,#13035,#11005,.T.) ;
#16342 = EDGE_CURVE('',#13035,#13033,#7140,.T.) ;
#16343 = EDGE_CURVE('',#13036,#13036,#11006,.T.) ;
#16344 = EDGE_CURVE('',#13036,#13037,#7141,.T.) ;
#16345 = EDGE_CURVE('',#13037,#13037,#11007,.T.) ;
#16346 = EDGE_CURVE('',#13038,#13038,#11008,.T.) ;
#16347 = EDGE_CURVE('',#13038,#13039,#7142,.T.) ;
#16348 = EDGE_CURVE('',#13039,#13039,#11009,.T.) ;
#16349 = EDGE_CURVE('',#13040,#13040,#11010,.T.) ;
#16350 = EDGE_CURVE('',#13040,#13041,#7143,.T.) ;
#16351 = EDGE_CURVE('',#13041,#13041,#11011,.T.) ;
#16352 = EDGE_CURVE('',#13042,#13042,#11012,.T.) ;
#16353 = EDGE_CURVE('',#13042,#13043,#7144,.T.) ;
#16354 = EDGE_CURVE('',#13043,#13043,#11013,.T.) ;
#16355 = EDGE_CURVE('',#13044,#13045,#7145,.T.) ;
#16356 = EDGE_CURVE('',#13044,#13046,#11014,.T.) ;
#16357 = EDGE_CURVE('',#13047,#13046,#7146,.T.) ;
#16358 = EDGE_CURVE('',#13045,#13047,#11015,.T.) ;
#16359 = EDGE_CURVE('',#13046,#13044,#7147,.T.) ;
#16360 = EDGE_CURVE('',#13047,#13048,#7148,.T.) ;
#16361 = EDGE_CURVE('',#13048,#13049,#7149,.T.) ;
#16362 = EDGE_CURVE('',#13049,#13050,#11016,.T.) ;
#16363 = EDGE_CURVE('',#13050,#13051,#11017,.T.) ;
#16364 = EDGE_CURVE('',#13051,#13052,#11018,.T.) ;
#16365 = EDGE_CURVE('',#13052,#13053,#11019,.T.) ;
#16366 = EDGE_CURVE('',#13053,#13049,#11020,.T.) ;
#16367 = EDGE_CURVE('',#13049,#13054,#7150,.T.) ;
#16368 = EDGE_CURVE('',#13054,#13055,#7151,.T.) ;
#16369 = EDGE_CURVE('',#13055,#13056,#11021,.T.) ;
#16370 = EDGE_CURVE('',#13056,#13057,#7152,.T.) ;
#16371 = EDGE_CURVE('',#13057,#13058,#11022,.T.) ;
#16372 = EDGE_CURVE('',#13058,#13059,#7153,.T.) ;
#16373 = EDGE_CURVE('',#13059,#13060,#7154,.T.) ;
#16374 = EDGE_CURVE('',#13060,#13061,#7155,.T.) ;
#16375 = EDGE_CURVE('',#13061,#13062,#11023,.T.) ;
#16376 = EDGE_CURVE('',#13062,#13045,#7156,.T.) ;
#16377 = EDGE_CURVE('',#13063,#13064,#7157,.T.) ;
#16378 = EDGE_CURVE('',#13064,#13063,#11024,.T.) ;
#16379 = EDGE_CURVE('',#13062,#13063,#7158,.T.) ;
#16380 = EDGE_CURVE('',#13064,#13061,#7159,.T.) ;
#16381 = EDGE_CURVE('',#13060,#13065,#7160,.T.) ;
#16382 = EDGE_CURVE('',#13066,#13065,#7161,.T.) ;
#16383 = EDGE_CURVE('',#13066,#13067,#7162,.T.) ;
#16384 = EDGE_CURVE('',#13068,#13067,#7163,.T.) ;
#16385 = EDGE_CURVE('',#13068,#13069,#7164,.T.) ;
#16386 = EDGE_CURVE('',#13070,#13069,#7165,.T.) ;
#16387 = EDGE_CURVE('',#13071,#13070,#7166,.T.) ;
#16388 = EDGE_CURVE('',#13072,#13071,#7167,.T.) ;
#16389 = EDGE_CURVE('',#13073,#13072,#7168,.T.) ;
#16390 = EDGE_CURVE('',#13074,#13073,#7169,.T.) ;
#16391 = EDGE_CURVE('',#13048,#13074,#7170,.T.) ;
#16392 = EDGE_CURVE('',#13075,#13075,#11025,.T.) ;
#16393 = EDGE_CURVE('',#13076,#13077,#7171,.T.) ;
#16394 = EDGE_CURVE('',#13077,#13076,#11026,.T.) ;
#16395 = EDGE_CURVE('',#13056,#13076,#7172,.T.) ;
#16396 = EDGE_CURVE('',#13077,#13055,#7173,.T.) ;
#16397 = EDGE_CURVE('',#13054,#13078,#7174,.T.) ;
#16398 = EDGE_CURVE('',#13079,#13078,#7175,.T.) ;
#16399 = EDGE_CURVE('',#13079,#13080,#7176,.T.) ;
#16400 = EDGE_CURVE('',#13081,#13080,#7177,.T.) ;
#16401 = EDGE_CURVE('',#13081,#13082,#7178,.T.) ;
#16402 = EDGE_CURVE('',#13083,#13082,#7179,.T.) ;
#16403 = EDGE_CURVE('',#13084,#13083,#7180,.T.) ;
#16404 = EDGE_CURVE('',#13085,#13084,#7181,.T.) ;
#16405 = EDGE_CURVE('',#13086,#13085,#7182,.T.) ;
#16406 = EDGE_CURVE('',#13087,#13086,#7183,.T.) ;
#16407 = EDGE_CURVE('',#13059,#13087,#7184,.T.) ;
#16408 = EDGE_CURVE('',#13058,#13088,#7185,.T.) ;
#16409 = EDGE_CURVE('',#13088,#13089,#7186,.T.) ;
#16410 = EDGE_CURVE('',#13089,#13057,#7187,.T.) ;
#16411 = EDGE_CURVE('',#13090,#13090,#11027,.T.) ;
#16412 = EDGE_CURVE('',#13089,#13088,#11028,.T.) ;
#16413 = EDGE_CURVE('',#13091,#13091,#11029,.T.) ;
#16414 = EDGE_CURVE('',#13091,#13092,#7188,.T.) ;
#16415 = EDGE_CURVE('',#13092,#13092,#11030,.T.) ;
#16416 = EDGE_CURVE('',#13093,#13093,#11031,.T.) ;
#16417 = EDGE_CURVE('',#13093,#13090,#7189,.T.) ;
#16418 = EDGE_CURVE('',#13094,#13095,#7190,.T.) ;
#16419 = EDGE_CURVE('',#13096,#13094,#11032,.T.) ;
#16420 = EDGE_CURVE('',#13097,#13096,#7191,.T.) ;
#16421 = EDGE_CURVE('',#13095,#13097,#11033,.T.) ;
#16422 = EDGE_CURVE('',#13098,#13099,#7192,.T.) ;
#16423 = EDGE_CURVE('',#13100,#13098,#11034,.T.) ;
#16424 = EDGE_CURVE('',#13101,#13100,#7193,.T.) ;
#16425 = EDGE_CURVE('',#13099,#13101,#11035,.T.) ;
#16426 = EDGE_CURVE('',#13102,#13098,#7194,.T.) ;
#16427 = EDGE_CURVE('',#13103,#13102,#7195,.T.) ;
#16428 = EDGE_CURVE('',#13104,#13103,#7196,.T.) ;
#16429 = EDGE_CURVE('',#13104,#13105,#7197,.T.) ;
#16430 = EDGE_CURVE('',#13100,#13105,#7198,.T.) ;
#16431 = EDGE_CURVE('',#13099,#13106,#7199,.T.) ;
#16432 = EDGE_CURVE('',#13106,#13102,#7200,.T.) ;
#16433 = EDGE_CURVE('',#13105,#13107,#7201,.T.) ;
#16434 = EDGE_CURVE('',#13107,#13101,#7202,.T.) ;
#16435 = EDGE_CURVE('',#13108,#13094,#7203,.T.) ;
#16436 = EDGE_CURVE('',#13109,#13108,#7204,.T.) ;
#16437 = EDGE_CURVE('',#13110,#13109,#7205,.T.) ;
#16438 = EDGE_CURVE('',#13110,#13111,#7206,.T.) ;
#16439 = EDGE_CURVE('',#13096,#13111,#7207,.T.) ;
#16440 = EDGE_CURVE('',#13095,#13112,#7208,.T.) ;
#16441 = EDGE_CURVE('',#13112,#13108,#7209,.T.) ;
#16442 = EDGE_CURVE('',#13111,#13113,#7210,.T.) ;
#16443 = EDGE_CURVE('',#13113,#13097,#7211,.T.) ;
#16444 = EDGE_CURVE('',#13114,#13106,#7212,.T.) ;
#16445 = EDGE_CURVE('',#13103,#13114,#7213,.T.) ;
#16446 = EDGE_CURVE('',#13115,#13107,#7214,.T.) ;
#16447 = EDGE_CURVE('',#13115,#13104,#7215,.T.) ;
#16448 = EDGE_CURVE('',#13114,#13115,#7216,.T.) ;
#16449 = EDGE_CURVE('',#13116,#13112,#7217,.T.) ;
#16450 = EDGE_CURVE('',#13109,#13116,#7218,.T.) ;
#16451 = EDGE_CURVE('',#13117,#13113,#7219,.T.) ;
#16452 = EDGE_CURVE('',#13117,#13110,#7220,.T.) ;
#16453 = EDGE_CURVE('',#13116,#13117,#7221,.T.) ;
#16454 = EDGE_CURVE('',#13118,#13119,#11036,.T.) ;
#16455 = EDGE_CURVE('',#13119,#13118,#11037,.T.) ;
#16456 = EDGE_CURVE('',#13120,#13120,#11038,.T.) ;
#16457 = EDGE_CURVE('',#13120,#13052,#7222,.T.) ;
#16458 = EDGE_CURVE('',#13119,#13051,#7223,.T.) ;
#16459 = EDGE_CURVE('',#13053,#13118,#7224,.T.) ;
#16460 = EDGE_CURVE('',#13121,#13121,#11039,.T.) ;
#16461 = EDGE_CURVE('',#13121,#13050,#7225,.T.) ;
#16462 = EDGE_CURVE('',#13122,#13122,#11040,.T.) ;
#16463 = EDGE_CURVE('',#13122,#13123,#7226,.T.) ;
#16464 = EDGE_CURVE('',#13123,#13123,#11041,.T.) ;
#16465 = EDGE_CURVE('',#13124,#13124,#11042,.T.) ;
#16466 = EDGE_CURVE('',#13124,#13125,#7227,.T.) ;
#16467 = EDGE_CURVE('',#13125,#13125,#11043,.T.) ;
#16468 = EDGE_CURVE('',#13126,#13126,#11044,.T.) ;
#16469 = EDGE_CURVE('',#13126,#13127,#7228,.T.) ;
#16470 = EDGE_CURVE('',#13127,#13127,#11045,.T.) ;
#16471 = EDGE_CURVE('',#13128,#13128,#11046,.T.) ;
#16472 = EDGE_CURVE('',#13128,#13129,#7229,.T.) ;
#16473 = EDGE_CURVE('',#13129,#13129,#11047,.T.) ;
#16474 = EDGE_CURVE('',#13075,#13130,#7230,.T.) ;
#16475 = EDGE_CURVE('',#13130,#13130,#11048,.T.) ;
#16476 = EDGE_CURVE('',#13131,#13132,#7231,.T.) ;
#16477 = EDGE_CURVE('',#13074,#13132,#7232,.T.) ;
#16478 = EDGE_CURVE('',#13073,#13131,#7233,.T.) ;
#16479 = EDGE_CURVE('',#13133,#13134,#7234,.T.) ;
#16480 = EDGE_CURVE('',#13134,#13072,#7235,.T.) ;
#16481 = EDGE_CURVE('',#13133,#13071,#7236,.T.) ;
#16482 = EDGE_CURVE('',#13131,#13134,#7237,.T.) ;
#16483 = EDGE_CURVE('',#13132,#13133,#7238,.T.) ;
#16484 = EDGE_CURVE('',#13082,#13070,#7239,.T.) ;
#16485 = EDGE_CURVE('',#13081,#13135,#7240,.T.) ;
#16486 = EDGE_CURVE('',#13135,#13136,#7241,.T.) ;
#16487 = EDGE_CURVE('',#13136,#13078,#7242,.T.) ;
#16488 = EDGE_CURVE('',#13137,#13138,#7243,.T.) ;
#16489 = EDGE_CURVE('',#13138,#13066,#7244,.T.) ;
#16490 = EDGE_CURVE('',#13137,#13065,#7245,.T.) ;
#16491 = EDGE_CURVE('',#13139,#13140,#7246,.T.) ;
#16492 = EDGE_CURVE('',#13068,#13140,#7247,.T.) ;
#16493 = EDGE_CURVE('',#13067,#13139,#7248,.T.) ;
#16494 = EDGE_CURVE('',#13138,#13139,#7249,.T.) ;
#16495 = EDGE_CURVE('',#13140,#13137,#7250,.T.) ;
#16496 = EDGE_CURVE('',#13136,#13141,#7251,.T.) ;
#16497 = EDGE_CURVE('',#13141,#13079,#7252,.T.) ;
#16498 = EDGE_CURVE('',#13080,#13142,#7253,.T.) ;
#16499 = EDGE_CURVE('',#13142,#13135,#7254,.T.) ;
#16500 = EDGE_CURVE('',#13141,#13142,#7255,.T.) ;
#16501 = EDGE_CURVE('',#13086,#13143,#7256,.T.) ;
#16502 = EDGE_CURVE('',#13143,#13144,#7257,.T.) ;
#16503 = EDGE_CURVE('',#13087,#13144,#7258,.T.) ;
#16504 = EDGE_CURVE('',#13145,#13084,#7259,.T.) ;
#16505 = EDGE_CURVE('',#13145,#13146,#7260,.T.) ;
#16506 = EDGE_CURVE('',#13146,#13085,#7261,.T.) ;
#16507 = EDGE_CURVE('',#13143,#13146,#7262,.T.) ;
#16508 = EDGE_CURVE('',#13144,#13145,#7263,.T.) ;
#16509 = EDGE_CURVE('',#13069,#13083,#7264,.T.) ;
#16510 = EDGE_CURVE('',#13147,#13147,#11049,.T.) ;
#16511 = EDGE_CURVE('',#13147,#13148,#7265,.T.) ;
#16512 = EDGE_CURVE('',#13148,#13148,#11050,.T.) ;
#16513 = EDGE_CURVE('',#13149,#13150,#7266,.T.) ;
#16514 = EDGE_CURVE('',#13149,#13151,#7267,.T.) ;
#16515 = EDGE_CURVE('',#13152,#13151,#7268,.T.) ;
#16516 = EDGE_CURVE('',#13152,#13150,#7269,.T.) ;
#16517 = EDGE_CURVE('',#13153,#13154,#7270,.T.) ;
#16518 = EDGE_CURVE('',#13153,#13155,#7271,.T.) ;
#16519 = EDGE_CURVE('',#13156,#13155,#7272,.T.) ;
#16520 = EDGE_CURVE('',#13156,#13154,#7273,.T.) ;
#16521 = EDGE_CURVE('',#13157,#13149,#7274,.T.) ;
#16522 = EDGE_CURVE('',#13155,#13157,#7275,.T.) ;
#16523 = EDGE_CURVE('',#13158,#13153,#7276,.T.) ;
#16524 = EDGE_CURVE('',#13151,#13158,#7277,.T.) ;
#16525 = EDGE_CURVE('',#13157,#13159,#7278,.T.) ;
#16526 = EDGE_CURVE('',#13150,#13159,#7279,.T.) ;
#16527 = EDGE_CURVE('',#13158,#13160,#7280,.T.) ;
#16528 = EDGE_CURVE('',#13154,#13160,#7281,.T.) ;
#16529 = EDGE_CURVE('',#13159,#13156,#7282,.T.) ;
#16530 = EDGE_CURVE('',#13160,#13152,#7283,.T.) ;
#16531 = EDGE_CURVE('',#13161,#13162,#7284,.T.) ;
#16532 = EDGE_CURVE('',#13163,#13161,#11051,.T.) ;
#16533 = EDGE_CURVE('',#13164,#13163,#7285,.T.) ;
#16534 = EDGE_CURVE('',#13165,#13164,#7286,.T.) ;
#16535 = EDGE_CURVE('',#13162,#13165,#11052,.T.) ;
#16536 = EDGE_CURVE('',#13166,#13167,#7287,.T.) ;
#16537 = EDGE_CURVE('',#13168,#13166,#11053,.T.) ;
#16538 = EDGE_CURVE('',#13169,#13168,#7288,.T.) ;
#16539 = EDGE_CURVE('',#13170,#13169,#7289,.T.) ;
#16540 = EDGE_CURVE('',#13167,#13170,#11054,.T.) ;
#16541 = EDGE_CURVE('',#13171,#13172,#7290,.T.) ;
#16542 = EDGE_CURVE('',#13173,#13171,#11055,.T.) ;
#16543 = EDGE_CURVE('',#13174,#13173,#7291,.T.) ;
#16544 = EDGE_CURVE('',#13172,#13174,#11056,.T.) ;
#16545 = EDGE_CURVE('',#13175,#13176,#7292,.T.) ;
#16546 = EDGE_CURVE('',#13177,#13175,#11057,.T.) ;
#16547 = EDGE_CURVE('',#13178,#13177,#7293,.T.) ;
#16548 = EDGE_CURVE('',#13179,#13178,#11058,.T.) ;
#16549 = EDGE_CURVE('',#13176,#13179,#7294,.T.) ;
#16550 = EDGE_CURVE('',#13180,#13181,#7295,.T.) ;
#16551 = EDGE_CURVE('',#13182,#13180,#11059,.T.) ;
#16552 = EDGE_CURVE('',#13183,#13182,#7296,.T.) ;
#16553 = EDGE_CURVE('',#13184,#13183,#7297,.T.) ;
#16554 = EDGE_CURVE('',#13181,#13184,#11060,.T.) ;
#16555 = EDGE_CURVE('',#13185,#13186,#7298,.T.) ;
#16556 = EDGE_CURVE('',#13187,#13185,#11061,.T.) ;
#16557 = EDGE_CURVE('',#13188,#13187,#7299,.T.) ;
#16558 = EDGE_CURVE('',#13186,#13188,#11062,.T.) ;
#16559 = EDGE_CURVE('',#13189,#13175,#7300,.T.) ;
#16560 = EDGE_CURVE('',#13189,#13190,#11063,.T.) ;
#16561 = EDGE_CURVE('',#13177,#13190,#7301,.T.) ;
#16562 = EDGE_CURVE('',#13191,#13171,#7302,.T.) ;
#16563 = EDGE_CURVE('',#13191,#13192,#11064,.T.) ;
#16564 = EDGE_CURVE('',#13173,#13192,#7303,.T.) ;
#16565 = EDGE_CURVE('',#13162,#13193,#7304,.T.) ;
#16566 = EDGE_CURVE('',#13194,#13165,#7305,.T.) ;
#16567 = EDGE_CURVE('',#13194,#13193,#11065,.T.) ;
#16568 = EDGE_CURVE('',#13195,#13166,#7306,.T.) ;
#16569 = EDGE_CURVE('',#13195,#13196,#11066,.T.) ;
#16570 = EDGE_CURVE('',#13168,#13196,#7307,.T.) ;
#16571 = EDGE_CURVE('',#13197,#13180,#7308,.T.) ;
#16572 = EDGE_CURVE('',#13197,#13198,#11067,.T.) ;
#16573 = EDGE_CURVE('',#13182,#13198,#7309,.T.) ;
#16574 = EDGE_CURVE('',#13199,#13185,#7310,.T.) ;
#16575 = EDGE_CURVE('',#13199,#13200,#11068,.T.) ;
#16576 = EDGE_CURVE('',#13187,#13200,#7311,.T.) ;
#16577 = EDGE_CURVE('',#13193,#13201,#7312,.T.) ;
#16578 = EDGE_CURVE('',#13202,#13194,#7313,.T.) ;
#16579 = EDGE_CURVE('',#13203,#13202,#7314,.T.) ;
#16580 = EDGE_CURVE('',#13201,#13203,#11069,.T.) ;
#16581 = EDGE_CURVE('',#13204,#13191,#7315,.T.) ;
#16582 = EDGE_CURVE('',#13205,#13204,#11070,.T.) ;
#16583 = EDGE_CURVE('',#13206,#13205,#11071,.T.) ;
#16584 = EDGE_CURVE('',#13192,#13206,#7316,.T.) ;
#16585 = EDGE_CURVE('',#13207,#13189,#7317,.T.) ;
#16586 = EDGE_CURVE('',#13208,#13207,#7318,.T.) ;
#16587 = EDGE_CURVE('',#13209,#13208,#11072,.T.) ;
#16588 = EDGE_CURVE('',#13190,#13209,#7319,.T.) ;
#16589 = EDGE_CURVE('',#13210,#13197,#7320,.T.) ;
#16590 = EDGE_CURVE('',#13211,#13210,#11073,.T.) ;
#16591 = EDGE_CURVE('',#13212,#13211,#7321,.T.) ;
#16592 = EDGE_CURVE('',#13198,#13212,#7322,.T.) ;
#16593 = EDGE_CURVE('',#13213,#13195,#7323,.T.) ;
#16594 = EDGE_CURVE('',#13214,#13213,#11074,.T.) ;
#16595 = EDGE_CURVE('',#13215,#13214,#7324,.T.) ;
#16596 = EDGE_CURVE('',#13196,#13215,#7325,.T.) ;
#16597 = EDGE_CURVE('',#13216,#13199,#7326,.T.) ;
#16598 = EDGE_CURVE('',#13217,#13216,#11075,.T.) ;
#16599 = EDGE_CURVE('',#13200,#13217,#7327,.T.) ;
#16600 = EDGE_CURVE('',#13218,#13186,#7328,.T.) ;
#16601 = EDGE_CURVE('',#13219,#13218,#7329,.T.) ;
#16602 = EDGE_CURVE('',#13220,#13219,#7330,.T.) ;
#16603 = EDGE_CURVE('',#13221,#13220,#7331,.T.) ;
#16604 = EDGE_CURVE('',#13216,#13221,#7332,.T.) ;
#16605 = EDGE_CURVE('',#13222,#13167,#7333,.T.) ;
#16606 = EDGE_CURVE('',#13223,#13222,#7334,.T.) ;
#16607 = EDGE_CURVE('',#13224,#13223,#7335,.T.) ;
#16608 = EDGE_CURVE('',#13225,#13224,#7336,.T.) ;
#16609 = EDGE_CURVE('',#13213,#13225,#7337,.T.) ;
#16610 = EDGE_CURVE('',#13226,#13169,#7338,.T.) ;
#16611 = EDGE_CURVE('',#13227,#13226,#7339,.T.) ;
#16612 = EDGE_CURVE('',#13170,#13227,#7340,.T.) ;
#16613 = EDGE_CURVE('',#13212,#13228,#7341,.T.) ;
#16614 = EDGE_CURVE('',#13228,#13220,#7342,.T.) ;
#16615 = EDGE_CURVE('',#13229,#13219,#7343,.T.) ;
#16616 = EDGE_CURVE('',#13229,#13183,#7344,.T.) ;
#16617 = EDGE_CURVE('',#13230,#13211,#7345,.T.) ;
#16618 = EDGE_CURVE('',#13228,#13230,#7346,.T.) ;
#16619 = EDGE_CURVE('',#13231,#13229,#7347,.T.) ;
#16620 = EDGE_CURVE('',#13184,#13231,#7348,.T.) ;
#16621 = EDGE_CURVE('',#13232,#13201,#7349,.T.) ;
#16622 = EDGE_CURVE('',#13233,#13232,#7350,.T.) ;
#16623 = EDGE_CURVE('',#13234,#13233,#7351,.T.) ;
#16624 = EDGE_CURVE('',#13235,#13234,#7352,.T.) ;
#16625 = EDGE_CURVE('',#13161,#13235,#7353,.T.) ;
#16626 = EDGE_CURVE('',#13236,#13202,#7354,.T.) ;
#16627 = EDGE_CURVE('',#13237,#13236,#7355,.T.) ;
#16628 = EDGE_CURVE('',#13203,#13237,#7356,.T.) ;
#16629 = EDGE_CURVE('',#13238,#13209,#7357,.T.) ;
#16630 = EDGE_CURVE('',#13239,#13238,#7358,.T.) ;
#16631 = EDGE_CURVE('',#13240,#13239,#7359,.T.) ;
#16632 = EDGE_CURVE('',#13241,#13240,#7360,.T.) ;
#16633 = EDGE_CURVE('',#13178,#13241,#7361,.T.) ;
#16634 = EDGE_CURVE('',#13242,#13207,#7362,.T.) ;
#16635 = EDGE_CURVE('',#13243,#13242,#7363,.T.) ;
#16636 = EDGE_CURVE('',#13208,#13243,#7364,.T.) ;
#16637 = EDGE_CURVE('',#13244,#13179,#7365,.T.) ;
#16638 = EDGE_CURVE('',#13245,#13244,#7366,.T.) ;
#16639 = EDGE_CURVE('',#13176,#13245,#7367,.T.) ;
#16640 = EDGE_CURVE('',#13246,#13206,#7368,.T.) ;
#16641 = EDGE_CURVE('',#13247,#13246,#7369,.T.) ;
#16642 = EDGE_CURVE('',#13248,#13247,#7370,.T.) ;
#16643 = EDGE_CURVE('',#13249,#13248,#7371,.T.) ;
#16644 = EDGE_CURVE('',#13174,#13249,#7372,.T.) ;
#16645 = EDGE_CURVE('',#13250,#13249,#11076,.T.) ;
#16646 = EDGE_CURVE('',#13250,#13172,#7373,.T.) ;
#16647 = EDGE_CURVE('',#13244,#13241,#11077,.T.) ;
#16648 = EDGE_CURVE('',#13251,#13231,#11078,.T.) ;
#16649 = EDGE_CURVE('',#13251,#13181,#7374,.T.) ;
#16650 = EDGE_CURVE('',#13252,#13235,#11079,.T.) ;
#16651 = EDGE_CURVE('',#13252,#13163,#7375,.T.) ;
#16652 = EDGE_CURVE('',#13222,#13227,#11080,.T.) ;
#16653 = EDGE_CURVE('',#13188,#13253,#7376,.T.) ;
#16654 = EDGE_CURVE('',#13218,#13253,#11081,.T.) ;
#16655 = EDGE_CURVE('',#13221,#13230,#11082,.T.) ;
#16656 = EDGE_CURVE('',#13253,#13254,#7377,.T.) ;
#16657 = EDGE_CURVE('',#13254,#13255,#7378,.T.) ;
#16658 = EDGE_CURVE('',#13255,#13252,#7379,.T.) ;
#16659 = EDGE_CURVE('',#13234,#13223,#7380,.T.) ;
#16660 = EDGE_CURVE('',#13226,#13256,#7381,.T.) ;
#16661 = EDGE_CURVE('',#13256,#13250,#7382,.T.) ;
#16662 = EDGE_CURVE('',#13248,#13245,#7383,.T.) ;
#16663 = EDGE_CURVE('',#13240,#13257,#7384,.T.) ;
#16664 = EDGE_CURVE('',#13257,#13251,#7385,.T.) ;
#16665 = EDGE_CURVE('',#13258,#13217,#7386,.T.) ;
#16666 = EDGE_CURVE('',#13259,#13258,#7387,.T.) ;
#16667 = EDGE_CURVE('',#13254,#13259,#7388,.T.) ;
#16668 = EDGE_CURVE('',#13164,#13255,#7389,.T.) ;
#16669 = EDGE_CURVE('',#13259,#13236,#7390,.T.) ;
#16670 = EDGE_CURVE('',#13237,#13258,#11083,.T.) ;
#16671 = EDGE_CURVE('',#13225,#13232,#11084,.T.) ;
#16672 = EDGE_CURVE('',#13224,#13233,#7391,.T.) ;
#16673 = EDGE_CURVE('',#13260,#13260,#11085,.T.) ;
#16674 = EDGE_CURVE('',#13260,#13205,#7392,.T.) ;
#16675 = EDGE_CURVE('',#13204,#13261,#7393,.T.) ;
#16676 = EDGE_CURVE('',#13261,#13262,#11086,.T.) ;
#16677 = EDGE_CURVE('',#13262,#13214,#7394,.T.) ;
#16678 = EDGE_CURVE('',#13210,#13263,#7395,.T.) ;
#16679 = EDGE_CURVE('',#13263,#13238,#11087,.T.) ;
#16680 = EDGE_CURVE('',#13243,#13246,#11088,.T.) ;
#16681 = EDGE_CURVE('',#13264,#13262,#7396,.T.) ;
#16682 = EDGE_CURVE('',#13215,#13264,#7397,.T.) ;
#16683 = EDGE_CURVE('',#13265,#13256,#7398,.T.) ;
#16684 = EDGE_CURVE('',#13261,#13265,#7399,.T.) ;
#16685 = EDGE_CURVE('',#13264,#13265,#7400,.T.) ;
#16686 = EDGE_CURVE('',#13247,#13242,#7401,.T.) ;
#16687 = EDGE_CURVE('',#13266,#13257,#7402,.T.) ;
#16688 = EDGE_CURVE('',#13263,#13266,#7403,.T.) ;
#16689 = EDGE_CURVE('',#13239,#13266,#7404,.T.) ;
#16690 = EDGE_CURVE('',#13267,#13267,#11089,.T.) ;
#16691 = EDGE_CURVE('',#13267,#13268,#7405,.T.) ;
#16692 = EDGE_CURVE('',#13268,#13268,#11090,.T.) ;
#16693 = EDGE_CURVE('',#13269,#13269,#11091,.T.) ;
#16694 = EDGE_CURVE('',#13270,#13270,#11092,.T.) ;
#16695 = EDGE_CURVE('',#13270,#13269,#7406,.T.) ;
#16696 = EDGE_CURVE('',#13271,#13271,#11093,.T.) ;
#16697 = EDGE_CURVE('',#13271,#13272,#7407,.T.) ;
#16698 = EDGE_CURVE('',#13272,#13272,#11094,.T.) ;
#16699 = EDGE_CURVE('',#13273,#13273,#11095,.T.) ;
#16700 = EDGE_CURVE('',#13273,#13274,#7408,.T.) ;
#16701 = EDGE_CURVE('',#13274,#13274,#11096,.T.) ;
#16702 = EDGE_CURVE('',#13275,#13276,#11097,.T.) ;
#16703 = EDGE_CURVE('',#13275,#13277,#7409,.T.) ;
#16704 = EDGE_CURVE('',#13278,#13277,#11098,.T.) ;
#16705 = EDGE_CURVE('',#13276,#13278,#7410,.T.) ;
#16706 = EDGE_CURVE('',#13276,#13279,#7411,.T.) ;
#16707 = EDGE_CURVE('',#13278,#13280,#7412,.T.) ;
#16708 = EDGE_CURVE('',#13281,#13280,#7413,.T.) ;
#16709 = EDGE_CURVE('',#13281,#13282,#7414,.T.) ;
#16710 = EDGE_CURVE('',#13279,#13282,#7415,.T.) ;
#16711 = EDGE_CURVE('',#13282,#13283,#7416,.T.) ;
#16712 = EDGE_CURVE('',#13284,#13281,#7417,.T.) ;
#16713 = EDGE_CURVE('',#13283,#13284,#7418,.T.) ;
#16714 = EDGE_CURVE('',#13285,#13275,#7419,.T.) ;
#16715 = EDGE_CURVE('',#13283,#13285,#7420,.T.) ;
#16716 = EDGE_CURVE('',#13286,#13284,#7421,.T.) ;
#16717 = EDGE_CURVE('',#13286,#13277,#7422,.T.) ;
#16718 = EDGE_CURVE('',#13279,#13287,#11099,.T.) ;
#16719 = EDGE_CURVE('',#13287,#13288,#7423,.T.) ;
#16720 = EDGE_CURVE('',#13289,#13288,#11100,.T.) ;
#16721 = EDGE_CURVE('',#13289,#13290,#7424,.T.) ;
#16722 = EDGE_CURVE('',#13290,#13285,#11101,.T.) ;
#16723 = EDGE_CURVE('',#13277,#13291,#7425,.T.) ;
#16724 = EDGE_CURVE('',#13292,#13291,#11102,.T.) ;
#16725 = EDGE_CURVE('',#13292,#13278,#7426,.T.) ;
#16726 = EDGE_CURVE('',#13293,#13286,#7427,.T.) ;
#16727 = EDGE_CURVE('',#13290,#13293,#7428,.T.) ;
#16728 = EDGE_CURVE('',#13291,#13289,#7429,.T.) ;
#16729 = EDGE_CURVE('',#13280,#13294,#7430,.T.) ;
#16730 = EDGE_CURVE('',#13295,#13294,#7431,.T.) ;
#16731 = EDGE_CURVE('',#13296,#13295,#7432,.T.) ;
#16732 = EDGE_CURVE('',#13296,#13293,#7433,.T.) ;
#16733 = EDGE_CURVE('',#13297,#13290,#7434,.T.) ;
#16734 = EDGE_CURVE('',#13298,#13297,#7435,.T.) ;
#16735 = EDGE_CURVE('',#13298,#13287,#7436,.T.) ;
#16736 = EDGE_CURVE('',#13295,#13298,#7437,.T.) ;
#16737 = EDGE_CURVE('',#13297,#13296,#7438,.T.) ;
#16738 = EDGE_CURVE('',#13294,#13287,#7439,.T.) ;
#16739 = EDGE_CURVE('',#13288,#13292,#7440,.T.) ;
#16740 = EDGE_CURVE('',#13299,#13299,#11103,.T.) ;
#16741 = EDGE_CURVE('',#13299,#13300,#7441,.T.) ;
#16742 = EDGE_CURVE('',#13300,#13300,#11104,.T.) ;
#16743 = EDGE_CURVE('',#13301,#13301,#11105,.T.) ;
#16744 = EDGE_CURVE('',#13301,#13302,#7442,.T.) ;
#16745 = EDGE_CURVE('',#13302,#13302,#11106,.T.) ;
#16746 = EDGE_CURVE('',#13303,#13303,#11107,.T.) ;
#16747 = EDGE_CURVE('',#13303,#13304,#7443,.T.) ;
#16748 = EDGE_CURVE('',#13304,#13304,#11108,.T.) ;
#16749 = EDGE_CURVE('',#13305,#13305,#11109,.T.) ;
#16750 = EDGE_CURVE('',#13305,#13306,#7444,.T.) ;
#16751 = EDGE_CURVE('',#13306,#13306,#11110,.T.) ;
#16752 = EDGE_CURVE('',#13307,#13307,#11111,.T.) ;
#16753 = EDGE_CURVE('',#13307,#13308,#7445,.T.) ;
#16754 = EDGE_CURVE('',#13308,#13308,#11112,.T.) ;
#16755 = EDGE_CURVE('',#13309,#13309,#11113,.T.) ;
#16756 = EDGE_CURVE('',#13309,#13310,#7446,.T.) ;
#16757 = EDGE_CURVE('',#13310,#13310,#11114,.T.) ;
#16758 = EDGE_CURVE('',#13311,#13311,#11115,.T.) ;
#16759 = EDGE_CURVE('',#13311,#13312,#7447,.T.) ;
#16760 = EDGE_CURVE('',#13312,#13312,#11116,.T.) ;
#16761 = EDGE_CURVE('',#13313,#13313,#11117,.T.) ;
#16762 = EDGE_CURVE('',#13313,#13314,#7448,.T.) ;
#16763 = EDGE_CURVE('',#13314,#13314,#11118,.T.) ;
#16764 = EDGE_CURVE('',#13315,#13315,#11119,.T.) ;
#16765 = EDGE_CURVE('',#13315,#13316,#7449,.T.) ;
#16766 = EDGE_CURVE('',#13316,#13316,#11120,.T.) ;
#16767 = EDGE_CURVE('',#13317,#13317,#11121,.T.) ;
#16768 = EDGE_CURVE('',#13318,#13318,#11122,.T.) ;
#16769 = EDGE_CURVE('',#13319,#13319,#11123,.T.) ;
#16770 = EDGE_CURVE('',#13320,#13320,#11124,.T.) ;
#16771 = EDGE_CURVE('',#13319,#13317,#7450,.T.) ;
#16772 = EDGE_CURVE('',#13321,#13321,#11125,.T.) ;
#16773 = EDGE_CURVE('',#13321,#13322,#7451,.T.) ;
#16774 = EDGE_CURVE('',#13322,#13323,#11126,.T.) ;
#16775 = EDGE_CURVE('',#13323,#13324,#7452,.T.) ;
#16776 = EDGE_CURVE('',#13324,#13325,#11127,.T.) ;
#16777 = EDGE_CURVE('',#13325,#13326,#7453,.T.) ;
#16778 = EDGE_CURVE('',#13326,#13327,#11128,.T.) ;
#16779 = EDGE_CURVE('',#13327,#13328,#7454,.T.) ;
#16780 = EDGE_CURVE('',#13328,#13329,#11129,.T.) ;
#16781 = EDGE_CURVE('',#13329,#13320,#7455,.T.) ;
#16782 = EDGE_CURVE('',#13329,#13330,#11130,.T.) ;
#16783 = EDGE_CURVE('',#13330,#13331,#7456,.T.) ;
#16784 = EDGE_CURVE('',#13331,#13326,#11131,.T.) ;
#16785 = EDGE_CURVE('',#13325,#13332,#11132,.T.) ;
#16786 = EDGE_CURVE('',#13332,#13333,#7457,.T.) ;
#16787 = EDGE_CURVE('',#13333,#13322,#11133,.T.) ;
#16788 = EDGE_CURVE('',#13334,#13335,#7458,.T.) ;
#16789 = EDGE_CURVE('',#13335,#13336,#11134,.T.) ;
#16790 = EDGE_CURVE('',#13336,#13337,#7459,.T.) ;
#16791 = EDGE_CURVE('',#13337,#13334,#11135,.T.) ;
#16792 = EDGE_CURVE('',#13338,#13339,#7460,.T.) ;
#16793 = EDGE_CURVE('',#13339,#13340,#11136,.T.) ;
#16794 = EDGE_CURVE('',#13340,#13341,#7461,.T.) ;
#16795 = EDGE_CURVE('',#13341,#13338,#11137,.T.) ;
#16796 = EDGE_CURVE('',#13342,#13343,#7462,.T.) ;
#16797 = EDGE_CURVE('',#13343,#13344,#11138,.T.) ;
#16798 = EDGE_CURVE('',#13344,#13345,#7463,.T.) ;
#16799 = EDGE_CURVE('',#13345,#13342,#11139,.T.) ;
#16800 = EDGE_CURVE('',#13346,#13347,#7464,.T.) ;
#16801 = EDGE_CURVE('',#13347,#13348,#11140,.T.) ;
#16802 = EDGE_CURVE('',#13348,#13349,#7465,.T.) ;
#16803 = EDGE_CURVE('',#13349,#13346,#11141,.T.) ;
#16804 = EDGE_CURVE('',#13350,#13351,#7466,.T.) ;
#16805 = EDGE_CURVE('',#13351,#13352,#11142,.T.) ;
#16806 = EDGE_CURVE('',#13352,#13353,#7467,.T.) ;
#16807 = EDGE_CURVE('',#13353,#13350,#11143,.T.) ;
#16808 = EDGE_CURVE('',#13354,#13355,#7468,.T.) ;
#16809 = EDGE_CURVE('',#13355,#13356,#11144,.T.) ;
#16810 = EDGE_CURVE('',#13356,#13357,#7469,.T.) ;
#16811 = EDGE_CURVE('',#13357,#13354,#11145,.T.) ;
#16812 = EDGE_CURVE('',#13352,#13358,#7470,.T.) ;
#16813 = EDGE_CURVE('',#13358,#13359,#7471,.T.) ;
#16814 = EDGE_CURVE('',#13359,#13353,#7472,.T.) ;
#16815 = EDGE_CURVE('',#13360,#13351,#7473,.T.) ;
#16816 = EDGE_CURVE('',#13358,#13360,#7474,.T.) ;
#16817 = EDGE_CURVE('',#13359,#13361,#7475,.T.) ;
#16818 = EDGE_CURVE('',#13350,#13361,#7476,.T.) ;
#16819 = EDGE_CURVE('',#13362,#13355,#7477,.T.) ;
#16820 = EDGE_CURVE('',#13363,#13362,#7478,.T.) ;
#16821 = EDGE_CURVE('',#13356,#13363,#7479,.T.) ;
#16822 = EDGE_CURVE('',#13361,#13360,#7480,.T.) ;
#16823 = EDGE_CURVE('',#13354,#13364,#7481,.T.) ;
#16824 = EDGE_CURVE('',#13364,#13362,#7482,.T.) ;
#16825 = EDGE_CURVE('',#13363,#13365,#7483,.T.) ;
#16826 = EDGE_CURVE('',#13365,#13357,#7484,.T.) ;
#16827 = EDGE_CURVE('',#13365,#13364,#7485,.T.) ;
#16828 = EDGE_CURVE('',#13348,#13366,#7486,.T.) ;
#16829 = EDGE_CURVE('',#13366,#13367,#7487,.T.) ;
#16830 = EDGE_CURVE('',#13367,#13349,#7488,.T.) ;
#16831 = EDGE_CURVE('',#13368,#13347,#7489,.T.) ;
#16832 = EDGE_CURVE('',#13366,#13368,#7490,.T.) ;
#16833 = EDGE_CURVE('',#13367,#13369,#7491,.T.) ;
#16834 = EDGE_CURVE('',#13346,#13369,#7492,.T.) ;
#16835 = EDGE_CURVE('',#13370,#13333,#7493,.T.) ;
#16836 = EDGE_CURVE('',#13371,#13370,#7494,.T.) ;
#16837 = EDGE_CURVE('',#13323,#13371,#7495,.T.) ;
#16838 = EDGE_CURVE('',#13369,#13368,#7496,.T.) ;
#16839 = EDGE_CURVE('',#13332,#13372,#7497,.T.) ;
#16840 = EDGE_CURVE('',#13372,#13370,#7498,.T.) ;
#16841 = EDGE_CURVE('',#13371,#13373,#7499,.T.) ;
#16842 = EDGE_CURVE('',#13373,#13324,#7500,.T.) ;
#16843 = EDGE_CURVE('',#13373,#13372,#7501,.T.) ;
#16844 = EDGE_CURVE('',#13340,#13374,#7502,.T.) ;
#16845 = EDGE_CURVE('',#13374,#13375,#7503,.T.) ;
#16846 = EDGE_CURVE('',#13375,#13341,#7504,.T.) ;
#16847 = EDGE_CURVE('',#13376,#13339,#7505,.T.) ;
#16848 = EDGE_CURVE('',#13374,#13376,#7506,.T.) ;
#16849 = EDGE_CURVE('',#13375,#13377,#7507,.T.) ;
#16850 = EDGE_CURVE('',#13338,#13377,#7508,.T.) ;
#16851 = EDGE_CURVE('',#13378,#13343,#7509,.T.) ;
#16852 = EDGE_CURVE('',#13379,#13378,#7510,.T.) ;
#16853 = EDGE_CURVE('',#13344,#13379,#7511,.T.) ;
#16854 = EDGE_CURVE('',#13377,#13376,#7512,.T.) ;
#16855 = EDGE_CURVE('',#13342,#13380,#7513,.T.) ;
#16856 = EDGE_CURVE('',#13380,#13378,#7514,.T.) ;
#16857 = EDGE_CURVE('',#13379,#13381,#7515,.T.) ;
#16858 = EDGE_CURVE('',#13381,#13345,#7516,.T.) ;
#16859 = EDGE_CURVE('',#13381,#13380,#7517,.T.) ;
#16860 = EDGE_CURVE('',#13336,#13382,#7518,.T.) ;
#16861 = EDGE_CURVE('',#13382,#13383,#7519,.T.) ;
#16862 = EDGE_CURVE('',#13383,#13337,#7520,.T.) ;
#16863 = EDGE_CURVE('',#13384,#13335,#7521,.T.) ;
#16864 = EDGE_CURVE('',#13382,#13384,#7522,.T.) ;
#16865 = EDGE_CURVE('',#13383,#13385,#7523,.T.) ;
#16866 = EDGE_CURVE('',#13334,#13385,#7524,.T.) ;
#16867 = EDGE_CURVE('',#13386,#13331,#7525,.T.) ;
#16868 = EDGE_CURVE('',#13387,#13386,#7526,.T.) ;
#16869 = EDGE_CURVE('',#13327,#13387,#7527,.T.) ;
#16870 = EDGE_CURVE('',#13385,#13384,#7528,.T.) ;
#16871 = EDGE_CURVE('',#13330,#13388,#7529,.T.) ;
#16872 = EDGE_CURVE('',#13388,#13386,#7530,.T.) ;
#16873 = EDGE_CURVE('',#13387,#13389,#7531,.T.) ;
#16874 = EDGE_CURVE('',#13389,#13328,#7532,.T.) ;
#16875 = EDGE_CURVE('',#13389,#13388,#7533,.T.) ;
#16876 = EDGE_CURVE('',#13318,#13390,#7534,.T.) ;
#16877 = EDGE_CURVE('',#13390,#13390,#11146,.T.) ;
#16878 = EDGE_CURVE('',#13391,#13391,#11147,.T.) ;
#16879 = EDGE_CURVE('',#13391,#13392,#7535,.T.) ;
#16880 = EDGE_CURVE('',#13392,#13392,#11148,.T.) ;
#16881 = EDGE_CURVE('',#13393,#13393,#11149,.T.) ;
#16882 = EDGE_CURVE('',#13393,#13394,#7536,.T.) ;
#16883 = EDGE_CURVE('',#13394,#13394,#11150,.T.) ;
#16884 = EDGE_CURVE('',#13395,#13395,#11151,.T.) ;
#16885 = EDGE_CURVE('',#13395,#13396,#7537,.T.) ;
#16886 = EDGE_CURVE('',#13396,#13396,#11152,.T.) ;
#16887 = EDGE_CURVE('',#13397,#13398,#7538,.T.) ;
#16888 = EDGE_CURVE('',#13397,#13399,#7539,.T.) ;
#16889 = EDGE_CURVE('',#13399,#13400,#7540,.T.) ;
#16890 = EDGE_CURVE('',#13400,#13398,#7541,.T.) ;
#16891 = EDGE_CURVE('',#13401,#13400,#7542,.T.) ;
#16892 = EDGE_CURVE('',#13402,#13399,#7543,.T.) ;
#16893 = EDGE_CURVE('',#13401,#13402,#7544,.T.) ;
#16894 = EDGE_CURVE('',#13403,#13404,#7545,.T.) ;
#16895 = EDGE_CURVE('',#13405,#13404,#7546,.T.) ;
#16896 = EDGE_CURVE('',#13398,#13405,#7547,.T.) ;
#16897 = EDGE_CURVE('',#13403,#13401,#7548,.T.) ;
#16898 = EDGE_CURVE('',#13406,#13407,#7549,.T.) ;
#16899 = EDGE_CURVE('',#13404,#13407,#7550,.T.) ;
#16900 = EDGE_CURVE('',#13406,#13403,#7551,.T.) ;
#16901 = EDGE_CURVE('',#13402,#13406,#7552,.T.) ;
#16902 = EDGE_CURVE('',#13397,#13408,#7553,.T.) ;
#16903 = EDGE_CURVE('',#13407,#13408,#7554,.T.) ;
#16904 = EDGE_CURVE('',#13408,#13405,#7555,.T.) ;
#16905 = EDGE_CURVE('',#13409,#13409,#11153,.T.) ;
#16906 = EDGE_CURVE('',#13409,#13410,#7556,.T.) ;
#16907 = EDGE_CURVE('',#13410,#13410,#11154,.T.) ;
#16908 = EDGE_CURVE('',#13411,#13412,#7557,.T.) ;
#16909 = EDGE_CURVE('',#13412,#13413,#7558,.T.) ;
#16910 = EDGE_CURVE('',#13413,#13414,#7559,.T.) ;
#16911 = EDGE_CURVE('',#13414,#13411,#7560,.T.) ;
#16912 = EDGE_CURVE('',#13414,#13415,#7561,.T.) ;
#16913 = EDGE_CURVE('',#13416,#13415,#7562,.T.) ;
#16914 = EDGE_CURVE('',#13411,#13416,#7563,.T.) ;
#16915 = EDGE_CURVE('',#13413,#13417,#7564,.T.) ;
#16916 = EDGE_CURVE('',#13415,#13417,#7565,.T.) ;
#16917 = EDGE_CURVE('',#13412,#13418,#7566,.T.) ;
#16918 = EDGE_CURVE('',#13417,#13418,#7567,.T.) ;
#16919 = EDGE_CURVE('',#13418,#13416,#7568,.T.) ;
#16920 = EDGE_CURVE('',#13419,#13419,#11155,.T.) ;
#16921 = EDGE_CURVE('',#13419,#13420,#7569,.T.) ;
#16922 = EDGE_CURVE('',#13420,#13420,#11156,.T.) ;
#16923 = EDGE_CURVE('',#13421,#13421,#11157,.T.) ;
#16924 = EDGE_CURVE('',#13421,#13422,#7570,.T.) ;
#16925 = EDGE_CURVE('',#13422,#13422,#11158,.T.) ;
#16926 = EDGE_CURVE('',#13423,#13423,#11159,.T.) ;
#16927 = EDGE_CURVE('',#13423,#13424,#7571,.T.) ;
#16928 = EDGE_CURVE('',#13424,#13424,#11160,.T.) ;
#16929 = EDGE_CURVE('',#13425,#13425,#11161,.T.) ;
#16930 = EDGE_CURVE('',#13425,#13426,#7572,.T.) ;
#16931 = EDGE_CURVE('',#13426,#13426,#11162,.T.) ;
#16932 = EDGE_CURVE('',#13427,#13427,#11163,.T.) ;
#16933 = EDGE_CURVE('',#13427,#13428,#7573,.T.) ;
#16934 = EDGE_CURVE('',#13429,#13428,#11164,.T.) ;
#16935 = EDGE_CURVE('',#13430,#13429,#7574,.T.) ;
#16936 = EDGE_CURVE('',#13431,#13430,#11165,.T.) ;
#16937 = EDGE_CURVE('',#13432,#13431,#7575,.T.) ;
#16938 = EDGE_CURVE('',#13428,#13432,#11166,.T.) ;
#16939 = EDGE_CURVE('',#13432,#13433,#7576,.T.) ;
#16940 = EDGE_CURVE('',#13433,#13434,#7577,.T.) ;
#16941 = EDGE_CURVE('',#13434,#13435,#7578,.T.) ;
#16942 = EDGE_CURVE('',#13435,#13436,#7579,.T.) ;
#16943 = EDGE_CURVE('',#13436,#13437,#7580,.T.) ;
#16944 = EDGE_CURVE('',#13437,#13438,#7581,.T.) ;
#16945 = EDGE_CURVE('',#13438,#13439,#7582,.T.) ;
#16946 = EDGE_CURVE('',#13439,#13440,#11167,.T.) ;
#16947 = EDGE_CURVE('',#13440,#13441,#11168,.T.) ;
#16948 = EDGE_CURVE('',#13441,#13442,#11169,.T.) ;
#16949 = EDGE_CURVE('',#13442,#13443,#7583,.T.) ;
#16950 = EDGE_CURVE('',#13443,#13444,#7584,.T.) ;
#16951 = EDGE_CURVE('',#13444,#13445,#7585,.T.) ;
#16952 = EDGE_CURVE('',#13445,#13446,#7586,.T.) ;
#16953 = EDGE_CURVE('',#13446,#13447,#7587,.T.) ;
#16954 = EDGE_CURVE('',#13447,#13448,#7588,.T.) ;
#16955 = EDGE_CURVE('',#13448,#13429,#7589,.T.) ;
#16956 = EDGE_CURVE('',#13449,#13431,#7590,.T.) ;
#16957 = EDGE_CURVE('',#13449,#13433,#7591,.T.) ;
#16958 = EDGE_CURVE('',#13450,#13451,#11170,.T.) ;
#16959 = EDGE_CURVE('',#13451,#13452,#7592,.T.) ;
#16960 = EDGE_CURVE('',#13452,#13453,#7593,.T.) ;
#16961 = EDGE_CURVE('',#13453,#13454,#7594,.T.) ;
#16962 = EDGE_CURVE('',#13454,#13455,#7595,.T.) ;
#16963 = EDGE_CURVE('',#13455,#13450,#7596,.T.) ;
#16964 = EDGE_CURVE('',#13451,#13439,#7597,.T.) ;
#16965 = EDGE_CURVE('',#13452,#13438,#7598,.T.) ;
#16966 = EDGE_CURVE('',#13453,#13437,#7599,.T.) ;
#16967 = EDGE_CURVE('',#13442,#13450,#7600,.T.) ;
#16968 = EDGE_CURVE('',#13455,#13443,#7601,.T.) ;
#16969 = EDGE_CURVE('',#13454,#13444,#7602,.T.) ;
#16970 = EDGE_CURVE('',#13430,#13456,#7603,.T.) ;
#16971 = EDGE_CURVE('',#13456,#13457,#7604,.T.) ;
#16972 = EDGE_CURVE('',#13457,#13458,#7605,.T.) ;
#16973 = EDGE_CURVE('',#13458,#13449,#7606,.T.) ;
#16974 = EDGE_CURVE('',#13456,#13448,#7607,.T.) ;
#16975 = EDGE_CURVE('',#13458,#13434,#7608,.T.) ;
#16976 = EDGE_CURVE('',#13457,#13447,#7609,.T.) ;
#16977 = EDGE_CURVE('',#13459,#13441,#7610,.T.) ;
#16978 = EDGE_CURVE('',#13460,#13459,#11171,.T.) ;
#16979 = EDGE_CURVE('',#13440,#13460,#7611,.T.) ;
#16980 = EDGE_CURVE('',#13461,#13462,#7612,.T.) ;
#16981 = EDGE_CURVE('',#13462,#13463,#7613,.T.) ;
#16982 = EDGE_CURVE('',#13463,#13464,#7614,.T.) ;
#16983 = EDGE_CURVE('',#13464,#13461,#7615,.T.) ;
#16984 = EDGE_CURVE('',#13459,#13460,#11172,.T.) ;
#16985 = EDGE_CURVE('',#13436,#13463,#7616,.T.) ;
#16986 = EDGE_CURVE('',#13445,#13462,#7617,.T.) ;
#16987 = EDGE_CURVE('',#13435,#13464,#7618,.T.) ;
#16988 = EDGE_CURVE('',#13446,#13461,#7619,.T.) ;
#16989 = EDGE_CURVE('',#13465,#13466,#7620,.T.) ;
#16990 = EDGE_CURVE('',#13467,#13465,#7621,.T.) ;
#16991 = EDGE_CURVE('',#13468,#13467,#7622,.T.) ;
#16992 = EDGE_CURVE('',#13466,#13468,#7623,.T.) ;
#16993 = EDGE_CURVE('',#13469,#13467,#7624,.T.) ;
#16994 = EDGE_CURVE('',#13470,#13469,#7625,.T.) ;
#16995 = EDGE_CURVE('',#13468,#13470,#7626,.T.) ;
#16996 = EDGE_CURVE('',#13471,#13472,#7627,.T.) ;
#16997 = EDGE_CURVE('',#13472,#13473,#7628,.T.) ;
#16998 = EDGE_CURVE('',#13473,#13466,#7629,.T.) ;
#16999 = EDGE_CURVE('',#13470,#13471,#7630,.T.) ;
#17000 = EDGE_CURVE('',#13474,#13475,#7631,.T.) ;
#17001 = EDGE_CURVE('',#13472,#13474,#7632,.T.) ;
#17002 = EDGE_CURVE('',#13471,#13476,#7633,.T.) ;
#17003 = EDGE_CURVE('',#13475,#13476,#7634,.T.) ;
#17004 = EDGE_CURVE('',#13477,#13475,#7635,.T.) ;
#17005 = EDGE_CURVE('',#13476,#13469,#7636,.T.) ;
#17006 = EDGE_CURVE('',#13465,#13477,#7637,.T.) ;
#17007 = EDGE_CURVE('',#13478,#13474,#7638,.T.) ;
#17008 = EDGE_CURVE('',#13473,#13478,#7639,.T.) ;
#17009 = EDGE_CURVE('',#13479,#13479,#11173,.T.) ;
#17010 = EDGE_CURVE('',#13479,#13480,#7640,.T.) ;
#17011 = EDGE_CURVE('',#13480,#13480,#11174,.T.) ;
#17012 = EDGE_CURVE('',#13481,#13482,#7641,.T.) ;
#17013 = EDGE_CURVE('',#13483,#13481,#7642,.T.) ;
#17014 = EDGE_CURVE('',#13484,#13483,#7643,.T.) ;
#17015 = EDGE_CURVE('',#13482,#13484,#7644,.T.) ;
#17016 = EDGE_CURVE('',#13485,#13486,#7645,.T.) ;
#17017 = EDGE_CURVE('',#13487,#13486,#7646,.T.) ;
#17018 = EDGE_CURVE('',#13488,#13487,#7647,.T.) ;
#17019 = EDGE_CURVE('',#13485,#13488,#7648,.T.) ;
#17020 = EDGE_CURVE('',#13486,#13483,#7649,.T.) ;
#17021 = EDGE_CURVE('',#13484,#13485,#7650,.T.) ;
#17022 = EDGE_CURVE('',#13489,#13482,#7651,.T.) ;
#17023 = EDGE_CURVE('',#13489,#13490,#7652,.T.) ;
#17024 = EDGE_CURVE('',#13481,#13490,#7653,.T.) ;
#17025 = EDGE_CURVE('',#13491,#13487,#7654,.T.) ;
#17026 = EDGE_CURVE('',#13477,#13491,#7655,.T.) ;
#17027 = EDGE_CURVE('',#13488,#13478,#7656,.T.) ;
#17028 = EDGE_CURVE('',#13492,#13492,#11175,.T.) ;
#17029 = EDGE_CURVE('',#13492,#13493,#7657,.T.) ;
#17030 = EDGE_CURVE('',#13493,#13493,#11176,.T.) ;
#17031 = EDGE_CURVE('',#13494,#13495,#7658,.T.) ;
#17032 = EDGE_CURVE('',#13496,#13495,#7659,.T.) ;
#17033 = EDGE_CURVE('',#13497,#13496,#7660,.T.) ;
#17034 = EDGE_CURVE('',#13494,#13497,#7661,.T.) ;
#17035 = EDGE_CURVE('',#13498,#13499,#7662,.T.) ;
#17036 = EDGE_CURVE('',#13495,#13499,#7663,.T.) ;
#17037 = EDGE_CURVE('',#13498,#13494,#7664,.T.) ;
#17038 = EDGE_CURVE('',#13500,#13501,#7665,.T.) ;
#17039 = EDGE_CURVE('',#13499,#13500,#7666,.T.) ;
#17040 = EDGE_CURVE('',#13501,#13498,#7667,.T.) ;
#17041 = EDGE_CURVE('',#13502,#13501,#7668,.T.) ;
#17042 = EDGE_CURVE('',#13502,#13503,#7669,.T.) ;
#17043 = EDGE_CURVE('',#13500,#13503,#7670,.T.) ;
#17044 = EDGE_CURVE('',#13504,#13496,#7671,.T.) ;
#17045 = EDGE_CURVE('',#13505,#13504,#7672,.T.) ;
#17046 = EDGE_CURVE('',#13497,#13505,#7673,.T.) ;
#17047 = EDGE_CURVE('',#13506,#13506,#11177,.T.) ;
#17048 = EDGE_CURVE('',#13506,#13507,#7674,.T.) ;
#17049 = EDGE_CURVE('',#13507,#13507,#11178,.T.) ;
#17050 = EDGE_CURVE('',#13475,#13502,#7675,.T.) ;
#17051 = EDGE_CURVE('',#13505,#13489,#7676,.T.) ;
#17052 = EDGE_CURVE('',#13490,#13504,#7677,.T.) ;
#17053 = EDGE_CURVE('',#13503,#13491,#7678,.T.) ;
#17054 = EDGE_CURVE('',#13508,#13509,#7679,.T.) ;
#17055 = EDGE_CURVE('',#13510,#13508,#7680,.T.) ;
#17056 = EDGE_CURVE('',#13511,#13510,#7681,.T.) ;
#17057 = EDGE_CURVE('',#13509,#13511,#7682,.T.) ;
#17058 = EDGE_CURVE('',#13509,#13512,#7683,.T.) ;
#17059 = EDGE_CURVE('',#13513,#13511,#7684,.T.) ;
#17060 = EDGE_CURVE('',#13512,#13513,#7685,.T.) ;
#17061 = EDGE_CURVE('',#13513,#13514,#7686,.T.) ;
#17062 = EDGE_CURVE('',#13514,#13510,#7687,.T.) ;
#17063 = EDGE_CURVE('',#13515,#13508,#7688,.T.) ;
#17064 = EDGE_CURVE('',#13514,#13515,#7689,.T.) ;
#17065 = EDGE_CURVE('',#13516,#13512,#7690,.T.) ;
#17066 = EDGE_CURVE('',#13516,#13517,#7691,.T.) ;
#17067 = EDGE_CURVE('',#13517,#13518,#7692,.T.) ;
#17068 = EDGE_CURVE('',#13518,#13519,#7693,.T.) ;
#17069 = EDGE_CURVE('',#13520,#13519,#7694,.T.) ;
#17070 = EDGE_CURVE('',#13520,#13521,#7695,.T.) ;
#17071 = EDGE_CURVE('',#13521,#13522,#7696,.T.) ;
#17072 = EDGE_CURVE('',#13522,#13523,#7697,.T.) ;
#17073 = EDGE_CURVE('',#13524,#13523,#7698,.T.) ;
#17074 = EDGE_CURVE('',#13524,#13525,#7699,.T.) ;
#17075 = EDGE_CURVE('',#13525,#13526,#7700,.T.) ;
#17076 = EDGE_CURVE('',#13526,#13527,#7701,.T.) ;
#17077 = EDGE_CURVE('',#13528,#13527,#7702,.T.) ;
#17078 = EDGE_CURVE('',#13528,#13529,#7703,.T.) ;
#17079 = EDGE_CURVE('',#13529,#13530,#7704,.T.) ;
#17080 = EDGE_CURVE('',#13530,#13531,#7705,.T.) ;
#17081 = EDGE_CURVE('',#13532,#13531,#7706,.T.) ;
#17082 = EDGE_CURVE('',#13532,#13533,#7707,.T.) ;
#17083 = EDGE_CURVE('',#13533,#13534,#7708,.T.) ;
#17084 = EDGE_CURVE('',#13534,#13535,#7709,.T.) ;
#17085 = EDGE_CURVE('',#13536,#13535,#7710,.T.) ;
#17086 = EDGE_CURVE('',#13536,#13537,#7711,.T.) ;
#17087 = EDGE_CURVE('',#13537,#13538,#7712,.T.) ;
#17088 = EDGE_CURVE('',#13538,#13539,#7713,.T.) ;
#17089 = EDGE_CURVE('',#13540,#13539,#7714,.T.) ;
#17090 = EDGE_CURVE('',#13540,#13541,#7715,.T.) ;
#17091 = EDGE_CURVE('',#13541,#13542,#7716,.T.) ;
#17092 = EDGE_CURVE('',#13542,#13543,#7717,.T.) ;
#17093 = EDGE_CURVE('',#13544,#13543,#7718,.T.) ;
#17094 = EDGE_CURVE('',#13544,#13545,#7719,.T.) ;
#17095 = EDGE_CURVE('',#13545,#13546,#7720,.T.) ;
#17096 = EDGE_CURVE('',#13546,#13547,#7721,.T.) ;
#17097 = EDGE_CURVE('',#13548,#13547,#7722,.T.) ;
#17098 = EDGE_CURVE('',#13548,#13549,#7723,.T.) ;
#17099 = EDGE_CURVE('',#13550,#13549,#7724,.T.) ;
#17100 = EDGE_CURVE('',#13551,#13550,#7725,.T.) ;
#17101 = EDGE_CURVE('',#13515,#13551,#7726,.T.) ;
#17102 = EDGE_CURVE('',#13552,#13553,#7727,.T.) ;
#17103 = EDGE_CURVE('',#13552,#13554,#7728,.T.) ;
#17104 = EDGE_CURVE('',#13554,#13555,#7729,.T.) ;
#17105 = EDGE_CURVE('',#13553,#13555,#7730,.T.) ;
#17106 = EDGE_CURVE('',#13553,#13516,#7731,.T.) ;
#17107 = EDGE_CURVE('',#13555,#13517,#7732,.T.) ;
#17108 = EDGE_CURVE('',#13518,#13554,#7733,.T.) ;
#17109 = EDGE_CURVE('',#13519,#13552,#7734,.T.) ;
#17110 = EDGE_CURVE('',#13551,#13556,#7735,.T.) ;
#17111 = EDGE_CURVE('',#13556,#13557,#7736,.T.) ;
#17112 = EDGE_CURVE('',#13557,#13548,#7737,.T.) ;
#17113 = EDGE_CURVE('',#13547,#13558,#7738,.T.) ;
#17114 = EDGE_CURVE('',#13558,#13559,#7739,.T.) ;
#17115 = EDGE_CURVE('',#13559,#13544,#7740,.T.) ;
#17116 = EDGE_CURVE('',#13543,#13560,#7741,.T.) ;
#17117 = EDGE_CURVE('',#13560,#13561,#7742,.T.) ;
#17118 = EDGE_CURVE('',#13561,#13540,#7743,.T.) ;
#17119 = EDGE_CURVE('',#13539,#13562,#7744,.T.) ;
#17120 = EDGE_CURVE('',#13562,#13563,#7745,.T.) ;
#17121 = EDGE_CURVE('',#13563,#13536,#7746,.T.) ;
#17122 = EDGE_CURVE('',#13535,#13564,#7747,.T.) ;
#17123 = EDGE_CURVE('',#13564,#13565,#7748,.T.) ;
#17124 = EDGE_CURVE('',#13565,#13532,#7749,.T.) ;
#17125 = EDGE_CURVE('',#13531,#13566,#7750,.T.) ;
#17126 = EDGE_CURVE('',#13566,#13567,#7751,.T.) ;
#17127 = EDGE_CURVE('',#13567,#13528,#7752,.T.) ;
#17128 = EDGE_CURVE('',#13527,#13568,#7753,.T.) ;
#17129 = EDGE_CURVE('',#13568,#13569,#7754,.T.) ;
#17130 = EDGE_CURVE('',#13569,#13524,#7755,.T.) ;
#17131 = EDGE_CURVE('',#13523,#13570,#7756,.T.) ;
#17132 = EDGE_CURVE('',#13570,#13571,#7757,.T.) ;
#17133 = EDGE_CURVE('',#13571,#13520,#7758,.T.) ;
#17134 = EDGE_CURVE('',#13572,#13521,#7759,.T.) ;
#17135 = EDGE_CURVE('',#13573,#13572,#7760,.T.) ;
#17136 = EDGE_CURVE('',#13522,#13573,#7761,.T.) ;
#17137 = EDGE_CURVE('',#13570,#13573,#7762,.T.) ;
#17138 = EDGE_CURVE('',#13571,#13572,#7763,.T.) ;
#17139 = EDGE_CURVE('',#13568,#13574,#7764,.T.) ;
#17140 = EDGE_CURVE('',#13574,#13575,#7765,.T.) ;
#17141 = EDGE_CURVE('',#13569,#13575,#7766,.T.) ;
#17142 = EDGE_CURVE('',#13575,#13525,#7767,.T.) ;
#17143 = EDGE_CURVE('',#13526,#13574,#7768,.T.) ;
#17144 = EDGE_CURVE('',#13576,#13529,#7769,.T.) ;
#17145 = EDGE_CURVE('',#13577,#13576,#7770,.T.) ;
#17146 = EDGE_CURVE('',#13530,#13577,#7771,.T.) ;
#17147 = EDGE_CURVE('',#13566,#13577,#7772,.T.) ;
#17148 = EDGE_CURVE('',#13567,#13576,#7773,.T.) ;
#17149 = EDGE_CURVE('',#13564,#13578,#7774,.T.) ;
#17150 = EDGE_CURVE('',#13578,#13579,#7775,.T.) ;
#17151 = EDGE_CURVE('',#13565,#13579,#7776,.T.) ;
#17152 = EDGE_CURVE('',#13579,#13533,#7777,.T.) ;
#17153 = EDGE_CURVE('',#13534,#13578,#7778,.T.) ;
#17154 = EDGE_CURVE('',#13580,#13537,#7779,.T.) ;
#17155 = EDGE_CURVE('',#13581,#13580,#7780,.T.) ;
#17156 = EDGE_CURVE('',#13538,#13581,#7781,.T.) ;
#17157 = EDGE_CURVE('',#13562,#13581,#7782,.T.) ;
#17158 = EDGE_CURVE('',#13563,#13580,#7783,.T.) ;
#17159 = EDGE_CURVE('',#13560,#13582,#7784,.T.) ;
#17160 = EDGE_CURVE('',#13582,#13583,#7785,.T.) ;
#17161 = EDGE_CURVE('',#13561,#13583,#7786,.T.) ;
#17162 = EDGE_CURVE('',#13583,#13541,#7787,.T.) ;
#17163 = EDGE_CURVE('',#13542,#13582,#7788,.T.) ;
#17164 = EDGE_CURVE('',#13584,#13545,#7789,.T.) ;
#17165 = EDGE_CURVE('',#13585,#13584,#7790,.T.) ;
#17166 = EDGE_CURVE('',#13546,#13585,#7791,.T.) ;
#17167 = EDGE_CURVE('',#13558,#13585,#7792,.T.) ;
#17168 = EDGE_CURVE('',#13559,#13584,#7793,.T.) ;
#17169 = EDGE_CURVE('',#13586,#13550,#7794,.T.) ;
#17170 = EDGE_CURVE('',#13549,#13587,#7795,.T.) ;
#17171 = EDGE_CURVE('',#13587,#13586,#7796,.T.) ;
#17172 = EDGE_CURVE('',#13557,#13587,#7797,.T.) ;
#17173 = EDGE_CURVE('',#13556,#13586,#7798,.T.) ;
#17174 = EDGE_CURVE('',#13588,#13588,#11179,.T.) ;
#17175 = EDGE_CURVE('',#13588,#13589,#7799,.T.) ;
#17176 = EDGE_CURVE('',#13589,#13589,#11180,.T.) ;
#17177 = EDGE_CURVE('',#13590,#13590,#11181,.T.) ;
#17178 = EDGE_CURVE('',#13590,#13591,#7800,.T.) ;
#17179 = EDGE_CURVE('',#13591,#13591,#11182,.T.) ;
#17180 = EDGE_CURVE('',#13592,#13592,#11183,.T.) ;
#17181 = EDGE_CURVE('',#13592,#13593,#7801,.T.) ;
#17182 = EDGE_CURVE('',#13593,#13593,#11184,.T.) ;
#17183 = EDGE_CURVE('',#13594,#13594,#11185,.T.) ;
#17184 = EDGE_CURVE('',#13594,#13595,#7802,.T.) ;
#17185 = EDGE_CURVE('',#13595,#13595,#11186,.T.) ;
#17186 = EDGE_CURVE('',#13596,#13597,#7803,.T.) ;
#17187 = EDGE_CURVE('',#13598,#13596,#11187,.T.) ;
#17188 = EDGE_CURVE('',#13599,#13598,#7804,.T.) ;
#17189 = EDGE_CURVE('',#13597,#13599,#19,.T.) ;
#17190 = EDGE_CURVE('',#13600,#13601,#11188,.T.) ;
#17191 = EDGE_CURVE('',#13601,#13600,#20,.T.) ;
#17192 = EDGE_CURVE('',#13602,#13603,#7805,.T.) ;
#17193 = EDGE_CURVE('',#13603,#13604,#7806,.T.) ;
#17194 = EDGE_CURVE('',#13604,#13605,#7807,.T.) ;
#17195 = EDGE_CURVE('',#13605,#13602,#7808,.T.) ;
#17196 = EDGE_CURVE('',#13596,#13598,#11189,.T.) ;
#17197 = EDGE_CURVE('',#13597,#13606,#11190,.T.) ;
#17198 = EDGE_CURVE('',#13606,#13599,#11191,.T.) ;
#17199 = EDGE_CURVE('',#13607,#13607,#11192,.T.) ;
#17200 = EDGE_CURVE('',#13607,#13608,#7809,.T.) ;
#17201 = EDGE_CURVE('',#13601,#13608,#11193,.T.) ;
#17202 = EDGE_CURVE('',#13608,#13600,#11194,.T.) ;
#17203 = EDGE_CURVE('',#13609,#13610,#7810,.T.) ;
#17204 = EDGE_CURVE('',#13610,#13611,#7811,.T.) ;
#17205 = EDGE_CURVE('',#13611,#13612,#7812,.T.) ;
#17206 = EDGE_CURVE('',#13612,#13609,#7813,.T.) ;
#17207 = EDGE_CURVE('',#13612,#13604,#7814,.T.) ;
#17208 = EDGE_CURVE('',#13609,#13603,#7815,.T.) ;
#17209 = EDGE_CURVE('',#13611,#13605,#7816,.T.) ;
#17210 = EDGE_CURVE('',#13610,#13602,#7817,.T.) ;
#17211 = EDGE_CURVE('',#13606,#13613,#7818,.T.) ;
#17212 = EDGE_CURVE('',#13613,#13613,#11195,.T.) ;
#17213 = EDGE_CURVE('',#13614,#13614,#11196,.T.) ;
#17214 = EDGE_CURVE('',#13614,#13615,#7819,.T.) ;
#17215 = EDGE_CURVE('',#13615,#13615,#11197,.T.) ;
#17216 = EDGE_CURVE('',#13615,#13616,#7820,.T.) ;
#17217 = EDGE_CURVE('',#13616,#13616,#11198,.T.) ;
#17218 = EDGE_CURVE('',#13617,#13617,#11199,.T.) ;
#17219 = EDGE_CURVE('',#13617,#13618,#7821,.T.) ;
#17220 = EDGE_CURVE('',#13618,#13618,#11200,.T.) ;
#17221 = EDGE_CURVE('',#13619,#13619,#11201,.T.) ;
#17222 = EDGE_CURVE('',#13620,#13620,#11202,.T.) ;
#17223 = EDGE_CURVE('',#13621,#13621,#11203,.T.) ;
#17224 = EDGE_CURVE('',#13622,#13622,#11204,.T.) ;
#17225 = EDGE_CURVE('',#13619,#13621,#7822,.T.) ;
#17226 = EDGE_CURVE('',#13622,#13620,#7823,.T.) ;
#17227 = EDGE_CURVE('',#13623,#13623,#11205,.T.) ;
#17228 = EDGE_CURVE('',#13623,#13624,#7824,.T.) ;
#17229 = EDGE_CURVE('',#13624,#13624,#11206,.T.) ;
#17230 = EDGE_CURVE('',#13625,#13625,#11207,.T.) ;
#17231 = EDGE_CURVE('',#13625,#13626,#7825,.T.) ;
#17232 = EDGE_CURVE('',#13626,#13626,#11208,.T.) ;
#17233 = EDGE_CURVE('',#13627,#13627,#11209,.T.) ;
#17234 = EDGE_CURVE('',#13627,#13628,#7826,.T.) ;
#17235 = EDGE_CURVE('',#13628,#13628,#11210,.T.) ;
#17236 = EDGE_CURVE('',#13629,#13629,#11211,.T.) ;
#17237 = EDGE_CURVE('',#13629,#13630,#7827,.T.) ;
#17238 = EDGE_CURVE('',#13630,#13630,#11212,.T.) ;
#17239 = EDGE_CURVE('',#13631,#13631,#11213,.T.) ;
#17240 = EDGE_CURVE('',#13631,#13632,#7828,.T.) ;
#17241 = EDGE_CURVE('',#13632,#13632,#11214,.T.) ;
#17242 = EDGE_CURVE('',#13633,#13633,#11215,.T.) ;
#17243 = EDGE_CURVE('',#13633,#13634,#7829,.T.) ;
#17244 = EDGE_CURVE('',#13634,#13634,#11216,.T.) ;
#17245 = EDGE_CURVE('',#13635,#13635,#11217,.T.) ;
#17246 = EDGE_CURVE('',#13635,#13636,#7830,.T.) ;
#17247 = EDGE_CURVE('',#13636,#13636,#11218,.T.) ;
#17248 = EDGE_CURVE('',#13637,#13637,#11219,.T.) ;
#17249 = EDGE_CURVE('',#13637,#13638,#7831,.T.) ;
#17250 = EDGE_CURVE('',#13638,#13638,#11220,.T.) ;
#17251 = EDGE_CURVE('',#13639,#13640,#7832,.T.) ;
#17252 = EDGE_CURVE('',#13641,#13639,#7833,.T.) ;
#17253 = EDGE_CURVE('',#13642,#13641,#7834,.T.) ;
#17254 = EDGE_CURVE('',#13640,#13642,#7835,.T.) ;
#17255 = EDGE_CURVE('',#13641,#13642,#11221,.T.) ;
#17256 = EDGE_CURVE('',#13640,#13639,#11222,.T.) ;
#17257 = EDGE_CURVE('',#13643,#13644,#11223,.T.) ;
#17258 = EDGE_CURVE('',#13644,#13643,#11224,.T.) ;
#17259 = EDGE_CURVE('',#13644,#13645,#7836,.T.) ;
#17260 = EDGE_CURVE('',#13645,#13645,#11225,.T.) ;
#17261 = EDGE_CURVE('',#13646,#13643,#7837,.T.) ;
#17262 = EDGE_CURVE('',#13647,#13646,#7838,.T.) ;
#17263 = EDGE_CURVE('',#13647,#13644,#7839,.T.) ;
#17264 = EDGE_CURVE('',#13644,#13648,#7840,.T.) ;
#17265 = EDGE_CURVE('',#13648,#13649,#7841,.T.) ;
#17266 = EDGE_CURVE('',#13643,#13649,#7842,.T.) ;
#17267 = EDGE_CURVE('',#13650,#13650,#11226,.T.) ;
#17268 = EDGE_CURVE('',#13650,#13651,#7843,.T.) ;
#17269 = EDGE_CURVE('',#13651,#13651,#11227,.T.) ;
#17270 = EDGE_CURVE('',#13652,#13652,#11228,.T.) ;
#17271 = EDGE_CURVE('',#13653,#13653,#11229,.T.) ;
#17272 = EDGE_CURVE('',#13653,#13652,#7844,.T.) ;
#17273 = EDGE_CURVE('',#13654,#13654,#11230,.T.) ;
#17274 = EDGE_CURVE('',#13654,#13655,#7845,.T.) ;
#17275 = EDGE_CURVE('',#13655,#13655,#11231,.T.) ;
#17276 = EDGE_CURVE('',#13656,#13657,#7846,.T.) ;
#17277 = EDGE_CURVE('',#13657,#13658,#7847,.T.) ;
#17278 = EDGE_CURVE('',#13658,#13659,#7848,.T.) ;
#17279 = EDGE_CURVE('',#13659,#13656,#7849,.T.) ;
#17280 = EDGE_CURVE('',#13660,#13661,#7850,.T.) ;
#17281 = EDGE_CURVE('',#13662,#13660,#7851,.T.) ;
#17282 = EDGE_CURVE('',#13663,#13662,#7852,.T.) ;
#17283 = EDGE_CURVE('',#13661,#13663,#7853,.T.) ;
#17284 = EDGE_CURVE('',#13664,#13665,#7854,.T.) ;
#17285 = EDGE_CURVE('',#13665,#13666,#7855,.T.) ;
#17286 = EDGE_CURVE('',#13666,#13667,#7856,.T.) ;
#17287 = EDGE_CURVE('',#13667,#13664,#7857,.T.) ;
#17288 = EDGE_CURVE('',#13649,#13668,#7858,.T.) ;
#17289 = EDGE_CURVE('',#13669,#13648,#7859,.T.) ;
#17290 = EDGE_CURVE('',#13668,#13669,#7860,.T.) ;
#17291 = EDGE_CURVE('',#13667,#13658,#7861,.T.) ;
#17292 = EDGE_CURVE('',#13664,#13657,#7862,.T.) ;
#17293 = EDGE_CURVE('',#13666,#13659,#7863,.T.) ;
#17294 = EDGE_CURVE('',#13665,#13656,#7864,.T.) ;
#17295 = EDGE_CURVE('',#13670,#13647,#7865,.T.) ;
#17296 = EDGE_CURVE('',#13670,#13669,#7866,.T.) ;
#17297 = EDGE_CURVE('',#13671,#13668,#7867,.T.) ;
#17298 = EDGE_CURVE('',#13646,#13671,#7868,.T.) ;
#17299 = EDGE_CURVE('',#13671,#13670,#7869,.T.) ;
#17300 = EDGE_CURVE('',#13662,#13672,#7870,.T.) ;
#17301 = EDGE_CURVE('',#13673,#13672,#7871,.T.) ;
#17302 = EDGE_CURVE('',#13663,#13673,#7872,.T.) ;
#17303 = EDGE_CURVE('',#13660,#13674,#7873,.T.) ;
#17304 = EDGE_CURVE('',#13672,#13674,#7874,.T.) ;
#17305 = EDGE_CURVE('',#13661,#13675,#7875,.T.) ;
#17306 = EDGE_CURVE('',#13674,#13675,#7876,.T.) ;
#17307 = EDGE_CURVE('',#13675,#13673,#7877,.T.) ;
#17308 = EDGE_CURVE('',#13676,#13676,#11232,.T.) ;
#17309 = EDGE_CURVE('',#13676,#13677,#7878,.T.) ;
#17310 = EDGE_CURVE('',#13677,#13677,#11233,.T.) ;
#17311 = EDGE_CURVE('',#13678,#13676,#11234,.T.) ;
#17312 = EDGE_CURVE('',#13679,#13679,#11235,.T.) ;
#17313 = EDGE_CURVE('',#13680,#13680,#11236,.T.) ;
#17314 = EDGE_CURVE('',#13679,#13681,#7879,.T.) ;
#17315 = EDGE_CURVE('',#13681,#13681,#11237,.T.) ;
#17316 = EDGE_CURVE('',#13682,#13682,#11238,.T.) ;
#17317 = EDGE_CURVE('',#13682,#13680,#7880,.T.) ;
#17318 = EDGE_CURVE('',#13683,#13684,#11239,.T.) ;
#17319 = EDGE_CURVE('',#13685,#13686,#11240,.T.) ;
#17320 = EDGE_CURVE('',#13687,#13688,#11241,.T.) ;
#17321 = EDGE_CURVE('',#13689,#13689,#11242,.T.) ;
#17322 = EDGE_CURVE('',#13690,#13690,#11243,.T.) ;
#17323 = EDGE_CURVE('',#13690,#13689,#7881,.T.) ;
#17324 = EDGE_CURVE('',#13691,#13692,#11244,.T.) ;
#17325 = EDGE_CURVE('',#13692,#13691,#11245,.T.) ;
#17326 = EDGE_CURVE('',#13693,#13694,#11246,.T.) ;
#17327 = EDGE_CURVE('',#13694,#13695,#11247,.T.) ;
#17328 = EDGE_CURVE('',#13695,#13696,#11248,.T.) ;
#17329 = EDGE_CURVE('',#13696,#13693,#11249,.T.) ;
#17330 = EDGE_CURVE('',#13697,#13698,#11250,.T.) ;
#17331 = EDGE_CURVE('',#13697,#13698,#11251,.T.) ;
#17332 = EDGE_CURVE('',#13699,#13700,#11252,.T.) ;
#17333 = EDGE_CURVE('',#13700,#13701,#11253,.T.) ;
#17334 = EDGE_CURVE('',#13701,#13699,#11254,.T.) ;
#17335 = EDGE_CURVE('',#13702,#13702,#11255,.T.) ;
#17336 = EDGE_CURVE('',#13702,#13703,#7882,.T.) ;
#17337 = EDGE_CURVE('',#13703,#13697,#21,.T.) ;
#17338 = EDGE_CURVE('',#13698,#13703,#22,.T.) ;
#17339 = EDGE_CURVE('',#13704,#13704,#11256,.T.) ;
#17340 = EDGE_CURVE('',#13704,#13705,#7883,.T.) ;
#17341 = EDGE_CURVE('',#13705,#13705,#11257,.T.) ;
#17342 = EDGE_CURVE('',#13706,#13706,#11258,.T.) ;
#17343 = EDGE_CURVE('',#13706,#13707,#7884,.T.) ;
#17344 = EDGE_CURVE('',#13708,#13707,#405,.T.) ;
#17345 = EDGE_CURVE('',#13709,#13708,#11259,.T.) ;
#17346 = EDGE_CURVE('',#13707,#13709,#406,.T.) ;
#17347 = EDGE_CURVE('',#13710,#13709,#11260,.T.) ;
#17348 = EDGE_CURVE('',#13710,#13711,#7885,.T.) ;
#17349 = EDGE_CURVE('',#13692,#13711,#407,.T.) ;
#17350 = EDGE_CURVE('',#13711,#13691,#408,.T.) ;
#17351 = EDGE_CURVE('',#13708,#13710,#11261,.T.) ;
#17352 = EDGE_CURVE('',#13711,#13694,#7886,.T.) ;
#17353 = EDGE_CURVE('',#13695,#13693,#409,.T.) ;
#17354 = EDGE_CURVE('',#13696,#13712,#7887,.T.) ;
#17355 = EDGE_CURVE('',#13713,#13712,#11262,.T.) ;
#17356 = EDGE_CURVE('',#13712,#13713,#410,.T.) ;
#17357 = EDGE_CURVE('',#13712,#13713,#11263,.T.) ;
#17358 = EDGE_CURVE('',#13712,#13700,#7888,.T.) ;
#17359 = EDGE_CURVE('',#13714,#13699,#411,.T.) ;
#17360 = EDGE_CURVE('',#13701,#13714,#412,.T.) ;
#17361 = EDGE_CURVE('',#13714,#13715,#7889,.T.) ;
#17362 = EDGE_CURVE('',#13715,#13715,#11264,.T.) ;
#17363 = EDGE_CURVE('',#13716,#13716,#11265,.T.) ;
#17364 = EDGE_CURVE('',#13717,#13718,#11266,.T.) ;
#17365 = EDGE_CURVE('',#13717,#13719,#11267,.T.) ;
#17366 = EDGE_CURVE('',#13718,#13719,#11268,.T.) ;
#17367 = EDGE_CURVE('',#13718,#13716,#7890,.T.) ;
#17368 = EDGE_CURVE('',#13717,#13719,#23,.T.) ;
#17369 = EDGE_CURVE('',#13720,#13721,#11269,.T.) ;
#17370 = EDGE_CURVE('',#13722,#13723,#11270,.T.) ;
#17371 = EDGE_CURVE('',#13724,#13723,#11271,.T.) ;
#17372 = EDGE_CURVE('',#13722,#13724,#11272,.T.) ;
#17373 = EDGE_CURVE('',#13722,#13723,#24,.T.) ;
#17374 = EDGE_CURVE('',#13725,#13726,#25,.T.) ;
#17375 = EDGE_CURVE('',#13726,#13725,#11273,.T.) ;
#17376 = EDGE_CURVE('',#13724,#13727,#7891,.T.) ;
#17377 = EDGE_CURVE('',#13727,#13725,#11274,.T.) ;
#17378 = EDGE_CURVE('',#13726,#13727,#11275,.T.) ;
#17379 = EDGE_CURVE('',#13728,#13729,#11276,.T.) ;
#17380 = EDGE_CURVE('',#13728,#13730,#11277,.T.) ;
#17381 = EDGE_CURVE('',#13729,#13730,#11278,.T.) ;
#17382 = EDGE_CURVE('',#13731,#13729,#11279,.T.) ;
#17383 = EDGE_CURVE('',#13732,#13733,#26,.T.) ;
#17384 = EDGE_CURVE('',#13732,#13733,#11280,.T.) ;
#17385 = EDGE_CURVE('',#13732,#13734,#11281,.T.) ;
#17386 = EDGE_CURVE('',#13734,#13729,#7892,.T.) ;
#17387 = EDGE_CURVE('',#13730,#13728,#27,.T.) ;
#17388 = EDGE_CURVE('',#13734,#13733,#11282,.T.) ;
#17389 = EDGE_CURVE('',#13735,#13736,#11283,.T.) ;
#17390 = EDGE_CURVE('',#13737,#13738,#413,.T.) ;
#17391 = EDGE_CURVE('',#13739,#13737,#414,.T.) ;
#17392 = EDGE_CURVE('',#13739,#13740,#7893,.T.) ;
#17393 = EDGE_CURVE('',#13740,#13740,#11284,.T.) ;
#17394 = EDGE_CURVE('',#13741,#13739,#415,.T.) ;
#17395 = EDGE_CURVE('',#13742,#13741,#416,.T.) ;
#17396 = EDGE_CURVE('',#13738,#13742,#11285,.T.) ;
#17397 = EDGE_CURVE('',#13738,#13743,#7894,.T.) ;
#17398 = EDGE_CURVE('',#13744,#13742,#7895,.T.) ;
#17399 = EDGE_CURVE('',#13743,#13744,#7896,.T.) ;
#17400 = EDGE_CURVE('',#13744,#13745,#11286,.T.) ;
#17401 = EDGE_CURVE('',#13745,#13743,#11287,.T.) ;
#17402 = EDGE_CURVE('',#13745,#13746,#7897,.T.) ;
#17403 = EDGE_CURVE('',#13746,#13746,#11288,.T.) ;
#17404 = EDGE_CURVE('',#13747,#13747,#11289,.T.) ;
#17405 = EDGE_CURVE('',#13747,#13748,#7898,.T.) ;
#17406 = EDGE_CURVE('',#13748,#13748,#11290,.T.) ;
#17407 = EDGE_CURVE('',#13749,#13749,#11291,.T.) ;
#17408 = EDGE_CURVE('',#13749,#13750,#7899,.T.) ;
#17409 = EDGE_CURVE('',#13750,#13750,#11292,.T.) ;
#17410 = EDGE_CURVE('',#13751,#13751,#11293,.T.) ;
#17411 = EDGE_CURVE('',#13751,#13752,#7900,.T.) ;
#17412 = EDGE_CURVE('',#13752,#13752,#11294,.T.) ;
#17413 = EDGE_CURVE('',#13753,#13753,#11295,.T.) ;
#17414 = EDGE_CURVE('',#13753,#13754,#7901,.T.) ;
#17415 = EDGE_CURVE('',#13754,#13754,#11296,.T.) ;
#17416 = EDGE_CURVE('',#13755,#13756,#28,.T.) ;
#17417 = EDGE_CURVE('',#13756,#13755,#29,.T.) ;
#17418 = EDGE_CURVE('',#13757,#13757,#11297,.T.) ;
#17419 = EDGE_CURVE('',#13757,#13758,#7902,.T.) ;
#17420 = EDGE_CURVE('',#13758,#13758,#11298,.T.) ;
#17421 = EDGE_CURVE('',#13759,#13759,#11299,.T.) ;
#17422 = EDGE_CURVE('',#13759,#13756,#7903,.T.) ;
#17423 = EDGE_CURVE('',#13760,#13760,#11300,.T.) ;
#17424 = EDGE_CURVE('',#13760,#13761,#7904,.T.) ;
#17425 = EDGE_CURVE('',#13761,#13761,#11301,.T.) ;
#17426 = EDGE_CURVE('',#13762,#13762,#11302,.T.) ;
#17427 = EDGE_CURVE('',#13762,#13763,#7905,.T.) ;
#17428 = EDGE_CURVE('',#13763,#13763,#11303,.T.) ;
#17429 = EDGE_CURVE('',#13764,#13765,#417,.T.) ;
#17430 = EDGE_CURVE('',#13766,#13764,#30,.T.) ;
#17431 = EDGE_CURVE('',#13767,#13766,#31,.T.) ;
#17432 = EDGE_CURVE('',#13768,#13767,#32,.T.) ;
#17433 = EDGE_CURVE('',#13765,#13768,#11304,.T.) ;
#17434 = EDGE_CURVE('',#13765,#13769,#7906,.T.) ;
#17435 = EDGE_CURVE('',#13769,#13769,#11305,.T.) ;
#17436 = EDGE_CURVE('',#13770,#13770,#11306,.T.) ;
#17437 = EDGE_CURVE('',#13770,#13771,#7907,.T.) ;
#17438 = EDGE_CURVE('',#13771,#13771,#11307,.T.) ;
#17439 = EDGE_CURVE('',#13765,#13772,#7908,.T.) ;
#17440 = EDGE_CURVE('',#13773,#13768,#418,.T.) ;
#17441 = EDGE_CURVE('',#13774,#13773,#11308,.T.) ;
#17442 = EDGE_CURVE('',#13775,#13774,#419,.T.) ;
#17443 = EDGE_CURVE('',#13776,#13775,#11309,.T.) ;
#17444 = EDGE_CURVE('',#13772,#13776,#420,.T.) ;
#17445 = EDGE_CURVE('',#13772,#13764,#11310,.T.) ;
#17446 = EDGE_CURVE('',#13775,#13777,#11311,.T.) ;
#17447 = EDGE_CURVE('',#13777,#13776,#11312,.T.) ;
#17448 = EDGE_CURVE('',#13773,#13778,#11313,.T.) ;
#17449 = EDGE_CURVE('',#13778,#13779,#11314,.T.) ;
#17450 = EDGE_CURVE('',#13779,#13774,#11315,.T.) ;
#17451 = EDGE_CURVE('',#13780,#13781,#11316,.T.) ;
#17452 = EDGE_CURVE('',#13781,#13782,#11317,.T.) ;
#17453 = EDGE_CURVE('',#13782,#13780,#11318,.T.) ;
#17454 = EDGE_CURVE('',#13783,#13784,#11319,.T.) ;
#17455 = EDGE_CURVE('',#13784,#13785,#11320,.T.) ;
#17456 = EDGE_CURVE('',#13785,#13786,#11321,.T.) ;
#17457 = EDGE_CURVE('',#13785,#13787,#11322,.T.) ;
#17458 = EDGE_CURVE('',#13787,#13783,#11323,.T.) ;
#17459 = EDGE_CURVE('',#13788,#13789,#11324,.T.) ;
#17460 = EDGE_CURVE('',#13789,#13790,#11325,.T.) ;
#17461 = EDGE_CURVE('',#13790,#13788,#11326,.T.) ;
#17462 = EDGE_CURVE('',#13791,#13792,#11327,.T.) ;
#17463 = EDGE_CURVE('',#13792,#13793,#11328,.T.) ;
#17464 = EDGE_CURVE('',#13793,#13791,#11329,.T.) ;
#17465 = EDGE_CURVE('',#13794,#13795,#11330,.T.) ;
#17466 = EDGE_CURVE('',#13795,#13796,#11331,.T.) ;
#17467 = EDGE_CURVE('',#13796,#13794,#11332,.T.) ;
#17468 = EDGE_CURVE('',#13797,#13798,#11333,.T.) ;
#17469 = EDGE_CURVE('',#13798,#13799,#11334,.T.) ;
#17470 = EDGE_CURVE('',#13800,#13799,#11335,.T.) ;
#17471 = EDGE_CURVE('',#13799,#13801,#11336,.T.) ;
#17472 = EDGE_CURVE('',#13801,#13797,#11337,.T.) ;
#17473 = EDGE_CURVE('',#13802,#13803,#11338,.T.) ;
#17474 = EDGE_CURVE('',#13803,#13804,#11339,.T.) ;
#17475 = EDGE_CURVE('',#13804,#13802,#11340,.T.) ;
#17476 = EDGE_CURVE('',#13805,#13806,#11341,.T.) ;
#17477 = EDGE_CURVE('',#13806,#13807,#11342,.T.) ;
#17478 = EDGE_CURVE('',#13807,#13805,#11343,.T.) ;
#17479 = EDGE_CURVE('',#13808,#13809,#11344,.T.) ;
#17480 = EDGE_CURVE('',#13809,#13810,#11345,.T.) ;
#17481 = EDGE_CURVE('',#13810,#13808,#11346,.T.) ;
#17482 = EDGE_CURVE('',#13811,#13812,#11347,.T.) ;
#17483 = EDGE_CURVE('',#13812,#13813,#11348,.T.) ;
#17484 = EDGE_CURVE('',#13813,#13814,#11349,.T.) ;
#17485 = EDGE_CURVE('',#13813,#13815,#11350,.T.) ;
#17486 = EDGE_CURVE('',#13815,#13811,#11351,.T.) ;
#17487 = EDGE_CURVE('',#13816,#13817,#11352,.T.) ;
#17488 = EDGE_CURVE('',#13817,#13818,#11353,.T.) ;
#17489 = EDGE_CURVE('',#13818,#13816,#11354,.T.) ;
#17490 = EDGE_CURVE('',#13819,#13820,#11355,.T.) ;
#17491 = EDGE_CURVE('',#13820,#13821,#11356,.T.) ;
#17492 = EDGE_CURVE('',#13821,#13819,#11357,.T.) ;
#17493 = EDGE_CURVE('',#13822,#13823,#11358,.T.) ;
#17494 = EDGE_CURVE('',#13823,#13824,#11359,.T.) ;
#17495 = EDGE_CURVE('',#13824,#13822,#11360,.T.) ;
#17496 = EDGE_CURVE('',#13825,#13826,#11361,.T.) ;
#17497 = EDGE_CURVE('',#13826,#13827,#11362,.T.) ;
#17498 = EDGE_CURVE('',#13828,#13827,#11363,.T.) ;
#17499 = EDGE_CURVE('',#13827,#13829,#11364,.T.) ;
#17500 = EDGE_CURVE('',#13829,#13825,#11365,.T.) ;
#17501 = EDGE_CURVE('',#13830,#13831,#11366,.T.) ;
#17502 = EDGE_CURVE('',#13831,#13832,#11367,.T.) ;
#17503 = EDGE_CURVE('',#13832,#13830,#11368,.T.) ;
#17504 = EDGE_CURVE('',#13833,#13834,#11369,.T.) ;
#17505 = EDGE_CURVE('',#13834,#13835,#11370,.T.) ;
#17506 = EDGE_CURVE('',#13835,#13833,#11371,.T.) ;
#17507 = EDGE_CURVE('',#13836,#13837,#11372,.T.) ;
#17508 = EDGE_CURVE('',#13837,#13838,#11373,.T.) ;
#17509 = EDGE_CURVE('',#13838,#13836,#11374,.T.) ;
#17510 = EDGE_CURVE('',#13839,#13840,#11375,.T.) ;
#17511 = EDGE_CURVE('',#13840,#13841,#11376,.T.) ;
#17512 = EDGE_CURVE('',#13841,#13842,#11377,.T.) ;
#17513 = EDGE_CURVE('',#13841,#13843,#11378,.T.) ;
#17514 = EDGE_CURVE('',#13843,#13839,#11379,.T.) ;
#17515 = EDGE_CURVE('',#13844,#13845,#11380,.T.) ;
#17516 = EDGE_CURVE('',#13845,#13846,#11381,.T.) ;
#17517 = EDGE_CURVE('',#13846,#13844,#11382,.T.) ;
#17518 = EDGE_CURVE('',#13847,#13848,#11383,.T.) ;
#17519 = EDGE_CURVE('',#13848,#13849,#11384,.T.) ;
#17520 = EDGE_CURVE('',#13849,#13847,#11385,.T.) ;
#17521 = EDGE_CURVE('',#13850,#13851,#11386,.T.) ;
#17522 = EDGE_CURVE('',#13851,#13852,#11387,.T.) ;
#17523 = EDGE_CURVE('',#13852,#13850,#11388,.T.) ;
#17524 = EDGE_CURVE('',#13853,#13854,#11389,.T.) ;
#17525 = EDGE_CURVE('',#13854,#13855,#11390,.T.) ;
#17526 = EDGE_CURVE('',#13856,#13855,#11391,.T.) ;
#17527 = EDGE_CURVE('',#13855,#13857,#11392,.T.) ;
#17528 = EDGE_CURVE('',#13857,#13853,#11393,.T.) ;
#17529 = EDGE_CURVE('',#13858,#13859,#11394,.T.) ;
#17530 = EDGE_CURVE('',#13859,#13860,#11395,.T.) ;
#17531 = EDGE_CURVE('',#13860,#13858,#11396,.T.) ;
#17532 = EDGE_CURVE('',#13861,#13862,#11397,.T.) ;
#17533 = EDGE_CURVE('',#13862,#13863,#11398,.T.) ;
#17534 = EDGE_CURVE('',#13863,#13861,#11399,.T.) ;
#17535 = EDGE_CURVE('',#13864,#13865,#11400,.T.) ;
#17536 = EDGE_CURVE('',#13865,#13866,#11401,.T.) ;
#17537 = EDGE_CURVE('',#13866,#13864,#11402,.T.) ;
#17538 = EDGE_CURVE('',#13867,#13868,#11403,.T.) ;
#17539 = EDGE_CURVE('',#13868,#13869,#11404,.T.) ;
#17540 = EDGE_CURVE('',#13869,#13870,#11405,.T.) ;
#17541 = EDGE_CURVE('',#13869,#13871,#11406,.T.) ;
#17542 = EDGE_CURVE('',#13871,#13867,#11407,.T.) ;
#17543 = EDGE_CURVE('',#13872,#13873,#11408,.T.) ;
#17544 = EDGE_CURVE('',#13873,#13874,#11409,.T.) ;
#17545 = EDGE_CURVE('',#13874,#13872,#11410,.T.) ;
#17546 = EDGE_CURVE('',#13875,#13876,#11411,.T.) ;
#17547 = EDGE_CURVE('',#13876,#13877,#11412,.T.) ;
#17548 = EDGE_CURVE('',#13877,#13875,#11413,.T.) ;
#17549 = EDGE_CURVE('',#13878,#13879,#11414,.T.) ;
#17550 = EDGE_CURVE('',#13879,#13880,#11415,.T.) ;
#17551 = EDGE_CURVE('',#13880,#13878,#11416,.T.) ;
#17552 = EDGE_CURVE('',#13881,#13882,#11417,.T.) ;
#17553 = EDGE_CURVE('',#13882,#13883,#11418,.T.) ;
#17554 = EDGE_CURVE('',#13884,#13883,#11419,.T.) ;
#17555 = EDGE_CURVE('',#13883,#13885,#11420,.T.) ;
#17556 = EDGE_CURVE('',#13885,#13881,#11421,.T.) ;
#17557 = EDGE_CURVE('',#13886,#13887,#11422,.T.) ;
#17558 = EDGE_CURVE('',#13887,#13888,#11423,.T.) ;
#17559 = EDGE_CURVE('',#13888,#13886,#11424,.T.) ;
#17560 = EDGE_CURVE('',#13889,#13890,#11425,.T.) ;
#17561 = EDGE_CURVE('',#13890,#13891,#11426,.T.) ;
#17562 = EDGE_CURVE('',#13891,#13889,#11427,.T.) ;
#17563 = EDGE_CURVE('',#13892,#13893,#11428,.T.) ;
#17564 = EDGE_CURVE('',#13893,#13894,#11429,.T.) ;
#17565 = EDGE_CURVE('',#13894,#13892,#11430,.T.) ;
#17566 = EDGE_CURVE('',#13895,#13896,#11431,.T.) ;
#17567 = EDGE_CURVE('',#13896,#13897,#11432,.T.) ;
#17568 = EDGE_CURVE('',#13897,#13898,#11433,.T.) ;
#17569 = EDGE_CURVE('',#13897,#13899,#11434,.T.) ;
#17570 = EDGE_CURVE('',#13899,#13895,#11435,.T.) ;
#17571 = EDGE_CURVE('',#13900,#13901,#11436,.T.) ;
#17572 = EDGE_CURVE('',#13901,#13902,#11437,.T.) ;
#17573 = EDGE_CURVE('',#13902,#13900,#11438,.T.) ;
#17574 = EDGE_CURVE('',#13903,#13904,#11439,.T.) ;
#17575 = EDGE_CURVE('',#13904,#13905,#11440,.T.) ;
#17576 = EDGE_CURVE('',#13905,#13903,#11441,.T.) ;
#17577 = EDGE_CURVE('',#13906,#13907,#11442,.T.) ;
#17578 = EDGE_CURVE('',#13907,#13908,#11443,.T.) ;
#17579 = EDGE_CURVE('',#13908,#13906,#11444,.T.) ;
#17580 = EDGE_CURVE('',#13909,#13910,#11445,.T.) ;
#17581 = EDGE_CURVE('',#13910,#13911,#11446,.T.) ;
#17582 = EDGE_CURVE('',#13912,#13911,#11447,.T.) ;
#17583 = EDGE_CURVE('',#13911,#13913,#11448,.T.) ;
#17584 = EDGE_CURVE('',#13913,#13909,#11449,.T.) ;
#17585 = EDGE_CURVE('',#13914,#13915,#11450,.T.) ;
#17586 = EDGE_CURVE('',#13915,#13916,#11451,.T.) ;
#17587 = EDGE_CURVE('',#13916,#13914,#11452,.T.) ;
#17588 = EDGE_CURVE('',#13917,#13918,#11453,.T.) ;
#17589 = EDGE_CURVE('',#13918,#13919,#11454,.T.) ;
#17590 = EDGE_CURVE('',#13919,#13917,#11455,.T.) ;
#17591 = EDGE_CURVE('',#13920,#13921,#11456,.T.) ;
#17592 = EDGE_CURVE('',#13921,#13922,#11457,.T.) ;
#17593 = EDGE_CURVE('',#13922,#13920,#11458,.T.) ;
#17594 = EDGE_CURVE('',#13923,#13924,#11459,.T.) ;
#17595 = EDGE_CURVE('',#13924,#13925,#11460,.T.) ;
#17596 = EDGE_CURVE('',#13925,#13926,#11461,.T.) ;
#17597 = EDGE_CURVE('',#13925,#13927,#11462,.T.) ;
#17598 = EDGE_CURVE('',#13927,#13923,#11463,.T.) ;
#17599 = EDGE_CURVE('',#13928,#13929,#11464,.T.) ;
#17600 = EDGE_CURVE('',#13929,#13930,#11465,.T.) ;
#17601 = EDGE_CURVE('',#13930,#13928,#11466,.T.) ;
#17602 = EDGE_CURVE('',#13931,#13932,#11467,.T.) ;
#17603 = EDGE_CURVE('',#13932,#13933,#11468,.T.) ;
#17604 = EDGE_CURVE('',#13933,#13931,#11469,.T.) ;
#17605 = EDGE_CURVE('',#13934,#13935,#11470,.T.) ;
#17606 = EDGE_CURVE('',#13935,#13936,#11471,.T.) ;
#17607 = EDGE_CURVE('',#13936,#13934,#11472,.T.) ;
#17608 = EDGE_CURVE('',#13937,#13938,#11473,.T.) ;
#17609 = EDGE_CURVE('',#13938,#13939,#11474,.T.) ;
#17610 = EDGE_CURVE('',#13940,#13939,#11475,.T.) ;
#17611 = EDGE_CURVE('',#13939,#13941,#11476,.T.) ;
#17612 = EDGE_CURVE('',#13941,#13937,#11477,.T.) ;
#17613 = EDGE_CURVE('',#13942,#13943,#11478,.T.) ;
#17614 = EDGE_CURVE('',#13943,#13944,#11479,.T.) ;
#17615 = EDGE_CURVE('',#13944,#13942,#11480,.T.) ;
#17616 = EDGE_CURVE('',#13945,#13946,#11481,.T.) ;
#17617 = EDGE_CURVE('',#13946,#13947,#11482,.T.) ;
#17618 = EDGE_CURVE('',#13947,#13945,#11483,.T.) ;
#17619 = EDGE_CURVE('',#13948,#13949,#11484,.T.) ;
#17620 = EDGE_CURVE('',#13949,#13950,#11485,.T.) ;
#17621 = EDGE_CURVE('',#13950,#13948,#11486,.T.) ;
#17622 = EDGE_CURVE('',#13951,#13952,#11487,.T.) ;
#17623 = EDGE_CURVE('',#13952,#13953,#11488,.T.) ;
#17624 = EDGE_CURVE('',#13953,#13954,#11489,.T.) ;
#17625 = EDGE_CURVE('',#13953,#13955,#11490,.T.) ;
#17626 = EDGE_CURVE('',#13955,#13951,#11491,.T.) ;
#17627 = EDGE_CURVE('',#13956,#13957,#11492,.T.) ;
#17628 = EDGE_CURVE('',#13957,#13958,#11493,.T.) ;
#17629 = EDGE_CURVE('',#13958,#13956,#11494,.T.) ;
#17630 = EDGE_CURVE('',#13959,#13960,#11495,.T.) ;
#17631 = EDGE_CURVE('',#13960,#13961,#11496,.T.) ;
#17632 = EDGE_CURVE('',#13961,#13959,#11497,.T.) ;
#17633 = EDGE_CURVE('',#13962,#13963,#11498,.T.) ;
#17634 = EDGE_CURVE('',#13963,#13964,#11499,.T.) ;
#17635 = EDGE_CURVE('',#13964,#13962,#11500,.T.) ;
#17636 = EDGE_CURVE('',#13965,#13966,#11501,.T.) ;
#17637 = EDGE_CURVE('',#13966,#13967,#11502,.T.) ;
#17638 = EDGE_CURVE('',#13968,#13967,#11503,.T.) ;
#17639 = EDGE_CURVE('',#13967,#13969,#11504,.T.) ;
#17640 = EDGE_CURVE('',#13969,#13965,#11505,.T.) ;
#17641 = EDGE_CURVE('',#13970,#13971,#11506,.T.) ;
#17642 = EDGE_CURVE('',#13971,#13972,#11507,.T.) ;
#17643 = EDGE_CURVE('',#13972,#13970,#11508,.T.) ;
#17644 = EDGE_CURVE('',#13973,#13974,#11509,.T.) ;
#17645 = EDGE_CURVE('',#13974,#13975,#11510,.T.) ;
#17646 = EDGE_CURVE('',#13975,#13973,#11511,.T.) ;
#17647 = EDGE_CURVE('',#13976,#13977,#11512,.T.) ;
#17648 = EDGE_CURVE('',#13977,#13978,#11513,.T.) ;
#17649 = EDGE_CURVE('',#13978,#13976,#11514,.T.) ;
#17650 = EDGE_CURVE('',#13979,#13980,#11515,.T.) ;
#17651 = EDGE_CURVE('',#13980,#13981,#11516,.T.) ;
#17652 = EDGE_CURVE('',#13981,#13982,#11517,.T.) ;
#17653 = EDGE_CURVE('',#13981,#13983,#11518,.T.) ;
#17654 = EDGE_CURVE('',#13983,#13979,#11519,.T.) ;
#17655 = EDGE_CURVE('',#13984,#13985,#11520,.T.) ;
#17656 = EDGE_CURVE('',#13985,#13986,#11521,.T.) ;
#17657 = EDGE_CURVE('',#13986,#13984,#11522,.T.) ;
#17658 = EDGE_CURVE('',#13987,#13988,#11523,.T.) ;
#17659 = EDGE_CURVE('',#13988,#13989,#11524,.T.) ;
#17660 = EDGE_CURVE('',#13989,#13987,#11525,.T.) ;
#17661 = EDGE_CURVE('',#13990,#13991,#11526,.T.) ;
#17662 = EDGE_CURVE('',#13991,#13992,#11527,.T.) ;
#17663 = EDGE_CURVE('',#13992,#13990,#11528,.T.) ;
#17664 = EDGE_CURVE('',#13993,#13994,#11529,.T.) ;
#17665 = EDGE_CURVE('',#13994,#13995,#11530,.T.) ;
#17666 = EDGE_CURVE('',#13996,#13995,#11531,.T.) ;
#17667 = EDGE_CURVE('',#13995,#13997,#11532,.T.) ;
#17668 = EDGE_CURVE('',#13997,#13993,#11533,.T.) ;
#17669 = EDGE_CURVE('',#13998,#13999,#11534,.T.) ;
#17670 = EDGE_CURVE('',#13999,#14000,#11535,.T.) ;
#17671 = EDGE_CURVE('',#14000,#13998,#11536,.T.) ;
#17672 = EDGE_CURVE('',#14001,#14002,#11537,.T.) ;
#17673 = EDGE_CURVE('',#14002,#14003,#11538,.T.) ;
#17674 = EDGE_CURVE('',#14003,#14001,#11539,.T.) ;
#17675 = EDGE_CURVE('',#14004,#14005,#11540,.T.) ;
#17676 = EDGE_CURVE('',#14005,#14006,#11541,.T.) ;
#17677 = EDGE_CURVE('',#14006,#14004,#11542,.T.) ;
#17678 = EDGE_CURVE('',#14007,#14008,#11543,.T.) ;
#17679 = EDGE_CURVE('',#14008,#14009,#11544,.T.) ;
#17680 = EDGE_CURVE('',#14009,#14010,#11545,.T.) ;
#17681 = EDGE_CURVE('',#14009,#14011,#11546,.T.) ;
#17682 = EDGE_CURVE('',#14011,#14007,#11547,.T.) ;
#17683 = EDGE_CURVE('',#14012,#14013,#11548,.T.) ;
#17684 = EDGE_CURVE('',#14013,#14014,#11549,.T.) ;
#17685 = EDGE_CURVE('',#14014,#14012,#11550,.T.) ;
#17686 = EDGE_CURVE('',#14015,#14016,#11551,.T.) ;
#17687 = EDGE_CURVE('',#14016,#14017,#11552,.T.) ;
#17688 = EDGE_CURVE('',#14017,#14015,#11553,.T.) ;
#17689 = EDGE_CURVE('',#14018,#14019,#11554,.T.) ;
#17690 = EDGE_CURVE('',#14019,#14020,#11555,.T.) ;
#17691 = EDGE_CURVE('',#14020,#14018,#11556,.T.) ;
#17692 = EDGE_CURVE('',#14021,#14022,#11557,.T.) ;
#17693 = EDGE_CURVE('',#14022,#14023,#11558,.T.) ;
#17694 = EDGE_CURVE('',#14024,#14023,#11559,.T.) ;
#17695 = EDGE_CURVE('',#14023,#14025,#11560,.T.) ;
#17696 = EDGE_CURVE('',#14025,#14021,#11561,.T.) ;
#17697 = EDGE_CURVE('',#14026,#14027,#11562,.T.) ;
#17698 = EDGE_CURVE('',#14027,#14028,#11563,.T.) ;
#17699 = EDGE_CURVE('',#14028,#14026,#11564,.T.) ;
#17700 = EDGE_CURVE('',#14029,#14030,#11565,.T.) ;
#17701 = EDGE_CURVE('',#14030,#14031,#11566,.T.) ;
#17702 = EDGE_CURVE('',#14031,#14029,#11567,.T.) ;
#17703 = EDGE_CURVE('',#14032,#14033,#11568,.T.) ;
#17704 = EDGE_CURVE('',#14033,#14034,#11569,.T.) ;
#17705 = EDGE_CURVE('',#14034,#14032,#11570,.T.) ;
#17706 = EDGE_CURVE('',#14035,#14036,#11571,.T.) ;
#17707 = EDGE_CURVE('',#14036,#14037,#11572,.T.) ;
#17708 = EDGE_CURVE('',#14037,#14038,#11573,.T.) ;
#17709 = EDGE_CURVE('',#14037,#14039,#11574,.T.) ;
#17710 = EDGE_CURVE('',#14039,#14035,#11575,.T.) ;
#17711 = EDGE_CURVE('',#14040,#14041,#11576,.T.) ;
#17712 = EDGE_CURVE('',#14041,#14042,#11577,.T.) ;
#17713 = EDGE_CURVE('',#14042,#14040,#11578,.T.) ;
#17714 = EDGE_CURVE('',#14043,#14044,#11579,.T.) ;
#17715 = EDGE_CURVE('',#14044,#14045,#11580,.T.) ;
#17716 = EDGE_CURVE('',#14045,#14043,#11581,.T.) ;
#17717 = EDGE_CURVE('',#14046,#14047,#11582,.T.) ;
#17718 = EDGE_CURVE('',#14047,#14048,#11583,.T.) ;
#17719 = EDGE_CURVE('',#14048,#14046,#11584,.T.) ;
#17720 = EDGE_CURVE('',#14049,#14050,#11585,.T.) ;
#17721 = EDGE_CURVE('',#14050,#14051,#11586,.T.) ;
#17722 = EDGE_CURVE('',#14052,#14051,#11587,.T.) ;
#17723 = EDGE_CURVE('',#14051,#14053,#11588,.T.) ;
#17724 = EDGE_CURVE('',#14053,#14049,#11589,.T.) ;
#17725 = EDGE_CURVE('',#14054,#14055,#11590,.T.) ;
#17726 = EDGE_CURVE('',#14055,#14056,#11591,.T.) ;
#17727 = EDGE_CURVE('',#14056,#14054,#11592,.T.) ;
#17728 = EDGE_CURVE('',#14057,#14058,#11593,.T.) ;
#17729 = EDGE_CURVE('',#14058,#14059,#11594,.T.) ;
#17730 = EDGE_CURVE('',#14059,#14057,#11595,.T.) ;
#17731 = EDGE_CURVE('',#14060,#14061,#11596,.T.) ;
#17732 = EDGE_CURVE('',#14061,#14062,#11597,.T.) ;
#17733 = EDGE_CURVE('',#14062,#14060,#11598,.T.) ;
#17734 = EDGE_CURVE('',#14063,#14064,#11599,.T.) ;
#17735 = EDGE_CURVE('',#14064,#14065,#11600,.T.) ;
#17736 = EDGE_CURVE('',#14065,#14066,#11601,.T.) ;
#17737 = EDGE_CURVE('',#14065,#14067,#11602,.T.) ;
#17738 = EDGE_CURVE('',#14067,#14063,#11603,.T.) ;
#17739 = EDGE_CURVE('',#14068,#14069,#11604,.T.) ;
#17740 = EDGE_CURVE('',#14069,#14070,#11605,.T.) ;
#17741 = EDGE_CURVE('',#14070,#14068,#11606,.T.) ;
#17742 = EDGE_CURVE('',#14071,#14072,#11607,.T.) ;
#17743 = EDGE_CURVE('',#14072,#14073,#11608,.T.) ;
#17744 = EDGE_CURVE('',#14073,#14071,#11609,.T.) ;
#17745 = EDGE_CURVE('',#14074,#14075,#11610,.T.) ;
#17746 = EDGE_CURVE('',#14075,#14076,#11611,.T.) ;
#17747 = EDGE_CURVE('',#14076,#14074,#11612,.T.) ;
#17748 = EDGE_CURVE('',#14077,#14078,#11613,.T.) ;
#17749 = EDGE_CURVE('',#14078,#14079,#11614,.T.) ;
#17750 = EDGE_CURVE('',#14080,#14079,#11615,.T.) ;
#17751 = EDGE_CURVE('',#14079,#14081,#11616,.T.) ;
#17752 = EDGE_CURVE('',#14081,#14077,#11617,.T.) ;
#17753 = EDGE_CURVE('',#14082,#14083,#11618,.T.) ;
#17754 = EDGE_CURVE('',#14083,#14084,#11619,.T.) ;
#17755 = EDGE_CURVE('',#14084,#14082,#11620,.T.) ;
#17756 = EDGE_CURVE('',#14085,#14086,#11621,.T.) ;
#17757 = EDGE_CURVE('',#14086,#14087,#11622,.T.) ;
#17758 = EDGE_CURVE('',#14087,#14085,#11623,.T.) ;
#17759 = EDGE_CURVE('',#14088,#14089,#11624,.T.) ;
#17760 = EDGE_CURVE('',#14089,#14090,#11625,.T.) ;
#17761 = EDGE_CURVE('',#14090,#14088,#11626,.T.) ;
#17762 = EDGE_CURVE('',#14091,#14092,#11627,.T.) ;
#17763 = EDGE_CURVE('',#14092,#14093,#11628,.T.) ;
#17764 = EDGE_CURVE('',#14093,#14094,#11629,.T.) ;
#17765 = EDGE_CURVE('',#14093,#14095,#11630,.T.) ;
#17766 = EDGE_CURVE('',#14095,#14091,#11631,.T.) ;
#17767 = EDGE_CURVE('',#14096,#14097,#11632,.T.) ;
#17768 = EDGE_CURVE('',#14097,#14098,#11633,.T.) ;
#17769 = EDGE_CURVE('',#14098,#14096,#11634,.T.) ;
#17770 = EDGE_CURVE('',#14099,#14100,#11635,.T.) ;
#17771 = EDGE_CURVE('',#14100,#14101,#11636,.T.) ;
#17772 = EDGE_CURVE('',#14101,#14099,#11637,.T.) ;
#17773 = EDGE_CURVE('',#14102,#14103,#11638,.T.) ;
#17774 = EDGE_CURVE('',#14103,#14104,#11639,.T.) ;
#17775 = EDGE_CURVE('',#14104,#14102,#11640,.T.) ;
#17776 = EDGE_CURVE('',#14105,#14106,#11641,.T.) ;
#17777 = EDGE_CURVE('',#14106,#14107,#11642,.T.) ;
#17778 = EDGE_CURVE('',#14108,#14107,#11643,.T.) ;
#17779 = EDGE_CURVE('',#14107,#14109,#11644,.T.) ;
#17780 = EDGE_CURVE('',#14109,#14105,#11645,.T.) ;
#17781 = EDGE_CURVE('',#14110,#14111,#11646,.T.) ;
#17782 = EDGE_CURVE('',#14111,#14112,#11647,.T.) ;
#17783 = EDGE_CURVE('',#14112,#14110,#11648,.T.) ;
#17784 = EDGE_CURVE('',#14113,#14114,#11649,.T.) ;
#17785 = EDGE_CURVE('',#14114,#14115,#11650,.T.) ;
#17786 = EDGE_CURVE('',#14115,#14113,#11651,.T.) ;
#17787 = EDGE_CURVE('',#14116,#14117,#11652,.T.) ;
#17788 = EDGE_CURVE('',#14117,#14118,#11653,.T.) ;
#17789 = EDGE_CURVE('',#14118,#14116,#11654,.T.) ;
#17790 = EDGE_CURVE('',#14119,#14120,#11655,.T.) ;
#17791 = EDGE_CURVE('',#14120,#14121,#11656,.T.) ;
#17792 = EDGE_CURVE('',#14121,#14122,#11657,.T.) ;
#17793 = EDGE_CURVE('',#14121,#14123,#11658,.T.) ;
#17794 = EDGE_CURVE('',#14123,#14119,#11659,.T.) ;
#17795 = EDGE_CURVE('',#14124,#14125,#11660,.T.) ;
#17796 = EDGE_CURVE('',#14125,#14126,#11661,.T.) ;
#17797 = EDGE_CURVE('',#14126,#14124,#11662,.T.) ;
#17798 = EDGE_CURVE('',#14127,#14128,#11663,.T.) ;
#17799 = EDGE_CURVE('',#14128,#14129,#11664,.T.) ;
#17800 = EDGE_CURVE('',#14129,#14127,#11665,.T.) ;
#17801 = EDGE_CURVE('',#14130,#14131,#11666,.T.) ;
#17802 = EDGE_CURVE('',#14131,#14132,#11667,.T.) ;
#17803 = EDGE_CURVE('',#14132,#14130,#11668,.T.) ;
#17804 = EDGE_CURVE('',#14133,#14134,#11669,.T.) ;
#17805 = EDGE_CURVE('',#14134,#14135,#11670,.T.) ;
#17806 = EDGE_CURVE('',#14136,#14135,#11671,.T.) ;
#17807 = EDGE_CURVE('',#14135,#14137,#11672,.T.) ;
#17808 = EDGE_CURVE('',#14137,#14133,#11673,.T.) ;
#17809 = EDGE_CURVE('',#14138,#14139,#11674,.T.) ;
#17810 = EDGE_CURVE('',#14139,#14140,#11675,.T.) ;
#17811 = EDGE_CURVE('',#14140,#14138,#11676,.T.) ;
#17812 = EDGE_CURVE('',#14141,#14142,#11677,.T.) ;
#17813 = EDGE_CURVE('',#14142,#14143,#11678,.T.) ;
#17814 = EDGE_CURVE('',#14143,#14141,#11679,.T.) ;
#17815 = EDGE_CURVE('',#14144,#14145,#11680,.T.) ;
#17816 = EDGE_CURVE('',#14145,#14146,#11681,.T.) ;
#17817 = EDGE_CURVE('',#14146,#14144,#11682,.T.) ;
#17818 = EDGE_CURVE('',#14147,#14148,#11683,.T.) ;
#17819 = EDGE_CURVE('',#14148,#14149,#11684,.T.) ;
#17820 = EDGE_CURVE('',#14149,#14150,#11685,.T.) ;
#17821 = EDGE_CURVE('',#14149,#14151,#11686,.T.) ;
#17822 = EDGE_CURVE('',#14151,#14147,#11687,.T.) ;
#17823 = EDGE_CURVE('',#14152,#14153,#11688,.T.) ;
#17824 = EDGE_CURVE('',#14153,#14154,#11689,.T.) ;
#17825 = EDGE_CURVE('',#14154,#14152,#11690,.T.) ;
#17826 = EDGE_CURVE('',#14155,#14156,#11691,.T.) ;
#17827 = EDGE_CURVE('',#14156,#14157,#11692,.T.) ;
#17828 = EDGE_CURVE('',#14157,#14155,#11693,.T.) ;
#17829 = EDGE_CURVE('',#14158,#14159,#11694,.T.) ;
#17830 = EDGE_CURVE('',#14159,#14160,#11695,.T.) ;
#17831 = EDGE_CURVE('',#14160,#14158,#11696,.T.) ;
#17832 = EDGE_CURVE('',#14161,#14162,#11697,.T.) ;
#17833 = EDGE_CURVE('',#14162,#14163,#11698,.T.) ;
#17834 = EDGE_CURVE('',#14164,#14163,#11699,.T.) ;
#17835 = EDGE_CURVE('',#14163,#14165,#11700,.T.) ;
#17836 = EDGE_CURVE('',#14165,#14161,#11701,.T.) ;
#17837 = EDGE_CURVE('',#14166,#14167,#11702,.T.) ;
#17838 = EDGE_CURVE('',#14167,#14168,#11703,.T.) ;
#17839 = EDGE_CURVE('',#14168,#14166,#11704,.T.) ;
#17840 = EDGE_CURVE('',#14169,#14170,#11705,.T.) ;
#17841 = EDGE_CURVE('',#14170,#14171,#11706,.T.) ;
#17842 = EDGE_CURVE('',#14171,#14169,#11707,.T.) ;
#17843 = EDGE_CURVE('',#14172,#14173,#11708,.T.) ;
#17844 = EDGE_CURVE('',#14173,#14174,#11709,.T.) ;
#17845 = EDGE_CURVE('',#14174,#14172,#11710,.T.) ;
#17846 = EDGE_CURVE('',#14175,#14176,#11711,.T.) ;
#17847 = EDGE_CURVE('',#14176,#14177,#11712,.T.) ;
#17848 = EDGE_CURVE('',#14177,#14178,#11713,.T.) ;
#17849 = EDGE_CURVE('',#14177,#14179,#11714,.T.) ;
#17850 = EDGE_CURVE('',#14179,#14175,#11715,.T.) ;
#17851 = EDGE_CURVE('',#14180,#14181,#11716,.T.) ;
#17852 = EDGE_CURVE('',#14181,#14182,#11717,.T.) ;
#17853 = EDGE_CURVE('',#14182,#14180,#11718,.T.) ;
#17854 = EDGE_CURVE('',#14183,#14184,#11719,.T.) ;
#17855 = EDGE_CURVE('',#14184,#14185,#11720,.T.) ;
#17856 = EDGE_CURVE('',#14185,#14183,#11721,.T.) ;
#17857 = EDGE_CURVE('',#14186,#14187,#11722,.T.) ;
#17858 = EDGE_CURVE('',#14187,#14188,#11723,.T.) ;
#17859 = EDGE_CURVE('',#14188,#14186,#11724,.T.) ;
#17860 = EDGE_CURVE('',#14189,#14190,#11725,.T.) ;
#17861 = EDGE_CURVE('',#14190,#14191,#11726,.T.) ;
#17862 = EDGE_CURVE('',#14192,#14191,#11727,.T.) ;
#17863 = EDGE_CURVE('',#14191,#14193,#11728,.T.) ;
#17864 = EDGE_CURVE('',#14193,#14189,#11729,.T.) ;
#17865 = EDGE_CURVE('',#14194,#14195,#11730,.T.) ;
#17866 = EDGE_CURVE('',#14195,#14196,#11731,.T.) ;
#17867 = EDGE_CURVE('',#14196,#14194,#11732,.T.) ;
#17868 = EDGE_CURVE('',#14197,#14198,#11733,.T.) ;
#17869 = EDGE_CURVE('',#14198,#14199,#11734,.T.) ;
#17870 = EDGE_CURVE('',#14199,#14197,#11735,.T.) ;
#17871 = EDGE_CURVE('',#14200,#14201,#11736,.T.) ;
#17872 = EDGE_CURVE('',#14201,#14202,#11737,.T.) ;
#17873 = EDGE_CURVE('',#14202,#14200,#11738,.T.) ;
#17874 = EDGE_CURVE('',#14203,#14204,#11739,.T.) ;
#17875 = EDGE_CURVE('',#14204,#14205,#11740,.T.) ;
#17876 = EDGE_CURVE('',#14205,#14206,#11741,.T.) ;
#17877 = EDGE_CURVE('',#14205,#14207,#11742,.T.) ;
#17878 = EDGE_CURVE('',#14207,#14203,#11743,.T.) ;
#17879 = EDGE_CURVE('',#14208,#14209,#11744,.T.) ;
#17880 = EDGE_CURVE('',#14209,#14210,#11745,.T.) ;
#17881 = EDGE_CURVE('',#14210,#14208,#11746,.T.) ;
#17882 = EDGE_CURVE('',#14211,#14212,#11747,.T.) ;
#17883 = EDGE_CURVE('',#14212,#14213,#11748,.T.) ;
#17884 = EDGE_CURVE('',#14213,#14211,#11749,.T.) ;
#17885 = EDGE_CURVE('',#14214,#14215,#11750,.T.) ;
#17886 = EDGE_CURVE('',#14215,#14216,#11751,.T.) ;
#17887 = EDGE_CURVE('',#14216,#14214,#11752,.T.) ;
#17888 = EDGE_CURVE('',#13766,#13777,#421,.T.) ;
#17889 = EDGE_CURVE('',#13767,#13779,#422,.T.) ;
#17890 = EDGE_CURVE('',#13778,#14217,#7909,.T.) ;
#17891 = EDGE_CURVE('',#13781,#14217,#423,.T.) ;
#17892 = EDGE_CURVE('',#14217,#13780,#424,.T.) ;
#17893 = EDGE_CURVE('',#13782,#14218,#7910,.T.) ;
#17894 = EDGE_CURVE('',#13784,#14218,#425,.T.) ;
#17895 = EDGE_CURVE('',#14218,#13783,#426,.T.) ;
#17896 = EDGE_CURVE('',#13787,#14219,#7911,.T.) ;
#17897 = EDGE_CURVE('',#13789,#14219,#427,.T.) ;
#17898 = EDGE_CURVE('',#14219,#13788,#428,.T.) ;
#17899 = EDGE_CURVE('',#13790,#14220,#7912,.T.) ;
#17900 = EDGE_CURVE('',#13792,#14220,#429,.T.) ;
#17901 = EDGE_CURVE('',#14220,#13791,#430,.T.) ;
#17902 = EDGE_CURVE('',#13793,#14221,#7913,.T.) ;
#17903 = EDGE_CURVE('',#13795,#14221,#431,.T.) ;
#17904 = EDGE_CURVE('',#14221,#13794,#432,.T.) ;
#17905 = EDGE_CURVE('',#13796,#14222,#7914,.T.) ;
#17906 = EDGE_CURVE('',#13798,#14222,#433,.T.) ;
#17907 = EDGE_CURVE('',#14222,#13797,#434,.T.) ;
#17908 = EDGE_CURVE('',#13801,#14223,#7915,.T.) ;
#17909 = EDGE_CURVE('',#13803,#14223,#435,.T.) ;
#17910 = EDGE_CURVE('',#14223,#13802,#436,.T.) ;
#17911 = EDGE_CURVE('',#13804,#14224,#7916,.T.) ;
#17912 = EDGE_CURVE('',#13806,#14224,#437,.T.) ;
#17913 = EDGE_CURVE('',#14224,#13805,#438,.T.) ;
#17914 = EDGE_CURVE('',#13807,#14225,#7917,.T.) ;
#17915 = EDGE_CURVE('',#13809,#14225,#439,.T.) ;
#17916 = EDGE_CURVE('',#14225,#13808,#440,.T.) ;
#17917 = EDGE_CURVE('',#13810,#14226,#7918,.T.) ;
#17918 = EDGE_CURVE('',#13812,#14226,#441,.T.) ;
#17919 = EDGE_CURVE('',#14226,#13811,#442,.T.) ;
#17920 = EDGE_CURVE('',#13815,#14227,#7919,.T.) ;
#17921 = EDGE_CURVE('',#13817,#14227,#443,.T.) ;
#17922 = EDGE_CURVE('',#14227,#13816,#444,.T.) ;
#17923 = EDGE_CURVE('',#13818,#14228,#7920,.T.) ;
#17924 = EDGE_CURVE('',#13820,#14228,#445,.T.) ;
#17925 = EDGE_CURVE('',#14228,#13819,#446,.T.) ;
#17926 = EDGE_CURVE('',#13821,#14229,#7921,.T.) ;
#17927 = EDGE_CURVE('',#13823,#14229,#447,.T.) ;
#17928 = EDGE_CURVE('',#14229,#13822,#448,.T.) ;
#17929 = EDGE_CURVE('',#13824,#14230,#7922,.T.) ;
#17930 = EDGE_CURVE('',#13826,#14230,#449,.T.) ;
#17931 = EDGE_CURVE('',#14230,#13825,#450,.T.) ;
#17932 = EDGE_CURVE('',#13829,#14231,#7923,.T.) ;
#17933 = EDGE_CURVE('',#13831,#14231,#451,.T.) ;
#17934 = EDGE_CURVE('',#14231,#13830,#452,.T.) ;
#17935 = EDGE_CURVE('',#13832,#14232,#7924,.T.) ;
#17936 = EDGE_CURVE('',#13834,#14232,#453,.T.) ;
#17937 = EDGE_CURVE('',#14232,#13833,#454,.T.) ;
#17938 = EDGE_CURVE('',#13835,#14233,#7925,.T.) ;
#17939 = EDGE_CURVE('',#13837,#14233,#455,.T.) ;
#17940 = EDGE_CURVE('',#14233,#13836,#456,.T.) ;
#17941 = EDGE_CURVE('',#13838,#14234,#7926,.T.) ;
#17942 = EDGE_CURVE('',#13840,#14234,#457,.T.) ;
#17943 = EDGE_CURVE('',#14234,#13839,#458,.T.) ;
#17944 = EDGE_CURVE('',#13843,#14235,#7927,.T.) ;
#17945 = EDGE_CURVE('',#13845,#14235,#459,.T.) ;
#17946 = EDGE_CURVE('',#14235,#13844,#460,.T.) ;
#17947 = EDGE_CURVE('',#13846,#14236,#7928,.T.) ;
#17948 = EDGE_CURVE('',#13848,#14236,#461,.T.) ;
#17949 = EDGE_CURVE('',#14236,#13847,#462,.T.) ;
#17950 = EDGE_CURVE('',#13849,#14237,#7929,.T.) ;
#17951 = EDGE_CURVE('',#13851,#14237,#463,.T.) ;
#17952 = EDGE_CURVE('',#14237,#13850,#464,.T.) ;
#17953 = EDGE_CURVE('',#13852,#14238,#7930,.T.) ;
#17954 = EDGE_CURVE('',#13854,#14238,#465,.T.) ;
#17955 = EDGE_CURVE('',#14238,#13853,#466,.T.) ;
#17956 = EDGE_CURVE('',#13857,#14239,#7931,.T.) ;
#17957 = EDGE_CURVE('',#13859,#14239,#467,.T.) ;
#17958 = EDGE_CURVE('',#14239,#13858,#468,.T.) ;
#17959 = EDGE_CURVE('',#13860,#14240,#7932,.T.) ;
#17960 = EDGE_CURVE('',#13862,#14240,#469,.T.) ;
#17961 = EDGE_CURVE('',#14240,#13861,#470,.T.) ;
#17962 = EDGE_CURVE('',#13863,#14241,#7933,.T.) ;
#17963 = EDGE_CURVE('',#13865,#14241,#471,.T.) ;
#17964 = EDGE_CURVE('',#14241,#13864,#472,.T.) ;
#17965 = EDGE_CURVE('',#13866,#14242,#7934,.T.) ;
#17966 = EDGE_CURVE('',#13868,#14242,#473,.T.) ;
#17967 = EDGE_CURVE('',#14242,#13867,#474,.T.) ;
#17968 = EDGE_CURVE('',#13871,#14243,#7935,.T.) ;
#17969 = EDGE_CURVE('',#13873,#14243,#475,.T.) ;
#17970 = EDGE_CURVE('',#14243,#13872,#476,.T.) ;
#17971 = EDGE_CURVE('',#13874,#14244,#7936,.T.) ;
#17972 = EDGE_CURVE('',#13876,#14244,#477,.T.) ;
#17973 = EDGE_CURVE('',#14244,#13875,#478,.T.) ;
#17974 = EDGE_CURVE('',#13877,#14245,#7937,.T.) ;
#17975 = EDGE_CURVE('',#13879,#14245,#479,.T.) ;
#17976 = EDGE_CURVE('',#14245,#13878,#480,.T.) ;
#17977 = EDGE_CURVE('',#13880,#14246,#7938,.T.) ;
#17978 = EDGE_CURVE('',#13882,#14246,#481,.T.) ;
#17979 = EDGE_CURVE('',#14246,#13881,#482,.T.) ;
#17980 = EDGE_CURVE('',#13885,#14247,#7939,.T.) ;
#17981 = EDGE_CURVE('',#13887,#14247,#483,.T.) ;
#17982 = EDGE_CURVE('',#14247,#13886,#484,.T.) ;
#17983 = EDGE_CURVE('',#13888,#14248,#7940,.T.) ;
#17984 = EDGE_CURVE('',#13890,#14248,#485,.T.) ;
#17985 = EDGE_CURVE('',#14248,#13889,#486,.T.) ;
#17986 = EDGE_CURVE('',#13891,#14249,#7941,.T.) ;
#17987 = EDGE_CURVE('',#13893,#14249,#487,.T.) ;
#17988 = EDGE_CURVE('',#14249,#13892,#488,.T.) ;
#17989 = EDGE_CURVE('',#13894,#14250,#7942,.T.) ;
#17990 = EDGE_CURVE('',#13896,#14250,#489,.T.) ;
#17991 = EDGE_CURVE('',#14250,#13895,#490,.T.) ;
#17992 = EDGE_CURVE('',#13899,#14251,#7943,.T.) ;
#17993 = EDGE_CURVE('',#13901,#14251,#491,.T.) ;
#17994 = EDGE_CURVE('',#14251,#13900,#492,.T.) ;
#17995 = EDGE_CURVE('',#13902,#14252,#7944,.T.) ;
#17996 = EDGE_CURVE('',#13904,#14252,#493,.T.) ;
#17997 = EDGE_CURVE('',#14252,#13903,#494,.T.) ;
#17998 = EDGE_CURVE('',#13905,#14253,#7945,.T.) ;
#17999 = EDGE_CURVE('',#13907,#14253,#495,.T.) ;
#18000 = EDGE_CURVE('',#14253,#13906,#496,.T.) ;
#18001 = EDGE_CURVE('',#13908,#14254,#7946,.T.) ;
#18002 = EDGE_CURVE('',#13910,#14254,#497,.T.) ;
#18003 = EDGE_CURVE('',#14254,#13909,#498,.T.) ;
#18004 = EDGE_CURVE('',#13913,#14255,#7947,.T.) ;
#18005 = EDGE_CURVE('',#13915,#14255,#499,.T.) ;
#18006 = EDGE_CURVE('',#14255,#13914,#500,.T.) ;
#18007 = EDGE_CURVE('',#13916,#14256,#7948,.T.) ;
#18008 = EDGE_CURVE('',#13918,#14256,#501,.T.) ;
#18009 = EDGE_CURVE('',#14256,#13917,#502,.T.) ;
#18010 = EDGE_CURVE('',#13919,#14257,#7949,.T.) ;
#18011 = EDGE_CURVE('',#13921,#14257,#503,.T.) ;
#18012 = EDGE_CURVE('',#14257,#13920,#504,.T.) ;
#18013 = EDGE_CURVE('',#13922,#14258,#7950,.T.) ;
#18014 = EDGE_CURVE('',#13924,#14258,#505,.T.) ;
#18015 = EDGE_CURVE('',#14258,#13923,#506,.T.) ;
#18016 = EDGE_CURVE('',#13927,#14259,#7951,.T.) ;
#18017 = EDGE_CURVE('',#13929,#14259,#507,.T.) ;
#18018 = EDGE_CURVE('',#14259,#13928,#508,.T.) ;
#18019 = EDGE_CURVE('',#13930,#14260,#7952,.T.) ;
#18020 = EDGE_CURVE('',#13932,#14260,#509,.T.) ;
#18021 = EDGE_CURVE('',#14260,#13931,#510,.T.) ;
#18022 = EDGE_CURVE('',#13933,#14261,#7953,.T.) ;
#18023 = EDGE_CURVE('',#13935,#14261,#511,.T.) ;
#18024 = EDGE_CURVE('',#14261,#13934,#512,.T.) ;
#18025 = EDGE_CURVE('',#13936,#14262,#7954,.T.) ;
#18026 = EDGE_CURVE('',#13938,#14262,#513,.T.) ;
#18027 = EDGE_CURVE('',#14262,#13937,#514,.T.) ;
#18028 = EDGE_CURVE('',#13941,#14263,#7955,.T.) ;
#18029 = EDGE_CURVE('',#13943,#14263,#515,.T.) ;
#18030 = EDGE_CURVE('',#14263,#13942,#516,.T.) ;
#18031 = EDGE_CURVE('',#13944,#14264,#7956,.T.) ;
#18032 = EDGE_CURVE('',#13946,#14264,#517,.T.) ;
#18033 = EDGE_CURVE('',#14264,#13945,#518,.T.) ;
#18034 = EDGE_CURVE('',#13947,#14265,#7957,.T.) ;
#18035 = EDGE_CURVE('',#13949,#14265,#519,.T.) ;
#18036 = EDGE_CURVE('',#14265,#13948,#520,.T.) ;
#18037 = EDGE_CURVE('',#13950,#14266,#7958,.T.) ;
#18038 = EDGE_CURVE('',#13952,#14266,#521,.T.) ;
#18039 = EDGE_CURVE('',#14266,#13951,#522,.T.) ;
#18040 = EDGE_CURVE('',#13955,#14267,#7959,.T.) ;
#18041 = EDGE_CURVE('',#13957,#14267,#523,.T.) ;
#18042 = EDGE_CURVE('',#14267,#13956,#524,.T.) ;
#18043 = EDGE_CURVE('',#13958,#14268,#7960,.T.) ;
#18044 = EDGE_CURVE('',#13960,#14268,#525,.T.) ;
#18045 = EDGE_CURVE('',#14268,#13959,#526,.T.) ;
#18046 = EDGE_CURVE('',#13961,#14269,#7961,.T.) ;
#18047 = EDGE_CURVE('',#13963,#14269,#527,.T.) ;
#18048 = EDGE_CURVE('',#14269,#13962,#528,.T.) ;
#18049 = EDGE_CURVE('',#13964,#14270,#7962,.T.) ;
#18050 = EDGE_CURVE('',#13966,#14270,#529,.T.) ;
#18051 = EDGE_CURVE('',#14270,#13965,#530,.T.) ;
#18052 = EDGE_CURVE('',#13969,#14271,#7963,.T.) ;
#18053 = EDGE_CURVE('',#13971,#14271,#531,.T.) ;
#18054 = EDGE_CURVE('',#14271,#13970,#532,.T.) ;
#18055 = EDGE_CURVE('',#13972,#14272,#7964,.T.) ;
#18056 = EDGE_CURVE('',#13974,#14272,#533,.T.) ;
#18057 = EDGE_CURVE('',#14272,#13973,#534,.T.) ;
#18058 = EDGE_CURVE('',#13975,#14273,#7965,.T.) ;
#18059 = EDGE_CURVE('',#13977,#14273,#535,.T.) ;
#18060 = EDGE_CURVE('',#14273,#13976,#536,.T.) ;
#18061 = EDGE_CURVE('',#13978,#14274,#7966,.T.) ;
#18062 = EDGE_CURVE('',#13980,#14274,#537,.T.) ;
#18063 = EDGE_CURVE('',#14274,#13979,#538,.T.) ;
#18064 = EDGE_CURVE('',#13983,#14275,#7967,.T.) ;
#18065 = EDGE_CURVE('',#13985,#14275,#539,.T.) ;
#18066 = EDGE_CURVE('',#14275,#13984,#540,.T.) ;
#18067 = EDGE_CURVE('',#13986,#14276,#7968,.T.) ;
#18068 = EDGE_CURVE('',#13988,#14276,#541,.T.) ;
#18069 = EDGE_CURVE('',#14276,#13987,#542,.T.) ;
#18070 = EDGE_CURVE('',#13989,#14277,#7969,.T.) ;
#18071 = EDGE_CURVE('',#13991,#14277,#543,.T.) ;
#18072 = EDGE_CURVE('',#14277,#13990,#544,.T.) ;
#18073 = EDGE_CURVE('',#13992,#14278,#7970,.T.) ;
#18074 = EDGE_CURVE('',#13994,#14278,#545,.T.) ;
#18075 = EDGE_CURVE('',#14278,#13993,#546,.T.) ;
#18076 = EDGE_CURVE('',#13997,#14279,#7971,.T.) ;
#18077 = EDGE_CURVE('',#13999,#14279,#547,.T.) ;
#18078 = EDGE_CURVE('',#14279,#13998,#548,.T.) ;
#18079 = EDGE_CURVE('',#14000,#14280,#7972,.T.) ;
#18080 = EDGE_CURVE('',#14002,#14280,#549,.T.) ;
#18081 = EDGE_CURVE('',#14280,#14001,#550,.T.) ;
#18082 = EDGE_CURVE('',#14003,#14281,#7973,.T.) ;
#18083 = EDGE_CURVE('',#14005,#14281,#551,.T.) ;
#18084 = EDGE_CURVE('',#14281,#14004,#552,.T.) ;
#18085 = EDGE_CURVE('',#14006,#14282,#7974,.T.) ;
#18086 = EDGE_CURVE('',#14008,#14282,#553,.T.) ;
#18087 = EDGE_CURVE('',#14282,#14007,#554,.T.) ;
#18088 = EDGE_CURVE('',#14011,#14283,#7975,.T.) ;
#18089 = EDGE_CURVE('',#14013,#14283,#555,.T.) ;
#18090 = EDGE_CURVE('',#14283,#14012,#556,.T.) ;
#18091 = EDGE_CURVE('',#14014,#14284,#7976,.T.) ;
#18092 = EDGE_CURVE('',#14016,#14284,#557,.T.) ;
#18093 = EDGE_CURVE('',#14284,#14015,#558,.T.) ;
#18094 = EDGE_CURVE('',#14017,#14285,#7977,.T.) ;
#18095 = EDGE_CURVE('',#14019,#14285,#559,.T.) ;
#18096 = EDGE_CURVE('',#14285,#14018,#560,.T.) ;
#18097 = EDGE_CURVE('',#14020,#14286,#7978,.T.) ;
#18098 = EDGE_CURVE('',#14022,#14286,#561,.T.) ;
#18099 = EDGE_CURVE('',#14286,#14021,#562,.T.) ;
#18100 = EDGE_CURVE('',#14025,#14287,#7979,.T.) ;
#18101 = EDGE_CURVE('',#14027,#14287,#563,.T.) ;
#18102 = EDGE_CURVE('',#14287,#14026,#564,.T.) ;
#18103 = EDGE_CURVE('',#14028,#14288,#7980,.T.) ;
#18104 = EDGE_CURVE('',#14030,#14288,#565,.T.) ;
#18105 = EDGE_CURVE('',#14288,#14029,#566,.T.) ;
#18106 = EDGE_CURVE('',#14031,#14289,#7981,.T.) ;
#18107 = EDGE_CURVE('',#14033,#14289,#567,.T.) ;
#18108 = EDGE_CURVE('',#14289,#14032,#568,.T.) ;
#18109 = EDGE_CURVE('',#14034,#14290,#7982,.T.) ;
#18110 = EDGE_CURVE('',#14036,#14290,#569,.T.) ;
#18111 = EDGE_CURVE('',#14290,#14035,#570,.T.) ;
#18112 = EDGE_CURVE('',#14039,#14291,#7983,.T.) ;
#18113 = EDGE_CURVE('',#14041,#14291,#571,.T.) ;
#18114 = EDGE_CURVE('',#14291,#14040,#572,.T.) ;
#18115 = EDGE_CURVE('',#14042,#14292,#7984,.T.) ;
#18116 = EDGE_CURVE('',#14044,#14292,#573,.T.) ;
#18117 = EDGE_CURVE('',#14292,#14043,#574,.T.) ;
#18118 = EDGE_CURVE('',#14045,#14293,#7985,.T.) ;
#18119 = EDGE_CURVE('',#14047,#14293,#575,.T.) ;
#18120 = EDGE_CURVE('',#14293,#14046,#576,.T.) ;
#18121 = EDGE_CURVE('',#14048,#14294,#7986,.T.) ;
#18122 = EDGE_CURVE('',#14050,#14294,#577,.T.) ;
#18123 = EDGE_CURVE('',#14294,#14049,#578,.T.) ;
#18124 = EDGE_CURVE('',#14053,#14295,#7987,.T.) ;
#18125 = EDGE_CURVE('',#14055,#14295,#579,.T.) ;
#18126 = EDGE_CURVE('',#14295,#14054,#580,.T.) ;
#18127 = EDGE_CURVE('',#14056,#14296,#7988,.T.) ;
#18128 = EDGE_CURVE('',#14058,#14296,#581,.T.) ;
#18129 = EDGE_CURVE('',#14296,#14057,#582,.T.) ;
#18130 = EDGE_CURVE('',#14059,#14297,#7989,.T.) ;
#18131 = EDGE_CURVE('',#14061,#14297,#583,.T.) ;
#18132 = EDGE_CURVE('',#14297,#14060,#584,.T.) ;
#18133 = EDGE_CURVE('',#14062,#14298,#7990,.T.) ;
#18134 = EDGE_CURVE('',#14064,#14298,#585,.T.) ;
#18135 = EDGE_CURVE('',#14298,#14063,#586,.T.) ;
#18136 = EDGE_CURVE('',#14067,#14299,#7991,.T.) ;
#18137 = EDGE_CURVE('',#14069,#14299,#587,.T.) ;
#18138 = EDGE_CURVE('',#14299,#14068,#588,.T.) ;
#18139 = EDGE_CURVE('',#14070,#14300,#7992,.T.) ;
#18140 = EDGE_CURVE('',#14072,#14300,#589,.T.) ;
#18141 = EDGE_CURVE('',#14300,#14071,#590,.T.) ;
#18142 = EDGE_CURVE('',#14073,#14301,#7993,.T.) ;
#18143 = EDGE_CURVE('',#14075,#14301,#591,.T.) ;
#18144 = EDGE_CURVE('',#14301,#14074,#592,.T.) ;
#18145 = EDGE_CURVE('',#14076,#14302,#7994,.T.) ;
#18146 = EDGE_CURVE('',#14078,#14302,#593,.T.) ;
#18147 = EDGE_CURVE('',#14302,#14077,#594,.T.) ;
#18148 = EDGE_CURVE('',#14081,#14303,#7995,.T.) ;
#18149 = EDGE_CURVE('',#14083,#14303,#595,.T.) ;
#18150 = EDGE_CURVE('',#14303,#14082,#596,.T.) ;
#18151 = EDGE_CURVE('',#14084,#14304,#7996,.T.) ;
#18152 = EDGE_CURVE('',#14086,#14304,#597,.T.) ;
#18153 = EDGE_CURVE('',#14304,#14085,#598,.T.) ;
#18154 = EDGE_CURVE('',#14087,#14305,#7997,.T.) ;
#18155 = EDGE_CURVE('',#14089,#14305,#599,.T.) ;
#18156 = EDGE_CURVE('',#14305,#14088,#600,.T.) ;
#18157 = EDGE_CURVE('',#14090,#14306,#7998,.T.) ;
#18158 = EDGE_CURVE('',#14092,#14306,#601,.T.) ;
#18159 = EDGE_CURVE('',#14306,#14091,#602,.T.) ;
#18160 = EDGE_CURVE('',#14095,#14307,#7999,.T.) ;
#18161 = EDGE_CURVE('',#14097,#14307,#603,.T.) ;
#18162 = EDGE_CURVE('',#14307,#14096,#604,.T.) ;
#18163 = EDGE_CURVE('',#14098,#14308,#8000,.T.) ;
#18164 = EDGE_CURVE('',#14100,#14308,#605,.T.) ;
#18165 = EDGE_CURVE('',#14308,#14099,#606,.T.) ;
#18166 = EDGE_CURVE('',#14101,#14309,#8001,.T.) ;
#18167 = EDGE_CURVE('',#14103,#14309,#607,.T.) ;
#18168 = EDGE_CURVE('',#14309,#14102,#608,.T.) ;
#18169 = EDGE_CURVE('',#14104,#14310,#8002,.T.) ;
#18170 = EDGE_CURVE('',#14106,#14310,#609,.T.) ;
#18171 = EDGE_CURVE('',#14310,#14105,#610,.T.) ;
#18172 = EDGE_CURVE('',#14109,#14311,#8003,.T.) ;
#18173 = EDGE_CURVE('',#14111,#14311,#611,.T.) ;
#18174 = EDGE_CURVE('',#14311,#14110,#612,.T.) ;
#18175 = EDGE_CURVE('',#14112,#14312,#8004,.T.) ;
#18176 = EDGE_CURVE('',#14114,#14312,#613,.T.) ;
#18177 = EDGE_CURVE('',#14312,#14113,#614,.T.) ;
#18178 = EDGE_CURVE('',#14115,#14313,#8005,.T.) ;
#18179 = EDGE_CURVE('',#14117,#14313,#615,.T.) ;
#18180 = EDGE_CURVE('',#14313,#14116,#616,.T.) ;
#18181 = EDGE_CURVE('',#14118,#14314,#8006,.T.) ;
#18182 = EDGE_CURVE('',#14120,#14314,#617,.T.) ;
#18183 = EDGE_CURVE('',#14314,#14119,#618,.T.) ;
#18184 = EDGE_CURVE('',#14123,#14315,#8007,.T.) ;
#18185 = EDGE_CURVE('',#14125,#14315,#619,.T.) ;
#18186 = EDGE_CURVE('',#14315,#14124,#620,.T.) ;
#18187 = EDGE_CURVE('',#14126,#14316,#8008,.T.) ;
#18188 = EDGE_CURVE('',#14128,#14316,#621,.T.) ;
#18189 = EDGE_CURVE('',#14316,#14127,#622,.T.) ;
#18190 = EDGE_CURVE('',#14129,#14317,#8009,.T.) ;
#18191 = EDGE_CURVE('',#14131,#14317,#623,.T.) ;
#18192 = EDGE_CURVE('',#14317,#14130,#624,.T.) ;
#18193 = EDGE_CURVE('',#14132,#14318,#8010,.T.) ;
#18194 = EDGE_CURVE('',#14134,#14318,#625,.T.) ;
#18195 = EDGE_CURVE('',#14318,#14133,#626,.T.) ;
#18196 = EDGE_CURVE('',#14137,#14319,#8011,.T.) ;
#18197 = EDGE_CURVE('',#14139,#14319,#627,.T.) ;
#18198 = EDGE_CURVE('',#14319,#14138,#628,.T.) ;
#18199 = EDGE_CURVE('',#14140,#14320,#8012,.T.) ;
#18200 = EDGE_CURVE('',#14142,#14320,#629,.T.) ;
#18201 = EDGE_CURVE('',#14320,#14141,#630,.T.) ;
#18202 = EDGE_CURVE('',#14143,#14321,#8013,.T.) ;
#18203 = EDGE_CURVE('',#14145,#14321,#631,.T.) ;
#18204 = EDGE_CURVE('',#14321,#14144,#632,.T.) ;
#18205 = EDGE_CURVE('',#14146,#14322,#8014,.T.) ;
#18206 = EDGE_CURVE('',#14148,#14322,#633,.T.) ;
#18207 = EDGE_CURVE('',#14322,#14147,#634,.T.) ;
#18208 = EDGE_CURVE('',#14151,#14323,#8015,.T.) ;
#18209 = EDGE_CURVE('',#14153,#14323,#635,.T.) ;
#18210 = EDGE_CURVE('',#14323,#14152,#636,.T.) ;
#18211 = EDGE_CURVE('',#14154,#14324,#8016,.T.) ;
#18212 = EDGE_CURVE('',#14156,#14324,#637,.T.) ;
#18213 = EDGE_CURVE('',#14324,#14155,#638,.T.) ;
#18214 = EDGE_CURVE('',#14157,#14325,#8017,.T.) ;
#18215 = EDGE_CURVE('',#14159,#14325,#639,.T.) ;
#18216 = EDGE_CURVE('',#14325,#14158,#640,.T.) ;
#18217 = EDGE_CURVE('',#14160,#14326,#8018,.T.) ;
#18218 = EDGE_CURVE('',#14162,#14326,#641,.T.) ;
#18219 = EDGE_CURVE('',#14326,#14161,#642,.T.) ;
#18220 = EDGE_CURVE('',#14165,#14327,#8019,.T.) ;
#18221 = EDGE_CURVE('',#14167,#14327,#643,.T.) ;
#18222 = EDGE_CURVE('',#14327,#14166,#644,.T.) ;
#18223 = EDGE_CURVE('',#14168,#14328,#8020,.T.) ;
#18224 = EDGE_CURVE('',#14170,#14328,#645,.T.) ;
#18225 = EDGE_CURVE('',#14328,#14169,#646,.T.) ;
#18226 = EDGE_CURVE('',#14171,#14329,#8021,.T.) ;
#18227 = EDGE_CURVE('',#14173,#14329,#647,.T.) ;
#18228 = EDGE_CURVE('',#14329,#14172,#648,.T.) ;
#18229 = EDGE_CURVE('',#14174,#14330,#8022,.T.) ;
#18230 = EDGE_CURVE('',#14176,#14330,#649,.T.) ;
#18231 = EDGE_CURVE('',#14330,#14175,#650,.T.) ;
#18232 = EDGE_CURVE('',#14179,#14331,#8023,.T.) ;
#18233 = EDGE_CURVE('',#14181,#14331,#651,.T.) ;
#18234 = EDGE_CURVE('',#14331,#14180,#652,.T.) ;
#18235 = EDGE_CURVE('',#14182,#14332,#8024,.T.) ;
#18236 = EDGE_CURVE('',#14184,#14332,#653,.T.) ;
#18237 = EDGE_CURVE('',#14332,#14183,#654,.T.) ;
#18238 = EDGE_CURVE('',#14185,#14333,#8025,.T.) ;
#18239 = EDGE_CURVE('',#14187,#14333,#655,.T.) ;
#18240 = EDGE_CURVE('',#14333,#14186,#656,.T.) ;
#18241 = EDGE_CURVE('',#14188,#14334,#8026,.T.) ;
#18242 = EDGE_CURVE('',#14190,#14334,#657,.T.) ;
#18243 = EDGE_CURVE('',#14334,#14189,#658,.T.) ;
#18244 = EDGE_CURVE('',#14193,#14335,#8027,.T.) ;
#18245 = EDGE_CURVE('',#14195,#14335,#659,.T.) ;
#18246 = EDGE_CURVE('',#14335,#14194,#660,.T.) ;
#18247 = EDGE_CURVE('',#14196,#14336,#8028,.T.) ;
#18248 = EDGE_CURVE('',#14198,#14336,#661,.T.) ;
#18249 = EDGE_CURVE('',#14336,#14197,#662,.T.) ;
#18250 = EDGE_CURVE('',#14199,#14337,#8029,.T.) ;
#18251 = EDGE_CURVE('',#14201,#14337,#663,.T.) ;
#18252 = EDGE_CURVE('',#14337,#14200,#664,.T.) ;
#18253 = EDGE_CURVE('',#14202,#14338,#8030,.T.) ;
#18254 = EDGE_CURVE('',#14204,#14338,#665,.T.) ;
#18255 = EDGE_CURVE('',#14338,#14203,#666,.T.) ;
#18256 = EDGE_CURVE('',#14207,#14339,#8031,.T.) ;
#18257 = EDGE_CURVE('',#14209,#14339,#667,.T.) ;
#18258 = EDGE_CURVE('',#14339,#14208,#668,.T.) ;
#18259 = EDGE_CURVE('',#14210,#14340,#8032,.T.) ;
#18260 = EDGE_CURVE('',#14212,#14340,#669,.T.) ;
#18261 = EDGE_CURVE('',#14340,#14211,#670,.T.) ;
#18262 = EDGE_CURVE('',#14213,#14341,#8033,.T.) ;
#18263 = EDGE_CURVE('',#14215,#14341,#671,.T.) ;
#18264 = EDGE_CURVE('',#14341,#14214,#672,.T.) ;
#18265 = EDGE_CURVE('',#14216,#14342,#8034,.T.) ;
#18266 = EDGE_CURVE('',#14342,#14342,#11753,.T.) ;
#18267 = EDGE_CURVE('',#14343,#14343,#11754,.T.) ;
#18268 = EDGE_CURVE('',#14343,#14344,#8035,.T.) ;
#18269 = EDGE_CURVE('',#14345,#14344,#33,.T.) ;
#18270 = EDGE_CURVE('',#14345,#14346,#8036,.T.) ;
#18271 = EDGE_CURVE('',#14346,#14346,#11755,.T.) ;
#18272 = EDGE_CURVE('',#14347,#14345,#34,.T.) ;
#18273 = EDGE_CURVE('',#14344,#14347,#35,.T.) ;
#18274 = EDGE_CURVE('',#14348,#14348,#11756,.T.) ;
#18275 = EDGE_CURVE('',#14348,#14349,#8037,.T.) ;
#18276 = EDGE_CURVE('',#14349,#14349,#11757,.T.) ;
#18277 = EDGE_CURVE('',#14345,#14350,#8038,.T.) ;
#18278 = EDGE_CURVE('',#14350,#14350,#11758,.T.) ;
#18279 = EDGE_CURVE('',#14351,#14352,#11759,.T.) ;
#18280 = EDGE_CURVE('',#14353,#14354,#11760,.T.) ;
#18281 = EDGE_CURVE('',#14354,#14353,#11761,.T.) ;
#18282 = EDGE_CURVE('',#14353,#14354,#673,.T.) ;
#18283 = EDGE_CURVE('',#14355,#14355,#11762,.T.) ;
#18284 = EDGE_CURVE('',#14356,#14356,#11763,.T.) ;
#18285 = EDGE_CURVE('',#14357,#14358,#36,.T.) ;
#18286 = EDGE_CURVE('',#14357,#14358,#11764,.T.) ;
#18287 = EDGE_CURVE('',#14359,#14360,#674,.T.) ;
#18288 = EDGE_CURVE('',#14361,#14360,#11765,.T.) ;
#18289 = EDGE_CURVE('',#14361,#14355,#8039,.T.) ;
#18290 = EDGE_CURVE('',#14359,#14361,#11766,.T.) ;
#18291 = EDGE_CURVE('',#14362,#14362,#11767,.T.) ;
#18292 = EDGE_CURVE('',#14363,#14363,#11768,.T.) ;
#18293 = EDGE_CURVE('',#14364,#14365,#37,.T.) ;
#18294 = EDGE_CURVE('',#14365,#14364,#11769,.T.) ;
#18295 = EDGE_CURVE('',#14362,#14366,#8040,.T.) ;
#18296 = EDGE_CURVE('',#14360,#14366,#11770,.T.) ;
#18297 = EDGE_CURVE('',#14366,#14359,#11771,.T.) ;
#18298 = EDGE_CURVE('',#14357,#14367,#11772,.T.) ;
#18299 = EDGE_CURVE('',#14367,#14363,#8041,.T.) ;
#18300 = EDGE_CURVE('',#14367,#14358,#11773,.T.) ;
#18301 = EDGE_CURVE('',#14356,#14368,#8042,.T.) ;
#18302 = EDGE_CURVE('',#14368,#14364,#11774,.T.) ;
#18303 = EDGE_CURVE('',#14365,#14368,#11775,.T.) ;
#18304 = EDGE_CURVE('',#14369,#14368,#11776,.T.) ;
#18305 = EDGE_CURVE('',#14370,#14370,#11777,.T.) ;
#18306 = EDGE_CURVE('',#14370,#14371,#8043,.T.) ;
#18307 = EDGE_CURVE('',#14371,#14371,#11778,.T.) ;
#18308 = EDGE_CURVE('',#14372,#14373,#8044,.T.) ;
#18309 = EDGE_CURVE('',#14374,#14372,#8045,.T.) ;
#18310 = EDGE_CURVE('',#14375,#14374,#8046,.T.) ;
#18311 = EDGE_CURVE('',#14373,#14375,#8047,.T.) ;
#18312 = EDGE_CURVE('',#14376,#14377,#8048,.T.) ;
#18313 = EDGE_CURVE('',#14377,#14373,#8049,.T.) ;
#18314 = EDGE_CURVE('',#14375,#14378,#8050,.T.) ;
#18315 = EDGE_CURVE('',#14378,#14376,#8051,.T.) ;
#18316 = EDGE_CURVE('',#14379,#14380,#8052,.T.) ;
#18317 = EDGE_CURVE('',#14380,#14381,#8053,.T.) ;
#18318 = EDGE_CURVE('',#14381,#14374,#8054,.T.) ;
#18319 = EDGE_CURVE('',#14372,#14379,#8055,.T.) ;
#18320 = EDGE_CURVE('',#14378,#14381,#8056,.T.) ;
#18321 = EDGE_CURVE('',#14376,#14380,#8057,.T.) ;
#18322 = EDGE_CURVE('',#14377,#14379,#8058,.T.) ;
#18323 = EDGE_CURVE('',#14382,#14382,#11779,.T.) ;
#18324 = EDGE_CURVE('',#14383,#14384,#8059,.T.) ;
#18325 = EDGE_CURVE('',#14384,#14383,#11780,.T.) ;
#18326 = EDGE_CURVE('',#14382,#14385,#8060,.T.) ;
#18327 = EDGE_CURVE('',#14385,#14386,#38,.T.) ;
#18328 = EDGE_CURVE('',#14386,#14384,#8061,.T.) ;
#18329 = EDGE_CURVE('',#14383,#14384,#11781,.T.) ;
#18330 = EDGE_CURVE('',#14386,#14385,#39,.T.) ;
#18331 = EDGE_CURVE('',#14387,#14388,#40,.T.) ;
#18332 = EDGE_CURVE('',#14388,#14387,#41,.T.) ;
#18333 = EDGE_CURVE('',#14388,#14386,#8062,.T.) ;
#18334 = EDGE_CURVE('',#14389,#14390,#42,.T.) ;
#18335 = EDGE_CURVE('',#14390,#14389,#43,.T.) ;
#18336 = EDGE_CURVE('',#14390,#14391,#8063,.T.) ;
#18337 = EDGE_CURVE('',#14392,#14391,#44,.T.) ;
#18338 = EDGE_CURVE('',#14391,#14392,#45,.T.) ;
#18339 = EDGE_CURVE('',#14393,#14394,#8064,.T.) ;
#18340 = EDGE_CURVE('',#14393,#14394,#11782,.T.) ;
#18341 = EDGE_CURVE('',#14394,#14393,#11783,.T.) ;
#18342 = EDGE_CURVE('',#14394,#14392,#8065,.T.) ;
#18343 = EDGE_CURVE('',#14391,#14395,#8066,.T.) ;
#18344 = EDGE_CURVE('',#14395,#14395,#11784,.T.) ;
#18345 = EDGE_CURVE('',#14396,#14397,#8067,.T.) ;
#18346 = EDGE_CURVE('',#14398,#14396,#8068,.T.) ;
#18347 = EDGE_CURVE('',#14399,#14398,#8069,.T.) ;
#18348 = EDGE_CURVE('',#14400,#14399,#11785,.T.) ;
#18349 = EDGE_CURVE('',#14401,#14400,#8070,.T.) ;
#18350 = EDGE_CURVE('',#14401,#14402,#8071,.T.) ;
#18351 = EDGE_CURVE('',#14403,#14402,#8072,.T.) ;
#18352 = EDGE_CURVE('',#14397,#14403,#11786,.T.) ;
#18353 = EDGE_CURVE('',#14404,#14405,#8073,.T.) ;
#18354 = EDGE_CURVE('',#14403,#14397,#11787,.T.) ;
#18355 = EDGE_CURVE('',#14406,#14406,#11788,.T.) ;
#18356 = EDGE_CURVE('',#14399,#14400,#11789,.T.) ;
#18357 = EDGE_CURVE('',#14407,#14407,#11790,.T.) ;
#18358 = EDGE_CURVE('',#14407,#14406,#8074,.T.) ;
#18359 = EDGE_CURVE('',#14408,#14408,#11791,.T.) ;
#18360 = EDGE_CURVE('',#14408,#14409,#8075,.T.) ;
#18361 = EDGE_CURVE('',#14409,#14409,#11792,.T.) ;
#18362 = EDGE_CURVE('',#14410,#14410,#11793,.T.) ;
#18363 = EDGE_CURVE('',#14410,#14411,#8076,.T.) ;
#18364 = EDGE_CURVE('',#14411,#14411,#11794,.T.) ;
#18365 = EDGE_CURVE('',#14412,#14413,#8077,.T.) ;
#18366 = EDGE_CURVE('',#14414,#14412,#11795,.T.) ;
#18367 = EDGE_CURVE('',#14415,#14414,#8078,.T.) ;
#18368 = EDGE_CURVE('',#14413,#14415,#11796,.T.) ;
#18369 = EDGE_CURVE('',#14416,#14412,#8079,.T.) ;
#18370 = EDGE_CURVE('',#14416,#14417,#8080,.T.) ;
#18371 = EDGE_CURVE('',#14418,#14417,#8081,.T.) ;
#18372 = EDGE_CURVE('',#14419,#14418,#8082,.T.) ;
#18373 = EDGE_CURVE('',#14414,#14419,#8083,.T.) ;
#18374 = EDGE_CURVE('',#14413,#14420,#8084,.T.) ;
#18375 = EDGE_CURVE('',#14420,#14416,#8085,.T.) ;
#18376 = EDGE_CURVE('',#14419,#14421,#8086,.T.) ;
#18377 = EDGE_CURVE('',#14421,#14415,#8087,.T.) ;
#18378 = EDGE_CURVE('',#14422,#14423,#8088,.T.) ;
#18379 = EDGE_CURVE('',#14423,#14418,#8089,.T.) ;
#18380 = EDGE_CURVE('',#14417,#14422,#8090,.T.) ;
#18381 = EDGE_CURVE('',#14421,#14423,#8091,.T.) ;
#18382 = EDGE_CURVE('',#14420,#14422,#8092,.T.) ;
#18383 = EDGE_CURVE('',#14424,#14425,#8093,.T.) ;
#18384 = EDGE_CURVE('',#14425,#14426,#8094,.T.) ;
#18385 = EDGE_CURVE('',#14426,#14427,#8095,.T.) ;
#18386 = EDGE_CURVE('',#14427,#14424,#8096,.T.) ;
#18387 = EDGE_CURVE('',#14428,#14429,#8097,.T.) ;
#18388 = EDGE_CURVE('',#14429,#14430,#8098,.T.) ;
#18389 = EDGE_CURVE('',#14430,#14431,#8099,.T.) ;
#18390 = EDGE_CURVE('',#14431,#14428,#8100,.T.) ;
#18391 = EDGE_CURVE('',#14427,#14430,#8101,.T.) ;
#18392 = EDGE_CURVE('',#14424,#14429,#8102,.T.) ;
#18393 = EDGE_CURVE('',#14426,#14431,#8103,.T.) ;
#18394 = EDGE_CURVE('',#14425,#14428,#8104,.T.) ;
#18395 = EDGE_CURVE('',#14432,#14433,#8105,.T.) ;
#18396 = EDGE_CURVE('',#14434,#14432,#8106,.T.) ;
#18397 = EDGE_CURVE('',#14435,#14434,#8107,.T.) ;
#18398 = EDGE_CURVE('',#14436,#14435,#8108,.T.) ;
#18399 = EDGE_CURVE('',#14436,#14437,#8109,.T.) ;
#18400 = EDGE_CURVE('',#14433,#14437,#8110,.T.) ;
#18401 = EDGE_CURVE('',#14438,#14434,#675,.T.) ;
#18402 = EDGE_CURVE('',#14439,#14438,#8111,.T.) ;
#18403 = EDGE_CURVE('',#14435,#14439,#8112,.T.) ;
#18404 = EDGE_CURVE('',#14439,#14440,#8113,.T.) ;
#18405 = EDGE_CURVE('',#14440,#14436,#8114,.T.) ;
#18406 = EDGE_CURVE('',#14433,#14441,#8115,.T.) ;
#18407 = EDGE_CURVE('',#14437,#14442,#8116,.T.) ;
#18408 = EDGE_CURVE('',#14442,#14441,#8117,.T.) ;
#18409 = EDGE_CURVE('',#14440,#14442,#8118,.T.) ;
#18410 = EDGE_CURVE('',#14441,#14443,#8119,.T.) ;
#18411 = EDGE_CURVE('',#14443,#14438,#8120,.T.) ;
#18412 = EDGE_CURVE('',#14443,#14444,#11797,.T.) ;
#18413 = EDGE_CURVE('',#14444,#14432,#11798,.T.) ;
#18414 = EDGE_CURVE('',#14445,#14445,#11799,.T.) ;
#18415 = EDGE_CURVE('',#14445,#14446,#8121,.T.) ;
#18416 = EDGE_CURVE('',#14446,#14446,#11800,.T.) ;
#18417 = EDGE_CURVE('',#14447,#14447,#11801,.T.) ;
#18418 = EDGE_CURVE('',#14447,#14444,#8122,.T.) ;
#18419 = EDGE_CURVE('',#14448,#14448,#11802,.T.) ;
#18420 = EDGE_CURVE('',#14448,#14449,#8123,.T.) ;
#18421 = EDGE_CURVE('',#14449,#14449,#11803,.T.) ;
#18422 = EDGE_CURVE('',#14450,#14451,#8124,.T.) ;
#18423 = EDGE_CURVE('',#14450,#14452,#8125,.T.) ;
#18424 = EDGE_CURVE('',#14453,#14452,#8126,.T.) ;
#18425 = EDGE_CURVE('',#14453,#14451,#8127,.T.) ;
#18426 = EDGE_CURVE('',#14454,#14455,#8128,.T.) ;
#18427 = EDGE_CURVE('',#14454,#14456,#8129,.T.) ;
#18428 = EDGE_CURVE('',#14457,#14456,#8130,.T.) ;
#18429 = EDGE_CURVE('',#14457,#14455,#8131,.T.) ;
#18430 = EDGE_CURVE('',#14458,#14450,#8132,.T.) ;
#18431 = EDGE_CURVE('',#14456,#14458,#8133,.T.) ;
#18432 = EDGE_CURVE('',#14459,#14454,#8134,.T.) ;
#18433 = EDGE_CURVE('',#14452,#14459,#8135,.T.) ;
#18434 = EDGE_CURVE('',#14458,#14460,#8136,.T.) ;
#18435 = EDGE_CURVE('',#14451,#14460,#8137,.T.) ;
#18436 = EDGE_CURVE('',#14459,#14461,#8138,.T.) ;
#18437 = EDGE_CURVE('',#14455,#14461,#8139,.T.) ;
#18438 = EDGE_CURVE('',#14460,#14457,#8140,.T.) ;
#18439 = EDGE_CURVE('',#14461,#14453,#8141,.T.) ;
#18440 = EDGE_CURVE('',#14462,#14462,#11804,.T.) ;
#18441 = EDGE_CURVE('',#14462,#14463,#8142,.T.) ;
#18442 = EDGE_CURVE('',#14463,#14463,#11805,.T.) ;
#18443 = EDGE_CURVE('',#14464,#14465,#8143,.T.) ;
#18444 = EDGE_CURVE('',#14464,#14466,#8144,.T.) ;
#18445 = EDGE_CURVE('',#14467,#14466,#8145,.T.) ;
#18446 = EDGE_CURVE('',#14467,#14465,#8146,.T.) ;
#18447 = EDGE_CURVE('',#14468,#14469,#8147,.T.) ;
#18448 = EDGE_CURVE('',#14468,#14470,#8148,.T.) ;
#18449 = EDGE_CURVE('',#14471,#14470,#8149,.T.) ;
#18450 = EDGE_CURVE('',#14471,#14469,#8150,.T.) ;
#18451 = EDGE_CURVE('',#14472,#14464,#8151,.T.) ;
#18452 = EDGE_CURVE('',#14470,#14472,#8152,.T.) ;
#18453 = EDGE_CURVE('',#14473,#14468,#8153,.T.) ;
#18454 = EDGE_CURVE('',#14466,#14473,#8154,.T.) ;
#18455 = EDGE_CURVE('',#14472,#14474,#8155,.T.) ;
#18456 = EDGE_CURVE('',#14465,#14474,#8156,.T.) ;
#18457 = EDGE_CURVE('',#14473,#14475,#8157,.T.) ;
#18458 = EDGE_CURVE('',#14469,#14475,#8158,.T.) ;
#18459 = EDGE_CURVE('',#14474,#14471,#8159,.T.) ;
#18460 = EDGE_CURVE('',#14475,#14467,#8160,.T.) ;
#18461 = EDGE_CURVE('',#14476,#14476,#11806,.T.) ;
#18462 = EDGE_CURVE('',#14476,#14477,#8161,.T.) ;
#18463 = EDGE_CURVE('',#14477,#14477,#11807,.T.) ;
#18464 = EDGE_CURVE('',#14478,#14479,#8162,.T.) ;
#18465 = EDGE_CURVE('',#14478,#14480,#8163,.T.) ;
#18466 = EDGE_CURVE('',#14481,#14480,#8164,.T.) ;
#18467 = EDGE_CURVE('',#14481,#14479,#8165,.T.) ;
#18468 = EDGE_CURVE('',#14482,#14483,#8166,.T.) ;
#18469 = EDGE_CURVE('',#14482,#14484,#8167,.T.) ;
#18470 = EDGE_CURVE('',#14485,#14484,#8168,.T.) ;
#18471 = EDGE_CURVE('',#14485,#14483,#8169,.T.) ;
#18472 = EDGE_CURVE('',#14486,#14478,#8170,.T.) ;
#18473 = EDGE_CURVE('',#14484,#14486,#8171,.T.) ;
#18474 = EDGE_CURVE('',#14487,#14482,#8172,.T.) ;
#18475 = EDGE_CURVE('',#14480,#14487,#8173,.T.) ;
#18476 = EDGE_CURVE('',#14486,#14488,#8174,.T.) ;
#18477 = EDGE_CURVE('',#14479,#14488,#8175,.T.) ;
#18478 = EDGE_CURVE('',#14487,#14489,#8176,.T.) ;
#18479 = EDGE_CURVE('',#14483,#14489,#8177,.T.) ;
#18480 = EDGE_CURVE('',#14488,#14485,#8178,.T.) ;
#18481 = EDGE_CURVE('',#14489,#14481,#8179,.T.) ;
#18482 = EDGE_CURVE('',#14490,#14490,#11808,.T.) ;
#18483 = EDGE_CURVE('',#14490,#14491,#8180,.T.) ;
#18484 = EDGE_CURVE('',#14491,#14491,#11809,.T.) ;
#18485 = EDGE_CURVE('',#14492,#14493,#8181,.T.) ;
#18486 = EDGE_CURVE('',#14492,#14494,#8182,.T.) ;
#18487 = EDGE_CURVE('',#14495,#14494,#8183,.T.) ;
#18488 = EDGE_CURVE('',#14495,#14493,#8184,.T.) ;
#18489 = EDGE_CURVE('',#14496,#14497,#8185,.T.) ;
#18490 = EDGE_CURVE('',#14496,#14498,#8186,.T.) ;
#18491 = EDGE_CURVE('',#14499,#14498,#8187,.T.) ;
#18492 = EDGE_CURVE('',#14499,#14497,#8188,.T.) ;
#18493 = EDGE_CURVE('',#14500,#14492,#8189,.T.) ;
#18494 = EDGE_CURVE('',#14498,#14500,#8190,.T.) ;
#18495 = EDGE_CURVE('',#14501,#14496,#8191,.T.) ;
#18496 = EDGE_CURVE('',#14494,#14501,#8192,.T.) ;
#18497 = EDGE_CURVE('',#14500,#14502,#8193,.T.) ;
#18498 = EDGE_CURVE('',#14493,#14502,#8194,.T.) ;
#18499 = EDGE_CURVE('',#14501,#14503,#8195,.T.) ;
#18500 = EDGE_CURVE('',#14497,#14503,#8196,.T.) ;
#18501 = EDGE_CURVE('',#14502,#14499,#8197,.T.) ;
#18502 = EDGE_CURVE('',#14503,#14495,#8198,.T.) ;
#18503 = EDGE_CURVE('',#14504,#14504,#11810,.T.) ;
#18504 = EDGE_CURVE('',#14505,#14505,#11811,.T.) ;
#18505 = EDGE_CURVE('',#14506,#14506,#11812,.T.) ;
#18506 = EDGE_CURVE('',#14506,#14504,#8199,.T.) ;
#18507 = EDGE_CURVE('',#14505,#14507,#8200,.T.) ;
#18508 = EDGE_CURVE('',#14507,#14507,#11813,.T.) ;
#18509 = EDGE_CURVE('',#14508,#14508,#11814,.T.) ;
#18510 = EDGE_CURVE('',#14509,#14509,#11815,.T.) ;
#18511 = EDGE_CURVE('',#14510,#14510,#11816,.T.) ;
#18512 = EDGE_CURVE('',#14510,#14508,#8201,.T.) ;
#18513 = EDGE_CURVE('',#14509,#14511,#8202,.T.) ;
#18514 = EDGE_CURVE('',#14511,#14511,#11817,.T.) ;
#18515 = EDGE_CURVE('',#14512,#14513,#676,.T.) ;
#18516 = EDGE_CURVE('',#14514,#14512,#46,.T.) ;
#18517 = EDGE_CURVE('',#14515,#14514,#677,.T.) ;
#18518 = EDGE_CURVE('',#14515,#14516,#678,.T.) ;
#18519 = EDGE_CURVE('',#14516,#14517,#8203,.T.) ;
#18520 = EDGE_CURVE('',#14518,#14517,#679,.T.) ;
#18521 = EDGE_CURVE('',#14519,#14518,#11818,.T.) ;
#18522 = EDGE_CURVE('',#14517,#14519,#680,.T.) ;
#18523 = EDGE_CURVE('',#14516,#14513,#681,.T.) ;
#18524 = EDGE_CURVE('',#14520,#14521,#11819,.T.) ;
#18525 = EDGE_CURVE('',#14521,#14520,#11820,.T.) ;
#18526 = EDGE_CURVE('',#14522,#14523,#11821,.T.) ;
#18527 = EDGE_CURVE('',#14523,#14522,#11822,.T.) ;
#18528 = EDGE_CURVE('',#14524,#14525,#11823,.T.) ;
#18529 = EDGE_CURVE('',#14525,#14524,#11824,.T.) ;
#18530 = EDGE_CURVE('',#14526,#14527,#11825,.T.) ;
#18531 = EDGE_CURVE('',#14527,#14528,#11826,.T.) ;
#18532 = EDGE_CURVE('',#14529,#14528,#11827,.T.) ;
#18533 = EDGE_CURVE('',#14528,#14526,#11828,.T.) ;
#18534 = EDGE_CURVE('',#14530,#14531,#11829,.T.) ;
#18535 = EDGE_CURVE('',#14531,#14532,#11830,.T.) ;
#18536 = EDGE_CURVE('',#14532,#14533,#11831,.T.) ;
#18537 = EDGE_CURVE('',#14533,#14530,#11832,.T.) ;
#18538 = EDGE_CURVE('',#14534,#14535,#11833,.T.) ;
#18539 = EDGE_CURVE('',#14535,#14536,#11834,.T.) ;
#18540 = EDGE_CURVE('',#14536,#14537,#11835,.T.) ;
#18541 = EDGE_CURVE('',#14537,#14534,#11836,.T.) ;
#18542 = EDGE_CURVE('',#14538,#14539,#11837,.T.) ;
#18543 = EDGE_CURVE('',#14539,#14540,#11838,.T.) ;
#18544 = EDGE_CURVE('',#14540,#14541,#11839,.T.) ;
#18545 = EDGE_CURVE('',#14541,#14538,#11840,.T.) ;
#18546 = EDGE_CURVE('',#14542,#14543,#11841,.T.) ;
#18547 = EDGE_CURVE('',#14543,#14544,#11842,.T.) ;
#18548 = EDGE_CURVE('',#14544,#14545,#11843,.T.) ;
#18549 = EDGE_CURVE('',#14545,#14542,#11844,.T.) ;
#18550 = EDGE_CURVE('',#14546,#14547,#11845,.T.) ;
#18551 = EDGE_CURVE('',#14547,#14548,#11846,.T.) ;
#18552 = EDGE_CURVE('',#14548,#14549,#11847,.T.) ;
#18553 = EDGE_CURVE('',#14549,#14546,#11848,.T.) ;
#18554 = EDGE_CURVE('',#14518,#14519,#11849,.T.) ;
#18555 = EDGE_CURVE('',#14550,#14551,#11850,.T.) ;
#18556 = EDGE_CURVE('',#14551,#14550,#11851,.T.) ;
#18557 = EDGE_CURVE('',#14521,#14552,#682,.T.) ;
#18558 = EDGE_CURVE('',#14552,#14520,#683,.T.) ;
#18559 = EDGE_CURVE('',#14552,#14553,#8204,.T.) ;
#18560 = EDGE_CURVE('',#14523,#14553,#684,.T.) ;
#18561 = EDGE_CURVE('',#14553,#14522,#685,.T.) ;
#18562 = EDGE_CURVE('',#14553,#14554,#8205,.T.) ;
#18563 = EDGE_CURVE('',#14525,#14554,#686,.T.) ;
#18564 = EDGE_CURVE('',#14554,#14524,#687,.T.) ;
#18565 = EDGE_CURVE('',#14554,#14555,#8206,.T.) ;
#18566 = EDGE_CURVE('',#14527,#14555,#688,.T.) ;
#18567 = EDGE_CURVE('',#14555,#14526,#689,.T.) ;
#18568 = EDGE_CURVE('',#14528,#14531,#8207,.T.) ;
#18569 = EDGE_CURVE('',#14532,#14530,#690,.T.) ;
#18570 = EDGE_CURVE('',#14533,#14535,#8208,.T.) ;
#18571 = EDGE_CURVE('',#14536,#14534,#691,.T.) ;
#18572 = EDGE_CURVE('',#14537,#14539,#8209,.T.) ;
#18573 = EDGE_CURVE('',#14540,#14538,#692,.T.) ;
#18574 = EDGE_CURVE('',#14541,#14543,#8210,.T.) ;
#18575 = EDGE_CURVE('',#14544,#14542,#693,.T.) ;
#18576 = EDGE_CURVE('',#14545,#14547,#8211,.T.) ;
#18577 = EDGE_CURVE('',#14548,#14546,#694,.T.) ;
#18578 = EDGE_CURVE('',#14549,#14556,#8212,.T.) ;
#18579 = EDGE_CURVE('',#14557,#14556,#47,.T.) ;
#18580 = EDGE_CURVE('',#14513,#14557,#695,.T.) ;
#18581 = EDGE_CURVE('',#14558,#14515,#696,.T.) ;
#18582 = EDGE_CURVE('',#14556,#14558,#48,.T.) ;
#18583 = EDGE_CURVE('',#14517,#14559,#8213,.T.) ;
#18584 = EDGE_CURVE('',#14551,#14559,#697,.T.) ;
#18585 = EDGE_CURVE('',#14559,#14550,#698,.T.) ;
#18586 = EDGE_CURVE('',#14559,#14552,#8214,.T.) ;
#18587 = EDGE_CURVE('',#14514,#14558,#11852,.T.) ;
#18588 = EDGE_CURVE('',#14556,#14560,#8215,.T.) ;
#18589 = EDGE_CURVE('',#14560,#14560,#11853,.T.) ;
#18590 = EDGE_CURVE('',#14557,#14512,#11854,.T.) ;
#18591 = ORIENTED_EDGE('',*,*,#14561,.F.) ;
#18592 = ORIENTED_EDGE('',*,*,#14562,.T.) ;
#18593 = ORIENTED_EDGE('',*,*,#14563,.F.) ;
#18594 = ORIENTED_EDGE('',*,*,#14562,.F.) ;
#18595 = ORIENTED_EDGE('',*,*,#14564,.F.) ;
#18596 = ORIENTED_EDGE('',*,*,#14565,.F.) ;
#18597 = ORIENTED_EDGE('',*,*,#14566,.T.) ;
#18598 = ORIENTED_EDGE('',*,*,#14567,.F.) ;
#18599 = ORIENTED_EDGE('',*,*,#14568,.F.) ;
#18600 = ORIENTED_EDGE('',*,*,#14569,.F.) ;
#18601 = ORIENTED_EDGE('',*,*,#14570,.T.) ;
#18602 = ORIENTED_EDGE('',*,*,#14571,.F.) ;
#18603 = ORIENTED_EDGE('',*,*,#14561,.T.) ;
#18604 = ORIENTED_EDGE('',*,*,#14572,.F.) ;
#18605 = ORIENTED_EDGE('',*,*,#14573,.T.) ;
#18606 = ORIENTED_EDGE('',*,*,#14574,.F.) ;
#18607 = ORIENTED_EDGE('',*,*,#14566,.F.) ;
#18608 = ORIENTED_EDGE('',*,*,#14569,.T.) ;
#18609 = ORIENTED_EDGE('',*,*,#14575,.T.) ;
#18610 = ORIENTED_EDGE('',*,*,#14576,.T.) ;
#18611 = ORIENTED_EDGE('',*,*,#14577,.T.) ;
#18612 = ORIENTED_EDGE('',*,*,#14578,.T.) ;
#18613 = ORIENTED_EDGE('',*,*,#14579,.F.) ;
#18614 = ORIENTED_EDGE('',*,*,#14570,.F.) ;
#18615 = ORIENTED_EDGE('',*,*,#14577,.F.) ;
#18616 = ORIENTED_EDGE('',*,*,#14580,.F.) ;
#18617 = ORIENTED_EDGE('',*,*,#14571,.T.) ;
#18618 = ORIENTED_EDGE('',*,*,#14579,.T.) ;
#18619 = ORIENTED_EDGE('',*,*,#14581,.T.) ;
#18620 = ORIENTED_EDGE('',*,*,#14567,.T.) ;
#18621 = ORIENTED_EDGE('',*,*,#14574,.T.) ;
#18622 = ORIENTED_EDGE('',*,*,#14582,.T.) ;
#18623 = ORIENTED_EDGE('',*,*,#14583,.T.) ;
#18624 = ORIENTED_EDGE('',*,*,#14584,.F.) ;
#18625 = ORIENTED_EDGE('',*,*,#14581,.F.) ;
#18626 = ORIENTED_EDGE('',*,*,#14578,.F.) ;
#18627 = ORIENTED_EDGE('',*,*,#14576,.F.) ;
#18628 = ORIENTED_EDGE('',*,*,#14585,.T.) ;
#18629 = ORIENTED_EDGE('',*,*,#14582,.F.) ;
#18630 = ORIENTED_EDGE('',*,*,#14573,.F.) ;
#18631 = ORIENTED_EDGE('',*,*,#14586,.F.) ;
#18632 = ORIENTED_EDGE('',*,*,#14563,.T.) ;
#18633 = ORIENTED_EDGE('',*,*,#14568,.T.) ;
#18634 = ORIENTED_EDGE('',*,*,#14583,.F.) ;
#18635 = ORIENTED_EDGE('',*,*,#14585,.F.) ;
#18636 = ORIENTED_EDGE('',*,*,#14575,.F.) ;
#18637 = ORIENTED_EDGE('',*,*,#14587,.F.) ;
#18638 = ORIENTED_EDGE('',*,*,#14588,.T.) ;
#18639 = ORIENTED_EDGE('',*,*,#14589,.F.) ;
#18640 = ORIENTED_EDGE('',*,*,#14590,.T.) ;
#18641 = ORIENTED_EDGE('',*,*,#14591,.T.) ;
#18642 = ORIENTED_EDGE('',*,*,#14592,.T.) ;
#18643 = ORIENTED_EDGE('',*,*,#14593,.F.) ;
#18644 = ORIENTED_EDGE('',*,*,#14564,.T.) ;
#18645 = ORIENTED_EDGE('',*,*,#14580,.T.) ;
#18646 = ORIENTED_EDGE('',*,*,#14584,.T.) ;
#18647 = ORIENTED_EDGE('',*,*,#14594,.F.) ;
#18648 = ORIENTED_EDGE('',*,*,#14588,.F.) ;
#18649 = ORIENTED_EDGE('',*,*,#14595,.F.) ;
#18650 = ORIENTED_EDGE('',*,*,#14596,.T.) ;
#18651 = ORIENTED_EDGE('',*,*,#14597,.F.) ;
#18652 = ORIENTED_EDGE('',*,*,#14596,.F.) ;
#18653 = ORIENTED_EDGE('',*,*,#14590,.F.) ;
#18654 = ORIENTED_EDGE('',*,*,#14598,.F.) ;
#18655 = ORIENTED_EDGE('',*,*,#14599,.T.) ;
#18656 = ORIENTED_EDGE('',*,*,#14600,.F.) ;
#18657 = ORIENTED_EDGE('',*,*,#14601,.F.) ;
#18658 = ORIENTED_EDGE('',*,*,#14602,.F.) ;
#18659 = ORIENTED_EDGE('',*,*,#14603,.T.) ;
#18660 = ORIENTED_EDGE('',*,*,#14604,.F.) ;
#18661 = ORIENTED_EDGE('',*,*,#14597,.T.) ;
#18662 = ORIENTED_EDGE('',*,*,#14605,.F.) ;
#18663 = ORIENTED_EDGE('',*,*,#14606,.T.) ;
#18664 = ORIENTED_EDGE('',*,*,#14607,.F.) ;
#18665 = ORIENTED_EDGE('',*,*,#14599,.F.) ;
#18666 = ORIENTED_EDGE('',*,*,#14602,.T.) ;
#18667 = ORIENTED_EDGE('',*,*,#14608,.T.) ;
#18668 = ORIENTED_EDGE('',*,*,#14609,.T.) ;
#18669 = ORIENTED_EDGE('',*,*,#14610,.T.) ;
#18670 = ORIENTED_EDGE('',*,*,#14611,.T.) ;
#18671 = ORIENTED_EDGE('',*,*,#14612,.F.) ;
#18672 = ORIENTED_EDGE('',*,*,#14603,.F.) ;
#18673 = ORIENTED_EDGE('',*,*,#14610,.F.) ;
#18674 = ORIENTED_EDGE('',*,*,#14591,.F.) ;
#18675 = ORIENTED_EDGE('',*,*,#14604,.T.) ;
#18676 = ORIENTED_EDGE('',*,*,#14612,.T.) ;
#18677 = ORIENTED_EDGE('',*,*,#14613,.T.) ;
#18678 = ORIENTED_EDGE('',*,*,#14600,.T.) ;
#18679 = ORIENTED_EDGE('',*,*,#14607,.T.) ;
#18680 = ORIENTED_EDGE('',*,*,#14614,.T.) ;
#18681 = ORIENTED_EDGE('',*,*,#14615,.T.) ;
#18682 = ORIENTED_EDGE('',*,*,#14592,.F.) ;
#18683 = ORIENTED_EDGE('',*,*,#14613,.F.) ;
#18684 = ORIENTED_EDGE('',*,*,#14611,.F.) ;
#18685 = ORIENTED_EDGE('',*,*,#14609,.F.) ;
#18686 = ORIENTED_EDGE('',*,*,#14616,.T.) ;
#18687 = ORIENTED_EDGE('',*,*,#14614,.F.) ;
#18688 = ORIENTED_EDGE('',*,*,#14606,.F.) ;
#18689 = ORIENTED_EDGE('',*,*,#14617,.F.) ;
#18690 = ORIENTED_EDGE('',*,*,#14595,.T.) ;
#18691 = ORIENTED_EDGE('',*,*,#14601,.T.) ;
#18692 = ORIENTED_EDGE('',*,*,#14615,.F.) ;
#18693 = ORIENTED_EDGE('',*,*,#14616,.F.) ;
#18694 = ORIENTED_EDGE('',*,*,#14608,.F.) ;
#18695 = ORIENTED_EDGE('',*,*,#14618,.F.) ;
#18696 = ORIENTED_EDGE('',*,*,#14619,.T.) ;
#18697 = ORIENTED_EDGE('',*,*,#14620,.T.) ;
#18698 = ORIENTED_EDGE('',*,*,#14621,.T.) ;
#18699 = ORIENTED_EDGE('',*,*,#14622,.F.) ;
#18700 = ORIENTED_EDGE('',*,*,#14623,.F.) ;
#18701 = ORIENTED_EDGE('',*,*,#14624,.F.) ;
#18702 = ORIENTED_EDGE('',*,*,#14619,.F.) ;
#18703 = ORIENTED_EDGE('',*,*,#14625,.F.) ;
#18704 = ORIENTED_EDGE('',*,*,#14621,.F.) ;
#18705 = ORIENTED_EDGE('',*,*,#14626,.T.) ;
#18706 = ORIENTED_EDGE('',*,*,#14627,.F.) ;
#18707 = ORIENTED_EDGE('',*,*,#14628,.F.) ;
#18708 = ORIENTED_EDGE('',*,*,#14629,.F.) ;
#18709 = ORIENTED_EDGE('',*,*,#14630,.F.) ;
#18710 = ORIENTED_EDGE('',*,*,#14631,.F.) ;
#18711 = ORIENTED_EDGE('',*,*,#14632,.F.) ;
#18712 = ORIENTED_EDGE('',*,*,#14627,.T.) ;
#18713 = ORIENTED_EDGE('',*,*,#14633,.T.) ;
#18714 = ORIENTED_EDGE('',*,*,#14623,.T.) ;
#18715 = ORIENTED_EDGE('',*,*,#14634,.F.) ;
#18716 = ORIENTED_EDGE('',*,*,#14635,.T.) ;
#18717 = ORIENTED_EDGE('',*,*,#14636,.T.) ;
#18718 = ORIENTED_EDGE('',*,*,#14629,.T.) ;
#18719 = ORIENTED_EDGE('',*,*,#14637,.F.) ;
#18720 = ORIENTED_EDGE('',*,*,#14631,.T.) ;
#18721 = ORIENTED_EDGE('',*,*,#14638,.T.) ;
#18722 = ORIENTED_EDGE('',*,*,#14639,.T.) ;
#18723 = ORIENTED_EDGE('',*,*,#14640,.F.) ;
#18724 = ORIENTED_EDGE('',*,*,#14639,.F.) ;
#18725 = ORIENTED_EDGE('',*,*,#14641,.T.) ;
#18726 = ORIENTED_EDGE('',*,*,#14635,.F.) ;
#18727 = ORIENTED_EDGE('',*,*,#14630,.T.) ;
#18728 = ORIENTED_EDGE('',*,*,#14636,.F.) ;
#18729 = ORIENTED_EDGE('',*,*,#14641,.F.) ;
#18730 = ORIENTED_EDGE('',*,*,#14638,.F.) ;
#18731 = ORIENTED_EDGE('',*,*,#14624,.T.) ;
#18732 = ORIENTED_EDGE('',*,*,#14633,.F.) ;
#18733 = ORIENTED_EDGE('',*,*,#14626,.F.) ;
#18734 = ORIENTED_EDGE('',*,*,#14620,.F.) ;
#18735 = ORIENTED_EDGE('',*,*,#14642,.F.) ;
#18736 = ORIENTED_EDGE('',*,*,#14643,.T.) ;
#18737 = ORIENTED_EDGE('',*,*,#14644,.T.) ;
#18738 = ORIENTED_EDGE('',*,*,#14645,.T.) ;
#18739 = ORIENTED_EDGE('',*,*,#14646,.F.) ;
#18740 = ORIENTED_EDGE('',*,*,#14647,.F.) ;
#18741 = ORIENTED_EDGE('',*,*,#14648,.F.) ;
#18742 = ORIENTED_EDGE('',*,*,#14643,.F.) ;
#18743 = ORIENTED_EDGE('',*,*,#14649,.F.) ;
#18744 = ORIENTED_EDGE('',*,*,#14645,.F.) ;
#18745 = ORIENTED_EDGE('',*,*,#14650,.T.) ;
#18746 = ORIENTED_EDGE('',*,*,#14651,.F.) ;
#18747 = ORIENTED_EDGE('',*,*,#14652,.F.) ;
#18748 = ORIENTED_EDGE('',*,*,#14653,.F.) ;
#18749 = ORIENTED_EDGE('',*,*,#14654,.F.) ;
#18750 = ORIENTED_EDGE('',*,*,#14655,.F.) ;
#18751 = ORIENTED_EDGE('',*,*,#14656,.F.) ;
#18752 = ORIENTED_EDGE('',*,*,#14651,.T.) ;
#18753 = ORIENTED_EDGE('',*,*,#14657,.T.) ;
#18754 = ORIENTED_EDGE('',*,*,#14647,.T.) ;
#18755 = ORIENTED_EDGE('',*,*,#14658,.F.) ;
#18756 = ORIENTED_EDGE('',*,*,#14659,.T.) ;
#18757 = ORIENTED_EDGE('',*,*,#14660,.T.) ;
#18758 = ORIENTED_EDGE('',*,*,#14653,.T.) ;
#18759 = ORIENTED_EDGE('',*,*,#14661,.F.) ;
#18760 = ORIENTED_EDGE('',*,*,#14655,.T.) ;
#18761 = ORIENTED_EDGE('',*,*,#14662,.T.) ;
#18762 = ORIENTED_EDGE('',*,*,#14663,.T.) ;
#18763 = ORIENTED_EDGE('',*,*,#14664,.F.) ;
#18764 = ORIENTED_EDGE('',*,*,#14663,.F.) ;
#18765 = ORIENTED_EDGE('',*,*,#14665,.T.) ;
#18766 = ORIENTED_EDGE('',*,*,#14659,.F.) ;
#18767 = ORIENTED_EDGE('',*,*,#14654,.T.) ;
#18768 = ORIENTED_EDGE('',*,*,#14660,.F.) ;
#18769 = ORIENTED_EDGE('',*,*,#14665,.F.) ;
#18770 = ORIENTED_EDGE('',*,*,#14662,.F.) ;
#18771 = ORIENTED_EDGE('',*,*,#14648,.T.) ;
#18772 = ORIENTED_EDGE('',*,*,#14657,.F.) ;
#18773 = ORIENTED_EDGE('',*,*,#14650,.F.) ;
#18774 = ORIENTED_EDGE('',*,*,#14644,.F.) ;
#18775 = ORIENTED_EDGE('',*,*,#14666,.F.) ;
#18776 = ORIENTED_EDGE('',*,*,#14667,.T.) ;
#18777 = ORIENTED_EDGE('',*,*,#14668,.T.) ;
#18778 = ORIENTED_EDGE('',*,*,#14669,.T.) ;
#18779 = ORIENTED_EDGE('',*,*,#14670,.F.) ;
#18780 = ORIENTED_EDGE('',*,*,#14671,.F.) ;
#18781 = ORIENTED_EDGE('',*,*,#14672,.F.) ;
#18782 = ORIENTED_EDGE('',*,*,#14667,.F.) ;
#18783 = ORIENTED_EDGE('',*,*,#14673,.F.) ;
#18784 = ORIENTED_EDGE('',*,*,#14669,.F.) ;
#18785 = ORIENTED_EDGE('',*,*,#14674,.T.) ;
#18786 = ORIENTED_EDGE('',*,*,#14675,.F.) ;
#18787 = ORIENTED_EDGE('',*,*,#14676,.F.) ;
#18788 = ORIENTED_EDGE('',*,*,#14677,.F.) ;
#18789 = ORIENTED_EDGE('',*,*,#14678,.F.) ;
#18790 = ORIENTED_EDGE('',*,*,#14679,.F.) ;
#18791 = ORIENTED_EDGE('',*,*,#14680,.F.) ;
#18792 = ORIENTED_EDGE('',*,*,#14675,.T.) ;
#18793 = ORIENTED_EDGE('',*,*,#14681,.T.) ;
#18794 = ORIENTED_EDGE('',*,*,#14671,.T.) ;
#18795 = ORIENTED_EDGE('',*,*,#14682,.F.) ;
#18796 = ORIENTED_EDGE('',*,*,#14683,.T.) ;
#18797 = ORIENTED_EDGE('',*,*,#14684,.T.) ;
#18798 = ORIENTED_EDGE('',*,*,#14677,.T.) ;
#18799 = ORIENTED_EDGE('',*,*,#14685,.F.) ;
#18800 = ORIENTED_EDGE('',*,*,#14679,.T.) ;
#18801 = ORIENTED_EDGE('',*,*,#14686,.T.) ;
#18802 = ORIENTED_EDGE('',*,*,#14687,.T.) ;
#18803 = ORIENTED_EDGE('',*,*,#14688,.F.) ;
#18804 = ORIENTED_EDGE('',*,*,#14687,.F.) ;
#18805 = ORIENTED_EDGE('',*,*,#14689,.T.) ;
#18806 = ORIENTED_EDGE('',*,*,#14683,.F.) ;
#18807 = ORIENTED_EDGE('',*,*,#14678,.T.) ;
#18808 = ORIENTED_EDGE('',*,*,#14684,.F.) ;
#18809 = ORIENTED_EDGE('',*,*,#14689,.F.) ;
#18810 = ORIENTED_EDGE('',*,*,#14686,.F.) ;
#18811 = ORIENTED_EDGE('',*,*,#14672,.T.) ;
#18812 = ORIENTED_EDGE('',*,*,#14681,.F.) ;
#18813 = ORIENTED_EDGE('',*,*,#14674,.F.) ;
#18814 = ORIENTED_EDGE('',*,*,#14668,.F.) ;
#18815 = ORIENTED_EDGE('',*,*,#14690,.F.) ;
#18816 = ORIENTED_EDGE('',*,*,#14691,.T.) ;
#18817 = ORIENTED_EDGE('',*,*,#14692,.T.) ;
#18818 = ORIENTED_EDGE('',*,*,#14693,.T.) ;
#18819 = ORIENTED_EDGE('',*,*,#14694,.F.) ;
#18820 = ORIENTED_EDGE('',*,*,#14695,.F.) ;
#18821 = ORIENTED_EDGE('',*,*,#14696,.F.) ;
#18822 = ORIENTED_EDGE('',*,*,#14691,.F.) ;
#18823 = ORIENTED_EDGE('',*,*,#14697,.F.) ;
#18824 = ORIENTED_EDGE('',*,*,#14693,.F.) ;
#18825 = ORIENTED_EDGE('',*,*,#14698,.T.) ;
#18826 = ORIENTED_EDGE('',*,*,#14699,.F.) ;
#18827 = ORIENTED_EDGE('',*,*,#14700,.F.) ;
#18828 = ORIENTED_EDGE('',*,*,#14701,.F.) ;
#18829 = ORIENTED_EDGE('',*,*,#14702,.F.) ;
#18830 = ORIENTED_EDGE('',*,*,#14703,.F.) ;
#18831 = ORIENTED_EDGE('',*,*,#14704,.F.) ;
#18832 = ORIENTED_EDGE('',*,*,#14699,.T.) ;
#18833 = ORIENTED_EDGE('',*,*,#14705,.T.) ;
#18834 = ORIENTED_EDGE('',*,*,#14695,.T.) ;
#18835 = ORIENTED_EDGE('',*,*,#14706,.F.) ;
#18836 = ORIENTED_EDGE('',*,*,#14707,.T.) ;
#18837 = ORIENTED_EDGE('',*,*,#14708,.T.) ;
#18838 = ORIENTED_EDGE('',*,*,#14701,.T.) ;
#18839 = ORIENTED_EDGE('',*,*,#14709,.F.) ;
#18840 = ORIENTED_EDGE('',*,*,#14703,.T.) ;
#18841 = ORIENTED_EDGE('',*,*,#14710,.T.) ;
#18842 = ORIENTED_EDGE('',*,*,#14711,.T.) ;
#18843 = ORIENTED_EDGE('',*,*,#14712,.F.) ;
#18844 = ORIENTED_EDGE('',*,*,#14711,.F.) ;
#18845 = ORIENTED_EDGE('',*,*,#14713,.T.) ;
#18846 = ORIENTED_EDGE('',*,*,#14707,.F.) ;
#18847 = ORIENTED_EDGE('',*,*,#14702,.T.) ;
#18848 = ORIENTED_EDGE('',*,*,#14708,.F.) ;
#18849 = ORIENTED_EDGE('',*,*,#14713,.F.) ;
#18850 = ORIENTED_EDGE('',*,*,#14710,.F.) ;
#18851 = ORIENTED_EDGE('',*,*,#14696,.T.) ;
#18852 = ORIENTED_EDGE('',*,*,#14705,.F.) ;
#18853 = ORIENTED_EDGE('',*,*,#14698,.F.) ;
#18854 = ORIENTED_EDGE('',*,*,#14692,.F.) ;
#18855 = ORIENTED_EDGE('',*,*,#14714,.F.) ;
#18856 = ORIENTED_EDGE('',*,*,#14715,.T.) ;
#18857 = ORIENTED_EDGE('',*,*,#14716,.F.) ;
#18858 = ORIENTED_EDGE('',*,*,#14715,.F.) ;
#18859 = ORIENTED_EDGE('',*,*,#14717,.T.) ;
#18860 = ORIENTED_EDGE('',*,*,#14718,.T.) ;
#18861 = ORIENTED_EDGE('',*,*,#14719,.F.) ;
#18862 = ORIENTED_EDGE('',*,*,#14718,.F.) ;
#18863 = ORIENTED_EDGE('',*,*,#14565,.T.) ;
#18864 = ORIENTED_EDGE('',*,*,#14593,.T.) ;
#18865 = ORIENTED_EDGE('',*,*,#14617,.T.) ;
#18866 = ORIENTED_EDGE('',*,*,#14605,.T.) ;
#18867 = ORIENTED_EDGE('',*,*,#14598,.T.) ;
#18868 = ORIENTED_EDGE('',*,*,#14589,.T.) ;
#18869 = ORIENTED_EDGE('',*,*,#14594,.T.) ;
#18870 = ORIENTED_EDGE('',*,*,#14586,.T.) ;
#18871 = ORIENTED_EDGE('',*,*,#14572,.T.) ;
#18872 = ORIENTED_EDGE('',*,*,#14714,.T.) ;
#18873 = ORIENTED_EDGE('',*,*,#14587,.T.) ;
#18874 = ORIENTED_EDGE('',*,*,#14719,.T.) ;
#18875 = ORIENTED_EDGE('',*,*,#14720,.F.) ;
#18876 = ORIENTED_EDGE('',*,*,#14721,.T.) ;
#18877 = ORIENTED_EDGE('',*,*,#14717,.F.) ;
#18878 = ORIENTED_EDGE('',*,*,#14721,.F.) ;
#18879 = ORIENTED_EDGE('',*,*,#14634,.T.) ;
#18880 = ORIENTED_EDGE('',*,*,#14628,.T.) ;
#18881 = ORIENTED_EDGE('',*,*,#14637,.T.) ;
#18882 = ORIENTED_EDGE('',*,*,#14640,.T.) ;
#18883 = ORIENTED_EDGE('',*,*,#14658,.T.) ;
#18884 = ORIENTED_EDGE('',*,*,#14652,.T.) ;
#18885 = ORIENTED_EDGE('',*,*,#14661,.T.) ;
#18886 = ORIENTED_EDGE('',*,*,#14664,.T.) ;
#18887 = ORIENTED_EDGE('',*,*,#14682,.T.) ;
#18888 = ORIENTED_EDGE('',*,*,#14676,.T.) ;
#18889 = ORIENTED_EDGE('',*,*,#14685,.T.) ;
#18890 = ORIENTED_EDGE('',*,*,#14688,.T.) ;
#18891 = ORIENTED_EDGE('',*,*,#14706,.T.) ;
#18892 = ORIENTED_EDGE('',*,*,#14700,.T.) ;
#18893 = ORIENTED_EDGE('',*,*,#14709,.T.) ;
#18894 = ORIENTED_EDGE('',*,*,#14712,.T.) ;
#18895 = ORIENTED_EDGE('',*,*,#14716,.T.) ;
#18896 = ORIENTED_EDGE('',*,*,#14722,.T.) ;
#18897 = ORIENTED_EDGE('',*,*,#14723,.F.) ;
#18898 = ORIENTED_EDGE('',*,*,#14722,.F.) ;
#18899 = ORIENTED_EDGE('',*,*,#14632,.T.) ;
#18900 = ORIENTED_EDGE('',*,*,#14622,.T.) ;
#18901 = ORIENTED_EDGE('',*,*,#14618,.T.) ;
#18902 = ORIENTED_EDGE('',*,*,#14625,.T.) ;
#18903 = ORIENTED_EDGE('',*,*,#14656,.T.) ;
#18904 = ORIENTED_EDGE('',*,*,#14646,.T.) ;
#18905 = ORIENTED_EDGE('',*,*,#14642,.T.) ;
#18906 = ORIENTED_EDGE('',*,*,#14649,.T.) ;
#18907 = ORIENTED_EDGE('',*,*,#14680,.T.) ;
#18908 = ORIENTED_EDGE('',*,*,#14670,.T.) ;
#18909 = ORIENTED_EDGE('',*,*,#14666,.T.) ;
#18910 = ORIENTED_EDGE('',*,*,#14673,.T.) ;
#18911 = ORIENTED_EDGE('',*,*,#14704,.T.) ;
#18912 = ORIENTED_EDGE('',*,*,#14694,.T.) ;
#18913 = ORIENTED_EDGE('',*,*,#14690,.T.) ;
#18914 = ORIENTED_EDGE('',*,*,#14697,.T.) ;
#18915 = ORIENTED_EDGE('',*,*,#14723,.T.) ;
#18916 = ORIENTED_EDGE('',*,*,#14720,.T.) ;
#18917 = ORIENTED_EDGE('',*,*,#14724,.F.) ;
#18918 = ORIENTED_EDGE('',*,*,#14725,.F.) ;
#18919 = ORIENTED_EDGE('',*,*,#14726,.F.) ;
#18920 = ORIENTED_EDGE('',*,*,#14727,.F.) ;
#18921 = ORIENTED_EDGE('',*,*,#14728,.F.) ;
#18922 = ORIENTED_EDGE('',*,*,#14727,.T.) ;
#18923 = ORIENTED_EDGE('',*,*,#14729,.F.) ;
#18924 = ORIENTED_EDGE('',*,*,#14730,.T.) ;
#18925 = ORIENTED_EDGE('',*,*,#14731,.F.) ;
#18926 = ORIENTED_EDGE('',*,*,#14732,.T.) ;
#18927 = ORIENTED_EDGE('',*,*,#14733,.F.) ;
#18928 = ORIENTED_EDGE('',*,*,#14725,.T.) ;
#18929 = ORIENTED_EDGE('',*,*,#14731,.T.) ;
#18930 = ORIENTED_EDGE('',*,*,#14724,.T.) ;
#18931 = ORIENTED_EDGE('',*,*,#14728,.T.) ;
#18932 = ORIENTED_EDGE('',*,*,#14734,.F.) ;
#18933 = ORIENTED_EDGE('',*,*,#14735,.F.) ;
#18934 = ORIENTED_EDGE('',*,*,#14736,.F.) ;
#18935 = ORIENTED_EDGE('',*,*,#14737,.T.) ;
#18936 = ORIENTED_EDGE('',*,*,#14738,.F.) ;
#18937 = ORIENTED_EDGE('',*,*,#14729,.T.) ;
#18938 = ORIENTED_EDGE('',*,*,#14726,.T.) ;
#18939 = ORIENTED_EDGE('',*,*,#14733,.T.) ;
#18940 = ORIENTED_EDGE('',*,*,#14739,.F.) ;
#18941 = ORIENTED_EDGE('',*,*,#14740,.F.) ;
#18942 = ORIENTED_EDGE('',*,*,#14741,.F.) ;
#18943 = ORIENTED_EDGE('',*,*,#14742,.T.) ;
#18944 = ORIENTED_EDGE('',*,*,#14743,.F.) ;
#18945 = ORIENTED_EDGE('',*,*,#14744,.T.) ;
#18946 = ORIENTED_EDGE('',*,*,#14736,.T.) ;
#18947 = ORIENTED_EDGE('',*,*,#14745,.T.) ;
#18948 = ORIENTED_EDGE('',*,*,#14741,.T.) ;
#18949 = ORIENTED_EDGE('',*,*,#14735,.T.) ;
#18950 = ORIENTED_EDGE('',*,*,#14746,.F.) ;
#18951 = ORIENTED_EDGE('',*,*,#14742,.F.) ;
#18952 = ORIENTED_EDGE('',*,*,#14745,.F.) ;
#18953 = ORIENTED_EDGE('',*,*,#14740,.T.) ;
#18954 = ORIENTED_EDGE('',*,*,#14747,.F.) ;
#18955 = ORIENTED_EDGE('',*,*,#14737,.F.) ;
#18956 = ORIENTED_EDGE('',*,*,#14744,.F.) ;
#18957 = ORIENTED_EDGE('',*,*,#14748,.F.) ;
#18958 = ORIENTED_EDGE('',*,*,#14749,.T.) ;
#18959 = ORIENTED_EDGE('',*,*,#14750,.F.) ;
#18960 = ORIENTED_EDGE('',*,*,#14749,.F.) ;
#18961 = ORIENTED_EDGE('',*,*,#14751,.T.) ;
#18962 = ORIENTED_EDGE('',*,*,#14748,.T.) ;
#18963 = ORIENTED_EDGE('',*,*,#14752,.F.) ;
#18964 = ORIENTED_EDGE('',*,*,#14753,.T.) ;
#18965 = ORIENTED_EDGE('',*,*,#14751,.F.) ;
#18966 = ORIENTED_EDGE('',*,*,#14753,.F.) ;
#18967 = ORIENTED_EDGE('',*,*,#14750,.T.) ;
#18968 = ORIENTED_EDGE('',*,*,#14752,.T.) ;
#18969 = ORIENTED_EDGE('',*,*,#14738,.T.) ;
#18970 = ORIENTED_EDGE('',*,*,#14747,.T.) ;
#18971 = ORIENTED_EDGE('',*,*,#14739,.T.) ;
#18972 = ORIENTED_EDGE('',*,*,#14732,.F.) ;
#18973 = ORIENTED_EDGE('',*,*,#14730,.F.) ;
#18974 = ORIENTED_EDGE('',*,*,#14743,.T.) ;
#18975 = ORIENTED_EDGE('',*,*,#14746,.T.) ;
#18976 = ORIENTED_EDGE('',*,*,#14734,.T.) ;
#18977 = ORIENTED_EDGE('',*,*,#14754,.F.) ;
#18978 = ORIENTED_EDGE('',*,*,#14755,.T.) ;
#18979 = ORIENTED_EDGE('',*,*,#14756,.T.) ;
#18980 = ORIENTED_EDGE('',*,*,#14757,.T.) ;
#18981 = ORIENTED_EDGE('',*,*,#14758,.F.) ;
#18982 = ORIENTED_EDGE('',*,*,#14759,.T.) ;
#18983 = ORIENTED_EDGE('',*,*,#14760,.T.) ;
#18984 = ORIENTED_EDGE('',*,*,#14761,.T.) ;
#18985 = ORIENTED_EDGE('',*,*,#14762,.T.) ;
#18986 = ORIENTED_EDGE('',*,*,#14760,.F.) ;
#18987 = ORIENTED_EDGE('',*,*,#14763,.F.) ;
#18988 = ORIENTED_EDGE('',*,*,#14756,.F.) ;
#18989 = ORIENTED_EDGE('',*,*,#14764,.T.) ;
#18990 = ORIENTED_EDGE('',*,*,#14757,.F.) ;
#18991 = ORIENTED_EDGE('',*,*,#14763,.T.) ;
#18992 = ORIENTED_EDGE('',*,*,#14759,.F.) ;
#18993 = ORIENTED_EDGE('',*,*,#14754,.T.) ;
#18994 = ORIENTED_EDGE('',*,*,#14764,.F.) ;
#18995 = ORIENTED_EDGE('',*,*,#14758,.T.) ;
#18996 = ORIENTED_EDGE('',*,*,#14765,.F.) ;
#18997 = ORIENTED_EDGE('',*,*,#14765,.T.) ;
#18998 = ORIENTED_EDGE('',*,*,#14761,.F.) ;
#18999 = ORIENTED_EDGE('',*,*,#14762,.F.) ;
#19000 = ORIENTED_EDGE('',*,*,#14755,.F.) ;
#19001 = ORIENTED_EDGE('',*,*,#14766,.F.) ;
#19002 = ORIENTED_EDGE('',*,*,#14767,.F.) ;
#19003 = ORIENTED_EDGE('',*,*,#14768,.F.) ;
#19004 = ORIENTED_EDGE('',*,*,#14769,.F.) ;
#19005 = ORIENTED_EDGE('',*,*,#14770,.F.) ;
#19006 = ORIENTED_EDGE('',*,*,#14771,.F.) ;
#19007 = ORIENTED_EDGE('',*,*,#14772,.F.) ;
#19008 = ORIENTED_EDGE('',*,*,#14773,.F.) ;
#19009 = ORIENTED_EDGE('',*,*,#14774,.F.) ;
#19010 = ORIENTED_EDGE('',*,*,#14775,.F.) ;
#19011 = ORIENTED_EDGE('',*,*,#14776,.F.) ;
#19012 = ORIENTED_EDGE('',*,*,#14777,.F.) ;
#19013 = ORIENTED_EDGE('',*,*,#14778,.F.) ;
#19014 = ORIENTED_EDGE('',*,*,#14779,.F.) ;
#19015 = ORIENTED_EDGE('',*,*,#14780,.F.) ;
#19016 = ORIENTED_EDGE('',*,*,#14781,.F.) ;
#19017 = ORIENTED_EDGE('',*,*,#14782,.F.) ;
#19018 = ORIENTED_EDGE('',*,*,#14783,.F.) ;
#19019 = ORIENTED_EDGE('',*,*,#14784,.F.) ;
#19020 = ORIENTED_EDGE('',*,*,#14785,.F.) ;
#19021 = ORIENTED_EDGE('',*,*,#14786,.F.) ;
#19022 = ORIENTED_EDGE('',*,*,#14787,.F.) ;
#19023 = ORIENTED_EDGE('',*,*,#14788,.F.) ;
#19024 = ORIENTED_EDGE('',*,*,#14789,.F.) ;
#19025 = ORIENTED_EDGE('',*,*,#14790,.F.) ;
#19026 = ORIENTED_EDGE('',*,*,#14791,.F.) ;
#19027 = ORIENTED_EDGE('',*,*,#14792,.F.) ;
#19028 = ORIENTED_EDGE('',*,*,#14793,.F.) ;
#19029 = ORIENTED_EDGE('',*,*,#14794,.F.) ;
#19030 = ORIENTED_EDGE('',*,*,#14795,.F.) ;
#19031 = ORIENTED_EDGE('',*,*,#14796,.T.) ;
#19032 = ORIENTED_EDGE('',*,*,#14797,.F.) ;
#19033 = ORIENTED_EDGE('',*,*,#14798,.F.) ;
#19034 = ORIENTED_EDGE('',*,*,#14799,.F.) ;
#19035 = ORIENTED_EDGE('',*,*,#14800,.F.) ;
#19036 = ORIENTED_EDGE('',*,*,#14801,.F.) ;
#19037 = ORIENTED_EDGE('',*,*,#14802,.F.) ;
#19038 = ORIENTED_EDGE('',*,*,#14803,.F.) ;
#19039 = ORIENTED_EDGE('',*,*,#14804,.F.) ;
#19040 = ORIENTED_EDGE('',*,*,#14805,.F.) ;
#19041 = ORIENTED_EDGE('',*,*,#14806,.F.) ;
#19042 = ORIENTED_EDGE('',*,*,#14807,.F.) ;
#19043 = ORIENTED_EDGE('',*,*,#14808,.F.) ;
#19044 = ORIENTED_EDGE('',*,*,#14809,.F.) ;
#19045 = ORIENTED_EDGE('',*,*,#14810,.F.) ;
#19046 = ORIENTED_EDGE('',*,*,#14811,.F.) ;
#19047 = ORIENTED_EDGE('',*,*,#14812,.F.) ;
#19048 = ORIENTED_EDGE('',*,*,#14813,.F.) ;
#19049 = ORIENTED_EDGE('',*,*,#14814,.F.) ;
#19050 = ORIENTED_EDGE('',*,*,#14815,.F.) ;
#19051 = ORIENTED_EDGE('',*,*,#14796,.F.) ;
#19052 = ORIENTED_EDGE('',*,*,#14816,.F.) ;
#19053 = ORIENTED_EDGE('',*,*,#14817,.F.) ;
#19054 = ORIENTED_EDGE('',*,*,#14818,.F.) ;
#19055 = ORIENTED_EDGE('',*,*,#14792,.T.) ;
#19056 = ORIENTED_EDGE('',*,*,#14819,.F.) ;
#19057 = ORIENTED_EDGE('',*,*,#14790,.T.) ;
#19058 = ORIENTED_EDGE('',*,*,#14820,.F.) ;
#19059 = ORIENTED_EDGE('',*,*,#14821,.T.) ;
#19060 = ORIENTED_EDGE('',*,*,#14822,.F.) ;
#19061 = ORIENTED_EDGE('',*,*,#14817,.T.) ;
#19062 = ORIENTED_EDGE('',*,*,#14823,.F.) ;
#19063 = ORIENTED_EDGE('',*,*,#14824,.T.) ;
#19064 = ORIENTED_EDGE('',*,*,#14825,.F.) ;
#19065 = ORIENTED_EDGE('',*,*,#14810,.T.) ;
#19066 = ORIENTED_EDGE('',*,*,#14826,.F.) ;
#19067 = ORIENTED_EDGE('',*,*,#14827,.T.) ;
#19068 = ORIENTED_EDGE('',*,*,#14828,.F.) ;
#19069 = ORIENTED_EDGE('',*,*,#14788,.T.) ;
#19070 = ORIENTED_EDGE('',*,*,#14829,.F.) ;
#19071 = ORIENTED_EDGE('',*,*,#14830,.T.) ;
#19072 = ORIENTED_EDGE('',*,*,#14831,.F.) ;
#19073 = ORIENTED_EDGE('',*,*,#14806,.T.) ;
#19074 = ORIENTED_EDGE('',*,*,#14832,.F.) ;
#19075 = ORIENTED_EDGE('',*,*,#14833,.F.) ;
#19076 = ORIENTED_EDGE('',*,*,#14834,.F.) ;
#19077 = ORIENTED_EDGE('',*,*,#14784,.T.) ;
#19078 = ORIENTED_EDGE('',*,*,#14835,.F.) ;
#19079 = ORIENTED_EDGE('',*,*,#14836,.T.) ;
#19080 = ORIENTED_EDGE('',*,*,#14837,.F.) ;
#19081 = ORIENTED_EDGE('',*,*,#14802,.T.) ;
#19082 = ORIENTED_EDGE('',*,*,#14838,.F.) ;
#19083 = ORIENTED_EDGE('',*,*,#14839,.F.) ;
#19084 = ORIENTED_EDGE('',*,*,#14840,.F.) ;
#19085 = ORIENTED_EDGE('',*,*,#14780,.T.) ;
#19086 = ORIENTED_EDGE('',*,*,#14841,.F.) ;
#19087 = ORIENTED_EDGE('',*,*,#14842,.T.) ;
#19088 = ORIENTED_EDGE('',*,*,#14843,.F.) ;
#19089 = ORIENTED_EDGE('',*,*,#14798,.T.) ;
#19090 = ORIENTED_EDGE('',*,*,#14844,.F.) ;
#19091 = ORIENTED_EDGE('',*,*,#14845,.F.) ;
#19092 = ORIENTED_EDGE('',*,*,#14846,.F.) ;
#19093 = ORIENTED_EDGE('',*,*,#14776,.T.) ;
#19094 = ORIENTED_EDGE('',*,*,#14847,.F.) ;
#19095 = ORIENTED_EDGE('',*,*,#14848,.T.) ;
#19096 = ORIENTED_EDGE('',*,*,#14849,.F.) ;
#19097 = ORIENTED_EDGE('',*,*,#14772,.T.) ;
#19098 = ORIENTED_EDGE('',*,*,#14850,.F.) ;
#19099 = ORIENTED_EDGE('',*,*,#14851,.T.) ;
#19100 = ORIENTED_EDGE('',*,*,#14852,.F.) ;
#19101 = ORIENTED_EDGE('',*,*,#14825,.T.) ;
#19102 = ORIENTED_EDGE('',*,*,#14853,.T.) ;
#19103 = ORIENTED_EDGE('',*,*,#14854,.T.) ;
#19104 = ORIENTED_EDGE('',*,*,#14855,.T.) ;
#19105 = ORIENTED_EDGE('',*,*,#14856,.T.) ;
#19106 = ORIENTED_EDGE('',*,*,#14857,.T.) ;
#19107 = ORIENTED_EDGE('',*,*,#14858,.T.) ;
#19108 = ORIENTED_EDGE('',*,*,#14859,.T.) ;
#19109 = ORIENTED_EDGE('',*,*,#14860,.T.) ;
#19110 = ORIENTED_EDGE('',*,*,#14861,.T.) ;
#19111 = ORIENTED_EDGE('',*,*,#14862,.T.) ;
#19112 = ORIENTED_EDGE('',*,*,#14863,.T.) ;
#19113 = ORIENTED_EDGE('',*,*,#14864,.T.) ;
#19114 = ORIENTED_EDGE('',*,*,#14865,.T.) ;
#19115 = ORIENTED_EDGE('',*,*,#14866,.T.) ;
#19116 = ORIENTED_EDGE('',*,*,#14867,.T.) ;
#19117 = ORIENTED_EDGE('',*,*,#14868,.T.) ;
#19118 = ORIENTED_EDGE('',*,*,#14869,.T.) ;
#19119 = ORIENTED_EDGE('',*,*,#14870,.T.) ;
#19120 = ORIENTED_EDGE('',*,*,#14871,.T.) ;
#19121 = ORIENTED_EDGE('',*,*,#14872,.T.) ;
#19122 = ORIENTED_EDGE('',*,*,#14873,.T.) ;
#19123 = ORIENTED_EDGE('',*,*,#14874,.T.) ;
#19124 = ORIENTED_EDGE('',*,*,#14875,.T.) ;
#19125 = ORIENTED_EDGE('',*,*,#14876,.T.) ;
#19126 = ORIENTED_EDGE('',*,*,#14877,.T.) ;
#19127 = ORIENTED_EDGE('',*,*,#14878,.T.) ;
#19128 = ORIENTED_EDGE('',*,*,#14879,.T.) ;
#19129 = ORIENTED_EDGE('',*,*,#14880,.T.) ;
#19130 = ORIENTED_EDGE('',*,*,#14881,.T.) ;
#19131 = ORIENTED_EDGE('',*,*,#14882,.T.) ;
#19132 = ORIENTED_EDGE('',*,*,#14883,.T.) ;
#19133 = ORIENTED_EDGE('',*,*,#14884,.T.) ;
#19134 = ORIENTED_EDGE('',*,*,#14885,.T.) ;
#19135 = ORIENTED_EDGE('',*,*,#14886,.T.) ;
#19136 = ORIENTED_EDGE('',*,*,#14887,.T.) ;
#19137 = ORIENTED_EDGE('',*,*,#14888,.T.) ;
#19138 = ORIENTED_EDGE('',*,*,#14889,.T.) ;
#19139 = ORIENTED_EDGE('',*,*,#14890,.T.) ;
#19140 = ORIENTED_EDGE('',*,*,#14891,.T.) ;
#19141 = ORIENTED_EDGE('',*,*,#14892,.T.) ;
#19142 = ORIENTED_EDGE('',*,*,#14893,.T.) ;
#19143 = ORIENTED_EDGE('',*,*,#14894,.T.) ;
#19144 = ORIENTED_EDGE('',*,*,#14895,.T.) ;
#19145 = ORIENTED_EDGE('',*,*,#14896,.T.) ;
#19146 = ORIENTED_EDGE('',*,*,#14897,.T.) ;
#19147 = ORIENTED_EDGE('',*,*,#14898,.T.) ;
#19148 = ORIENTED_EDGE('',*,*,#14899,.T.) ;
#19149 = ORIENTED_EDGE('',*,*,#14900,.T.) ;
#19150 = ORIENTED_EDGE('',*,*,#14901,.T.) ;
#19151 = ORIENTED_EDGE('',*,*,#14902,.T.) ;
#19152 = ORIENTED_EDGE('',*,*,#14903,.T.) ;
#19153 = ORIENTED_EDGE('',*,*,#14904,.T.) ;
#19154 = ORIENTED_EDGE('',*,*,#14905,.T.) ;
#19155 = ORIENTED_EDGE('',*,*,#14906,.T.) ;
#19156 = ORIENTED_EDGE('',*,*,#14907,.T.) ;
#19157 = ORIENTED_EDGE('',*,*,#14908,.T.) ;
#19158 = ORIENTED_EDGE('',*,*,#14909,.T.) ;
#19159 = ORIENTED_EDGE('',*,*,#14910,.T.) ;
#19160 = ORIENTED_EDGE('',*,*,#14911,.T.) ;
#19161 = ORIENTED_EDGE('',*,*,#14912,.T.) ;
#19162 = ORIENTED_EDGE('',*,*,#14913,.T.) ;
#19163 = ORIENTED_EDGE('',*,*,#14914,.T.) ;
#19164 = ORIENTED_EDGE('',*,*,#14915,.T.) ;
#19165 = ORIENTED_EDGE('',*,*,#14916,.T.) ;
#19166 = ORIENTED_EDGE('',*,*,#14917,.T.) ;
#19167 = ORIENTED_EDGE('',*,*,#14918,.T.) ;
#19168 = ORIENTED_EDGE('',*,*,#14816,.T.) ;
#19169 = ORIENTED_EDGE('',*,*,#14795,.T.) ;
#19170 = ORIENTED_EDGE('',*,*,#14919,.T.) ;
#19171 = ORIENTED_EDGE('',*,*,#14920,.T.) ;
#19172 = ORIENTED_EDGE('',*,*,#14921,.T.) ;
#19173 = ORIENTED_EDGE('',*,*,#14922,.T.) ;
#19174 = ORIENTED_EDGE('',*,*,#14923,.T.) ;
#19175 = ORIENTED_EDGE('',*,*,#14924,.T.) ;
#19176 = ORIENTED_EDGE('',*,*,#14925,.T.) ;
#19177 = ORIENTED_EDGE('',*,*,#14926,.T.) ;
#19178 = ORIENTED_EDGE('',*,*,#14927,.T.) ;
#19179 = ORIENTED_EDGE('',*,*,#14928,.T.) ;
#19180 = ORIENTED_EDGE('',*,*,#14929,.T.) ;
#19181 = ORIENTED_EDGE('',*,*,#14930,.T.) ;
#19182 = ORIENTED_EDGE('',*,*,#14931,.T.) ;
#19183 = ORIENTED_EDGE('',*,*,#14932,.T.) ;
#19184 = ORIENTED_EDGE('',*,*,#14933,.T.) ;
#19185 = ORIENTED_EDGE('',*,*,#14934,.T.) ;
#19186 = ORIENTED_EDGE('',*,*,#14820,.T.) ;
#19187 = ORIENTED_EDGE('',*,*,#14793,.T.) ;
#19188 = ORIENTED_EDGE('',*,*,#14818,.T.) ;
#19189 = ORIENTED_EDGE('',*,*,#14828,.T.) ;
#19190 = ORIENTED_EDGE('',*,*,#14935,.T.) ;
#19191 = ORIENTED_EDGE('',*,*,#14811,.T.) ;
#19192 = ORIENTED_EDGE('',*,*,#14834,.T.) ;
#19193 = ORIENTED_EDGE('',*,*,#14936,.T.) ;
#19194 = ORIENTED_EDGE('',*,*,#14937,.T.) ;
#19195 = ORIENTED_EDGE('',*,*,#14807,.T.) ;
#19196 = ORIENTED_EDGE('',*,*,#14840,.T.) ;
#19197 = ORIENTED_EDGE('',*,*,#14938,.T.) ;
#19198 = ORIENTED_EDGE('',*,*,#14939,.T.) ;
#19199 = ORIENTED_EDGE('',*,*,#14803,.T.) ;
#19200 = ORIENTED_EDGE('',*,*,#14846,.T.) ;
#19201 = ORIENTED_EDGE('',*,*,#14940,.T.) ;
#19202 = ORIENTED_EDGE('',*,*,#14799,.T.) ;
#19203 = ORIENTED_EDGE('',*,*,#14785,.T.) ;
#19204 = ORIENTED_EDGE('',*,*,#14837,.T.) ;
#19205 = ORIENTED_EDGE('',*,*,#14941,.T.) ;
#19206 = ORIENTED_EDGE('',*,*,#14942,.T.) ;
#19207 = ORIENTED_EDGE('',*,*,#14781,.T.) ;
#19208 = ORIENTED_EDGE('',*,*,#14843,.T.) ;
#19209 = ORIENTED_EDGE('',*,*,#14943,.T.) ;
#19210 = ORIENTED_EDGE('',*,*,#14944,.T.) ;
#19211 = ORIENTED_EDGE('',*,*,#14777,.T.) ;
#19212 = ORIENTED_EDGE('',*,*,#14849,.T.) ;
#19213 = ORIENTED_EDGE('',*,*,#14945,.T.) ;
#19214 = ORIENTED_EDGE('',*,*,#14946,.T.) ;
#19215 = ORIENTED_EDGE('',*,*,#14773,.T.) ;
#19216 = ORIENTED_EDGE('',*,*,#14852,.T.) ;
#19217 = ORIENTED_EDGE('',*,*,#14947,.T.) ;
#19218 = ORIENTED_EDGE('',*,*,#14948,.T.) ;
#19219 = ORIENTED_EDGE('',*,*,#14789,.T.) ;
#19220 = ORIENTED_EDGE('',*,*,#14831,.T.) ;
#19221 = ORIENTED_EDGE('',*,*,#14949,.T.) ;
#19222 = ORIENTED_EDGE('',*,*,#14950,.T.) ;
#19223 = ORIENTED_EDGE('',*,*,#14951,.T.) ;
#19224 = ORIENTED_EDGE('',*,*,#14952,.T.) ;
#19225 = ORIENTED_EDGE('',*,*,#14953,.T.) ;
#19226 = ORIENTED_EDGE('',*,*,#14954,.T.) ;
#19227 = ORIENTED_EDGE('',*,*,#14955,.T.) ;
#19228 = ORIENTED_EDGE('',*,*,#14956,.T.) ;
#19229 = ORIENTED_EDGE('',*,*,#14957,.T.) ;
#19230 = ORIENTED_EDGE('',*,*,#14958,.T.) ;
#19231 = ORIENTED_EDGE('',*,*,#14959,.T.) ;
#19232 = ORIENTED_EDGE('',*,*,#14960,.T.) ;
#19233 = ORIENTED_EDGE('',*,*,#14961,.T.) ;
#19234 = ORIENTED_EDGE('',*,*,#14962,.T.) ;
#19235 = ORIENTED_EDGE('',*,*,#14963,.T.) ;
#19236 = ORIENTED_EDGE('',*,*,#14964,.T.) ;
#19237 = ORIENTED_EDGE('',*,*,#14965,.T.) ;
#19238 = ORIENTED_EDGE('',*,*,#14966,.T.) ;
#19239 = ORIENTED_EDGE('',*,*,#14967,.T.) ;
#19240 = ORIENTED_EDGE('',*,*,#14968,.T.) ;
#19241 = ORIENTED_EDGE('',*,*,#14969,.T.) ;
#19242 = ORIENTED_EDGE('',*,*,#14970,.T.) ;
#19243 = ORIENTED_EDGE('',*,*,#14971,.T.) ;
#19244 = ORIENTED_EDGE('',*,*,#14972,.T.) ;
#19245 = ORIENTED_EDGE('',*,*,#14973,.T.) ;
#19246 = ORIENTED_EDGE('',*,*,#14974,.T.) ;
#19247 = ORIENTED_EDGE('',*,*,#14975,.T.) ;
#19248 = ORIENTED_EDGE('',*,*,#14976,.T.) ;
#19249 = ORIENTED_EDGE('',*,*,#14977,.T.) ;
#19250 = ORIENTED_EDGE('',*,*,#14978,.T.) ;
#19251 = ORIENTED_EDGE('',*,*,#14979,.T.) ;
#19252 = ORIENTED_EDGE('',*,*,#14980,.T.) ;
#19253 = ORIENTED_EDGE('',*,*,#14981,.T.) ;
#19254 = ORIENTED_EDGE('',*,*,#14982,.T.) ;
#19255 = ORIENTED_EDGE('',*,*,#14983,.T.) ;
#19256 = ORIENTED_EDGE('',*,*,#14984,.T.) ;
#19257 = ORIENTED_EDGE('',*,*,#14985,.T.) ;
#19258 = ORIENTED_EDGE('',*,*,#14986,.T.) ;
#19259 = ORIENTED_EDGE('',*,*,#14987,.T.) ;
#19260 = ORIENTED_EDGE('',*,*,#14988,.T.) ;
#19261 = ORIENTED_EDGE('',*,*,#14989,.T.) ;
#19262 = ORIENTED_EDGE('',*,*,#14990,.T.) ;
#19263 = ORIENTED_EDGE('',*,*,#14991,.T.) ;
#19264 = ORIENTED_EDGE('',*,*,#14992,.T.) ;
#19265 = ORIENTED_EDGE('',*,*,#14993,.T.) ;
#19266 = ORIENTED_EDGE('',*,*,#14994,.T.) ;
#19267 = ORIENTED_EDGE('',*,*,#14995,.T.) ;
#19268 = ORIENTED_EDGE('',*,*,#14996,.T.) ;
#19269 = ORIENTED_EDGE('',*,*,#14997,.T.) ;
#19270 = ORIENTED_EDGE('',*,*,#14998,.T.) ;
#19271 = ORIENTED_EDGE('',*,*,#14999,.T.) ;
#19272 = ORIENTED_EDGE('',*,*,#15000,.T.) ;
#19273 = ORIENTED_EDGE('',*,*,#15001,.T.) ;
#19274 = ORIENTED_EDGE('',*,*,#15002,.T.) ;
#19275 = ORIENTED_EDGE('',*,*,#15003,.T.) ;
#19276 = ORIENTED_EDGE('',*,*,#15004,.T.) ;
#19277 = ORIENTED_EDGE('',*,*,#15005,.T.) ;
#19278 = ORIENTED_EDGE('',*,*,#15006,.T.) ;
#19279 = ORIENTED_EDGE('',*,*,#15007,.T.) ;
#19280 = ORIENTED_EDGE('',*,*,#15008,.T.) ;
#19281 = ORIENTED_EDGE('',*,*,#15009,.T.) ;
#19282 = ORIENTED_EDGE('',*,*,#15010,.T.) ;
#19283 = ORIENTED_EDGE('',*,*,#15011,.T.) ;
#19284 = ORIENTED_EDGE('',*,*,#15012,.T.) ;
#19285 = ORIENTED_EDGE('',*,*,#15013,.T.) ;
#19286 = ORIENTED_EDGE('',*,*,#15014,.T.) ;
#19287 = ORIENTED_EDGE('',*,*,#15015,.T.) ;
#19288 = ORIENTED_EDGE('',*,*,#15016,.T.) ;
#19289 = ORIENTED_EDGE('',*,*,#15017,.T.) ;
#19290 = ORIENTED_EDGE('',*,*,#15018,.T.) ;
#19291 = ORIENTED_EDGE('',*,*,#15019,.T.) ;
#19292 = ORIENTED_EDGE('',*,*,#15020,.T.) ;
#19293 = ORIENTED_EDGE('',*,*,#15021,.T.) ;
#19294 = ORIENTED_EDGE('',*,*,#15022,.T.) ;
#19295 = ORIENTED_EDGE('',*,*,#15023,.T.) ;
#19296 = ORIENTED_EDGE('',*,*,#15024,.T.) ;
#19297 = ORIENTED_EDGE('',*,*,#15025,.T.) ;
#19298 = ORIENTED_EDGE('',*,*,#15026,.T.) ;
#19299 = ORIENTED_EDGE('',*,*,#15027,.T.) ;
#19300 = ORIENTED_EDGE('',*,*,#15028,.T.) ;
#19301 = ORIENTED_EDGE('',*,*,#15029,.T.) ;
#19302 = ORIENTED_EDGE('',*,*,#15030,.T.) ;
#19303 = ORIENTED_EDGE('',*,*,#15031,.T.) ;
#19304 = ORIENTED_EDGE('',*,*,#15032,.T.) ;
#19305 = ORIENTED_EDGE('',*,*,#15033,.T.) ;
#19306 = ORIENTED_EDGE('',*,*,#15034,.T.) ;
#19307 = ORIENTED_EDGE('',*,*,#15035,.T.) ;
#19308 = ORIENTED_EDGE('',*,*,#15036,.T.) ;
#19309 = ORIENTED_EDGE('',*,*,#15037,.T.) ;
#19310 = ORIENTED_EDGE('',*,*,#15038,.T.) ;
#19311 = ORIENTED_EDGE('',*,*,#15039,.T.) ;
#19312 = ORIENTED_EDGE('',*,*,#15040,.T.) ;
#19313 = ORIENTED_EDGE('',*,*,#15041,.T.) ;
#19314 = ORIENTED_EDGE('',*,*,#15042,.T.) ;
#19315 = ORIENTED_EDGE('',*,*,#15043,.T.) ;
#19316 = ORIENTED_EDGE('',*,*,#15044,.T.) ;
#19317 = ORIENTED_EDGE('',*,*,#15045,.T.) ;
#19318 = ORIENTED_EDGE('',*,*,#15046,.T.) ;
#19319 = ORIENTED_EDGE('',*,*,#15047,.T.) ;
#19320 = ORIENTED_EDGE('',*,*,#15048,.T.) ;
#19321 = ORIENTED_EDGE('',*,*,#15049,.T.) ;
#19322 = ORIENTED_EDGE('',*,*,#15050,.T.) ;
#19323 = ORIENTED_EDGE('',*,*,#15051,.T.) ;
#19324 = ORIENTED_EDGE('',*,*,#15052,.T.) ;
#19325 = ORIENTED_EDGE('',*,*,#15053,.T.) ;
#19326 = ORIENTED_EDGE('',*,*,#15054,.T.) ;
#19327 = ORIENTED_EDGE('',*,*,#15055,.T.) ;
#19328 = ORIENTED_EDGE('',*,*,#15056,.T.) ;
#19329 = ORIENTED_EDGE('',*,*,#15057,.T.) ;
#19330 = ORIENTED_EDGE('',*,*,#15058,.T.) ;
#19331 = ORIENTED_EDGE('',*,*,#15059,.T.) ;
#19332 = ORIENTED_EDGE('',*,*,#15060,.T.) ;
#19333 = ORIENTED_EDGE('',*,*,#15061,.T.) ;
#19334 = ORIENTED_EDGE('',*,*,#15062,.T.) ;
#19335 = ORIENTED_EDGE('',*,*,#15063,.T.) ;
#19336 = ORIENTED_EDGE('',*,*,#15064,.T.) ;
#19337 = ORIENTED_EDGE('',*,*,#15065,.T.) ;
#19338 = ORIENTED_EDGE('',*,*,#15066,.T.) ;
#19339 = ORIENTED_EDGE('',*,*,#15067,.T.) ;
#19340 = ORIENTED_EDGE('',*,*,#15068,.T.) ;
#19341 = ORIENTED_EDGE('',*,*,#15069,.T.) ;
#19342 = ORIENTED_EDGE('',*,*,#15070,.T.) ;
#19343 = ORIENTED_EDGE('',*,*,#15071,.T.) ;
#19344 = ORIENTED_EDGE('',*,*,#15072,.T.) ;
#19345 = ORIENTED_EDGE('',*,*,#15073,.T.) ;
#19346 = ORIENTED_EDGE('',*,*,#15074,.T.) ;
#19347 = ORIENTED_EDGE('',*,*,#15075,.T.) ;
#19348 = ORIENTED_EDGE('',*,*,#15076,.T.) ;
#19349 = ORIENTED_EDGE('',*,*,#15077,.T.) ;
#19350 = ORIENTED_EDGE('',*,*,#15078,.T.) ;
#19351 = ORIENTED_EDGE('',*,*,#15079,.T.) ;
#19352 = ORIENTED_EDGE('',*,*,#15080,.T.) ;
#19353 = ORIENTED_EDGE('',*,*,#15081,.T.) ;
#19354 = ORIENTED_EDGE('',*,*,#15082,.T.) ;
#19355 = ORIENTED_EDGE('',*,*,#15083,.T.) ;
#19356 = ORIENTED_EDGE('',*,*,#15084,.T.) ;
#19357 = ORIENTED_EDGE('',*,*,#15085,.T.) ;
#19358 = ORIENTED_EDGE('',*,*,#15086,.T.) ;
#19359 = ORIENTED_EDGE('',*,*,#15087,.T.) ;
#19360 = ORIENTED_EDGE('',*,*,#15088,.T.) ;
#19361 = ORIENTED_EDGE('',*,*,#15089,.T.) ;
#19362 = ORIENTED_EDGE('',*,*,#15090,.T.) ;
#19363 = ORIENTED_EDGE('',*,*,#15091,.T.) ;
#19364 = ORIENTED_EDGE('',*,*,#15092,.T.) ;
#19365 = ORIENTED_EDGE('',*,*,#15093,.T.) ;
#19366 = ORIENTED_EDGE('',*,*,#15094,.T.) ;
#19367 = ORIENTED_EDGE('',*,*,#15095,.T.) ;
#19368 = ORIENTED_EDGE('',*,*,#15096,.T.) ;
#19369 = ORIENTED_EDGE('',*,*,#15097,.T.) ;
#19370 = ORIENTED_EDGE('',*,*,#15098,.T.) ;
#19371 = ORIENTED_EDGE('',*,*,#15099,.T.) ;
#19372 = ORIENTED_EDGE('',*,*,#15100,.T.) ;
#19373 = ORIENTED_EDGE('',*,*,#15101,.T.) ;
#19374 = ORIENTED_EDGE('',*,*,#15102,.T.) ;
#19375 = ORIENTED_EDGE('',*,*,#15103,.T.) ;
#19376 = ORIENTED_EDGE('',*,*,#15104,.T.) ;
#19377 = ORIENTED_EDGE('',*,*,#15105,.T.) ;
#19378 = ORIENTED_EDGE('',*,*,#15106,.T.) ;
#19379 = ORIENTED_EDGE('',*,*,#15107,.T.) ;
#19380 = ORIENTED_EDGE('',*,*,#15108,.T.) ;
#19381 = ORIENTED_EDGE('',*,*,#15109,.T.) ;
#19382 = ORIENTED_EDGE('',*,*,#15110,.T.) ;
#19383 = ORIENTED_EDGE('',*,*,#15111,.T.) ;
#19384 = ORIENTED_EDGE('',*,*,#15112,.T.) ;
#19385 = ORIENTED_EDGE('',*,*,#15113,.T.) ;
#19386 = ORIENTED_EDGE('',*,*,#15114,.T.) ;
#19387 = ORIENTED_EDGE('',*,*,#15115,.T.) ;
#19388 = ORIENTED_EDGE('',*,*,#14769,.T.) ;
#19389 = ORIENTED_EDGE('',*,*,#15116,.T.) ;
#19390 = ORIENTED_EDGE('',*,*,#15117,.T.) ;
#19391 = ORIENTED_EDGE('',*,*,#15118,.T.) ;
#19392 = ORIENTED_EDGE('',*,*,#15119,.T.) ;
#19393 = ORIENTED_EDGE('',*,*,#14768,.T.) ;
#19394 = ORIENTED_EDGE('',*,*,#15120,.F.) ;
#19395 = ORIENTED_EDGE('',*,*,#15121,.T.) ;
#19396 = ORIENTED_EDGE('',*,*,#15116,.F.) ;
#19397 = ORIENTED_EDGE('',*,*,#14822,.T.) ;
#19398 = ORIENTED_EDGE('',*,*,#15122,.T.) ;
#19399 = ORIENTED_EDGE('',*,*,#15123,.T.) ;
#19400 = ORIENTED_EDGE('',*,*,#15124,.T.) ;
#19401 = ORIENTED_EDGE('',*,*,#15125,.T.) ;
#19402 = ORIENTED_EDGE('',*,*,#15126,.T.) ;
#19403 = ORIENTED_EDGE('',*,*,#15127,.T.) ;
#19404 = ORIENTED_EDGE('',*,*,#15128,.T.) ;
#19405 = ORIENTED_EDGE('',*,*,#15129,.T.) ;
#19406 = ORIENTED_EDGE('',*,*,#15130,.T.) ;
#19407 = ORIENTED_EDGE('',*,*,#15131,.T.) ;
#19408 = ORIENTED_EDGE('',*,*,#15132,.T.) ;
#19409 = ORIENTED_EDGE('',*,*,#15133,.T.) ;
#19410 = ORIENTED_EDGE('',*,*,#15134,.T.) ;
#19411 = ORIENTED_EDGE('',*,*,#15135,.T.) ;
#19412 = ORIENTED_EDGE('',*,*,#15136,.T.) ;
#19413 = ORIENTED_EDGE('',*,*,#15137,.T.) ;
#19414 = ORIENTED_EDGE('',*,*,#14797,.T.) ;
#19415 = ORIENTED_EDGE('',*,*,#14815,.T.) ;
#19416 = ORIENTED_EDGE('',*,*,#15138,.T.) ;
#19417 = ORIENTED_EDGE('',*,*,#15139,.T.) ;
#19418 = ORIENTED_EDGE('',*,*,#15140,.T.) ;
#19419 = ORIENTED_EDGE('',*,*,#15141,.T.) ;
#19420 = ORIENTED_EDGE('',*,*,#15142,.T.) ;
#19421 = ORIENTED_EDGE('',*,*,#15143,.T.) ;
#19422 = ORIENTED_EDGE('',*,*,#15144,.T.) ;
#19423 = ORIENTED_EDGE('',*,*,#15145,.T.) ;
#19424 = ORIENTED_EDGE('',*,*,#15146,.T.) ;
#19425 = ORIENTED_EDGE('',*,*,#15147,.T.) ;
#19426 = ORIENTED_EDGE('',*,*,#15148,.T.) ;
#19427 = ORIENTED_EDGE('',*,*,#15149,.T.) ;
#19428 = ORIENTED_EDGE('',*,*,#15150,.T.) ;
#19429 = ORIENTED_EDGE('',*,*,#15151,.T.) ;
#19430 = ORIENTED_EDGE('',*,*,#15152,.T.) ;
#19431 = ORIENTED_EDGE('',*,*,#15153,.T.) ;
#19432 = ORIENTED_EDGE('',*,*,#15154,.T.) ;
#19433 = ORIENTED_EDGE('',*,*,#15155,.T.) ;
#19434 = ORIENTED_EDGE('',*,*,#15156,.T.) ;
#19435 = ORIENTED_EDGE('',*,*,#15157,.T.) ;
#19436 = ORIENTED_EDGE('',*,*,#15158,.T.) ;
#19437 = ORIENTED_EDGE('',*,*,#15159,.T.) ;
#19438 = ORIENTED_EDGE('',*,*,#15160,.T.) ;
#19439 = ORIENTED_EDGE('',*,*,#15161,.T.) ;
#19440 = ORIENTED_EDGE('',*,*,#15162,.T.) ;
#19441 = ORIENTED_EDGE('',*,*,#15163,.T.) ;
#19442 = ORIENTED_EDGE('',*,*,#15164,.T.) ;
#19443 = ORIENTED_EDGE('',*,*,#15165,.T.) ;
#19444 = ORIENTED_EDGE('',*,*,#15166,.T.) ;
#19445 = ORIENTED_EDGE('',*,*,#15167,.T.) ;
#19446 = ORIENTED_EDGE('',*,*,#15168,.T.) ;
#19447 = ORIENTED_EDGE('',*,*,#15169,.T.) ;
#19448 = ORIENTED_EDGE('',*,*,#15170,.T.) ;
#19449 = ORIENTED_EDGE('',*,*,#15171,.T.) ;
#19450 = ORIENTED_EDGE('',*,*,#15172,.T.) ;
#19451 = ORIENTED_EDGE('',*,*,#15173,.T.) ;
#19452 = ORIENTED_EDGE('',*,*,#15174,.T.) ;
#19453 = ORIENTED_EDGE('',*,*,#15175,.T.) ;
#19454 = ORIENTED_EDGE('',*,*,#15176,.T.) ;
#19455 = ORIENTED_EDGE('',*,*,#15177,.T.) ;
#19456 = ORIENTED_EDGE('',*,*,#15178,.T.) ;
#19457 = ORIENTED_EDGE('',*,*,#15179,.T.) ;
#19458 = ORIENTED_EDGE('',*,*,#15180,.T.) ;
#19459 = ORIENTED_EDGE('',*,*,#15181,.T.) ;
#19460 = ORIENTED_EDGE('',*,*,#15182,.T.) ;
#19461 = ORIENTED_EDGE('',*,*,#15183,.T.) ;
#19462 = ORIENTED_EDGE('',*,*,#15184,.T.) ;
#19463 = ORIENTED_EDGE('',*,*,#15185,.T.) ;
#19464 = ORIENTED_EDGE('',*,*,#15186,.T.) ;
#19465 = ORIENTED_EDGE('',*,*,#15187,.T.) ;
#19466 = ORIENTED_EDGE('',*,*,#15188,.T.) ;
#19467 = ORIENTED_EDGE('',*,*,#15189,.T.) ;
#19468 = ORIENTED_EDGE('',*,*,#15190,.T.) ;
#19469 = ORIENTED_EDGE('',*,*,#15191,.T.) ;
#19470 = ORIENTED_EDGE('',*,*,#15192,.T.) ;
#19471 = ORIENTED_EDGE('',*,*,#15193,.T.) ;
#19472 = ORIENTED_EDGE('',*,*,#15194,.T.) ;
#19473 = ORIENTED_EDGE('',*,*,#15195,.T.) ;
#19474 = ORIENTED_EDGE('',*,*,#15196,.T.) ;
#19475 = ORIENTED_EDGE('',*,*,#15197,.T.) ;
#19476 = ORIENTED_EDGE('',*,*,#15198,.T.) ;
#19477 = ORIENTED_EDGE('',*,*,#15199,.T.) ;
#19478 = ORIENTED_EDGE('',*,*,#15200,.T.) ;
#19479 = ORIENTED_EDGE('',*,*,#15201,.T.) ;
#19480 = ORIENTED_EDGE('',*,*,#15202,.T.) ;
#19481 = ORIENTED_EDGE('',*,*,#15203,.T.) ;
#19482 = ORIENTED_EDGE('',*,*,#14823,.T.) ;
#19483 = ORIENTED_EDGE('',*,*,#14819,.T.) ;
#19484 = ORIENTED_EDGE('',*,*,#14791,.T.) ;
#19485 = ORIENTED_EDGE('',*,*,#15204,.T.) ;
#19486 = ORIENTED_EDGE('',*,*,#15205,.T.) ;
#19487 = ORIENTED_EDGE('',*,*,#14835,.T.) ;
#19488 = ORIENTED_EDGE('',*,*,#14783,.T.) ;
#19489 = ORIENTED_EDGE('',*,*,#15206,.T.) ;
#19490 = ORIENTED_EDGE('',*,*,#15207,.T.) ;
#19491 = ORIENTED_EDGE('',*,*,#14841,.T.) ;
#19492 = ORIENTED_EDGE('',*,*,#14779,.T.) ;
#19493 = ORIENTED_EDGE('',*,*,#15208,.T.) ;
#19494 = ORIENTED_EDGE('',*,*,#15209,.T.) ;
#19495 = ORIENTED_EDGE('',*,*,#14847,.T.) ;
#19496 = ORIENTED_EDGE('',*,*,#14775,.T.) ;
#19497 = ORIENTED_EDGE('',*,*,#15210,.T.) ;
#19498 = ORIENTED_EDGE('',*,*,#15211,.T.) ;
#19499 = ORIENTED_EDGE('',*,*,#14850,.T.) ;
#19500 = ORIENTED_EDGE('',*,*,#14771,.T.) ;
#19501 = ORIENTED_EDGE('',*,*,#15212,.T.) ;
#19502 = ORIENTED_EDGE('',*,*,#15213,.T.) ;
#19503 = ORIENTED_EDGE('',*,*,#15214,.T.) ;
#19504 = ORIENTED_EDGE('',*,*,#14829,.T.) ;
#19505 = ORIENTED_EDGE('',*,*,#14787,.T.) ;
#19506 = ORIENTED_EDGE('',*,*,#14809,.T.) ;
#19507 = ORIENTED_EDGE('',*,*,#15215,.T.) ;
#19508 = ORIENTED_EDGE('',*,*,#15216,.T.) ;
#19509 = ORIENTED_EDGE('',*,*,#14832,.T.) ;
#19510 = ORIENTED_EDGE('',*,*,#14805,.T.) ;
#19511 = ORIENTED_EDGE('',*,*,#15217,.T.) ;
#19512 = ORIENTED_EDGE('',*,*,#15218,.T.) ;
#19513 = ORIENTED_EDGE('',*,*,#14838,.T.) ;
#19514 = ORIENTED_EDGE('',*,*,#14801,.T.) ;
#19515 = ORIENTED_EDGE('',*,*,#15219,.T.) ;
#19516 = ORIENTED_EDGE('',*,*,#14844,.T.) ;
#19517 = ORIENTED_EDGE('',*,*,#15220,.T.) ;
#19518 = ORIENTED_EDGE('',*,*,#15221,.T.) ;
#19519 = ORIENTED_EDGE('',*,*,#15222,.T.) ;
#19520 = ORIENTED_EDGE('',*,*,#15120,.T.) ;
#19521 = ORIENTED_EDGE('',*,*,#14767,.T.) ;
#19522 = ORIENTED_EDGE('',*,*,#14813,.T.) ;
#19523 = ORIENTED_EDGE('',*,*,#15223,.T.) ;
#19524 = ORIENTED_EDGE('',*,*,#14826,.T.) ;
#19525 = ORIENTED_EDGE('',*,*,#15224,.T.) ;
#19526 = ORIENTED_EDGE('',*,*,#15225,.T.) ;
#19527 = ORIENTED_EDGE('',*,*,#15226,.T.) ;
#19528 = ORIENTED_EDGE('',*,*,#15227,.T.) ;
#19529 = ORIENTED_EDGE('',*,*,#15228,.T.) ;
#19530 = ORIENTED_EDGE('',*,*,#15229,.T.) ;
#19531 = ORIENTED_EDGE('',*,*,#15230,.T.) ;
#19532 = ORIENTED_EDGE('',*,*,#15231,.T.) ;
#19533 = ORIENTED_EDGE('',*,*,#15232,.T.) ;
#19534 = ORIENTED_EDGE('',*,*,#15233,.T.) ;
#19535 = ORIENTED_EDGE('',*,*,#15234,.T.) ;
#19536 = ORIENTED_EDGE('',*,*,#15235,.T.) ;
#19537 = ORIENTED_EDGE('',*,*,#15236,.T.) ;
#19538 = ORIENTED_EDGE('',*,*,#15237,.T.) ;
#19539 = ORIENTED_EDGE('',*,*,#15238,.T.) ;
#19540 = ORIENTED_EDGE('',*,*,#15239,.T.) ;
#19541 = ORIENTED_EDGE('',*,*,#15240,.T.) ;
#19542 = ORIENTED_EDGE('',*,*,#15241,.T.) ;
#19543 = ORIENTED_EDGE('',*,*,#15242,.T.) ;
#19544 = ORIENTED_EDGE('',*,*,#15243,.T.) ;
#19545 = ORIENTED_EDGE('',*,*,#15244,.T.) ;
#19546 = ORIENTED_EDGE('',*,*,#15245,.T.) ;
#19547 = ORIENTED_EDGE('',*,*,#15246,.T.) ;
#19548 = ORIENTED_EDGE('',*,*,#15247,.T.) ;
#19549 = ORIENTED_EDGE('',*,*,#15248,.T.) ;
#19550 = ORIENTED_EDGE('',*,*,#15249,.T.) ;
#19551 = ORIENTED_EDGE('',*,*,#15250,.T.) ;
#19552 = ORIENTED_EDGE('',*,*,#15251,.T.) ;
#19553 = ORIENTED_EDGE('',*,*,#15252,.T.) ;
#19554 = ORIENTED_EDGE('',*,*,#15253,.T.) ;
#19555 = ORIENTED_EDGE('',*,*,#15254,.T.) ;
#19556 = ORIENTED_EDGE('',*,*,#15255,.T.) ;
#19557 = ORIENTED_EDGE('',*,*,#15256,.T.) ;
#19558 = ORIENTED_EDGE('',*,*,#15257,.T.) ;
#19559 = ORIENTED_EDGE('',*,*,#15258,.T.) ;
#19560 = ORIENTED_EDGE('',*,*,#15259,.T.) ;
#19561 = ORIENTED_EDGE('',*,*,#15260,.T.) ;
#19562 = ORIENTED_EDGE('',*,*,#15261,.T.) ;
#19563 = ORIENTED_EDGE('',*,*,#15262,.T.) ;
#19564 = ORIENTED_EDGE('',*,*,#15263,.T.) ;
#19565 = ORIENTED_EDGE('',*,*,#15264,.T.) ;
#19566 = ORIENTED_EDGE('',*,*,#15265,.T.) ;
#19567 = ORIENTED_EDGE('',*,*,#15266,.T.) ;
#19568 = ORIENTED_EDGE('',*,*,#15267,.T.) ;
#19569 = ORIENTED_EDGE('',*,*,#15268,.T.) ;
#19570 = ORIENTED_EDGE('',*,*,#15269,.T.) ;
#19571 = ORIENTED_EDGE('',*,*,#15270,.T.) ;
#19572 = ORIENTED_EDGE('',*,*,#15271,.T.) ;
#19573 = ORIENTED_EDGE('',*,*,#15272,.T.) ;
#19574 = ORIENTED_EDGE('',*,*,#15273,.T.) ;
#19575 = ORIENTED_EDGE('',*,*,#15274,.T.) ;
#19576 = ORIENTED_EDGE('',*,*,#15275,.T.) ;
#19577 = ORIENTED_EDGE('',*,*,#15276,.T.) ;
#19578 = ORIENTED_EDGE('',*,*,#15277,.T.) ;
#19579 = ORIENTED_EDGE('',*,*,#15278,.T.) ;
#19580 = ORIENTED_EDGE('',*,*,#15279,.T.) ;
#19581 = ORIENTED_EDGE('',*,*,#15280,.T.) ;
#19582 = ORIENTED_EDGE('',*,*,#15281,.T.) ;
#19583 = ORIENTED_EDGE('',*,*,#15282,.T.) ;
#19584 = ORIENTED_EDGE('',*,*,#15283,.T.) ;
#19585 = ORIENTED_EDGE('',*,*,#15284,.T.) ;
#19586 = ORIENTED_EDGE('',*,*,#15285,.T.) ;
#19587 = ORIENTED_EDGE('',*,*,#15286,.T.) ;
#19588 = ORIENTED_EDGE('',*,*,#15287,.T.) ;
#19589 = ORIENTED_EDGE('',*,*,#15288,.T.) ;
#19590 = ORIENTED_EDGE('',*,*,#15289,.T.) ;
#19591 = ORIENTED_EDGE('',*,*,#15290,.T.) ;
#19592 = ORIENTED_EDGE('',*,*,#15291,.T.) ;
#19593 = ORIENTED_EDGE('',*,*,#15292,.T.) ;
#19594 = ORIENTED_EDGE('',*,*,#15293,.T.) ;
#19595 = ORIENTED_EDGE('',*,*,#15294,.T.) ;
#19596 = ORIENTED_EDGE('',*,*,#15295,.T.) ;
#19597 = ORIENTED_EDGE('',*,*,#15296,.T.) ;
#19598 = ORIENTED_EDGE('',*,*,#15297,.T.) ;
#19599 = ORIENTED_EDGE('',*,*,#15298,.T.) ;
#19600 = ORIENTED_EDGE('',*,*,#15299,.T.) ;
#19601 = ORIENTED_EDGE('',*,*,#15300,.T.) ;
#19602 = ORIENTED_EDGE('',*,*,#15301,.T.) ;
#19603 = ORIENTED_EDGE('',*,*,#15302,.T.) ;
#19604 = ORIENTED_EDGE('',*,*,#15303,.T.) ;
#19605 = ORIENTED_EDGE('',*,*,#15304,.T.) ;
#19606 = ORIENTED_EDGE('',*,*,#15305,.T.) ;
#19607 = ORIENTED_EDGE('',*,*,#15306,.T.) ;
#19608 = ORIENTED_EDGE('',*,*,#15307,.T.) ;
#19609 = ORIENTED_EDGE('',*,*,#15308,.T.) ;
#19610 = ORIENTED_EDGE('',*,*,#15309,.T.) ;
#19611 = ORIENTED_EDGE('',*,*,#15310,.T.) ;
#19612 = ORIENTED_EDGE('',*,*,#15311,.T.) ;
#19613 = ORIENTED_EDGE('',*,*,#15312,.T.) ;
#19614 = ORIENTED_EDGE('',*,*,#15313,.T.) ;
#19615 = ORIENTED_EDGE('',*,*,#15314,.T.) ;
#19616 = ORIENTED_EDGE('',*,*,#15315,.T.) ;
#19617 = ORIENTED_EDGE('',*,*,#15316,.T.) ;
#19618 = ORIENTED_EDGE('',*,*,#15317,.T.) ;
#19619 = ORIENTED_EDGE('',*,*,#15318,.T.) ;
#19620 = ORIENTED_EDGE('',*,*,#15319,.T.) ;
#19621 = ORIENTED_EDGE('',*,*,#15320,.T.) ;
#19622 = ORIENTED_EDGE('',*,*,#15321,.T.) ;
#19623 = ORIENTED_EDGE('',*,*,#15322,.T.) ;
#19624 = ORIENTED_EDGE('',*,*,#15323,.T.) ;
#19625 = ORIENTED_EDGE('',*,*,#15324,.T.) ;
#19626 = ORIENTED_EDGE('',*,*,#15325,.T.) ;
#19627 = ORIENTED_EDGE('',*,*,#15326,.T.) ;
#19628 = ORIENTED_EDGE('',*,*,#15327,.T.) ;
#19629 = ORIENTED_EDGE('',*,*,#15328,.T.) ;
#19630 = ORIENTED_EDGE('',*,*,#15329,.T.) ;
#19631 = ORIENTED_EDGE('',*,*,#15330,.T.) ;
#19632 = ORIENTED_EDGE('',*,*,#15331,.T.) ;
#19633 = ORIENTED_EDGE('',*,*,#15332,.T.) ;
#19634 = ORIENTED_EDGE('',*,*,#15333,.T.) ;
#19635 = ORIENTED_EDGE('',*,*,#15334,.T.) ;
#19636 = ORIENTED_EDGE('',*,*,#15335,.T.) ;
#19637 = ORIENTED_EDGE('',*,*,#15336,.T.) ;
#19638 = ORIENTED_EDGE('',*,*,#15337,.T.) ;
#19639 = ORIENTED_EDGE('',*,*,#15338,.T.) ;
#19640 = ORIENTED_EDGE('',*,*,#15339,.T.) ;
#19641 = ORIENTED_EDGE('',*,*,#15340,.T.) ;
#19642 = ORIENTED_EDGE('',*,*,#15341,.T.) ;
#19643 = ORIENTED_EDGE('',*,*,#15342,.T.) ;
#19644 = ORIENTED_EDGE('',*,*,#15343,.T.) ;
#19645 = ORIENTED_EDGE('',*,*,#15344,.T.) ;
#19646 = ORIENTED_EDGE('',*,*,#15345,.T.) ;
#19647 = ORIENTED_EDGE('',*,*,#15346,.T.) ;
#19648 = ORIENTED_EDGE('',*,*,#15347,.T.) ;
#19649 = ORIENTED_EDGE('',*,*,#15348,.T.) ;
#19650 = ORIENTED_EDGE('',*,*,#15349,.T.) ;
#19651 = ORIENTED_EDGE('',*,*,#15350,.T.) ;
#19652 = ORIENTED_EDGE('',*,*,#15351,.T.) ;
#19653 = ORIENTED_EDGE('',*,*,#15352,.T.) ;
#19654 = ORIENTED_EDGE('',*,*,#15353,.T.) ;
#19655 = ORIENTED_EDGE('',*,*,#15354,.T.) ;
#19656 = ORIENTED_EDGE('',*,*,#15355,.T.) ;
#19657 = ORIENTED_EDGE('',*,*,#15356,.T.) ;
#19658 = ORIENTED_EDGE('',*,*,#15357,.T.) ;
#19659 = ORIENTED_EDGE('',*,*,#15358,.T.) ;
#19660 = ORIENTED_EDGE('',*,*,#15359,.T.) ;
#19661 = ORIENTED_EDGE('',*,*,#15360,.T.) ;
#19662 = ORIENTED_EDGE('',*,*,#15361,.T.) ;
#19663 = ORIENTED_EDGE('',*,*,#15362,.T.) ;
#19664 = ORIENTED_EDGE('',*,*,#15363,.T.) ;
#19665 = ORIENTED_EDGE('',*,*,#15364,.T.) ;
#19666 = ORIENTED_EDGE('',*,*,#15365,.T.) ;
#19667 = ORIENTED_EDGE('',*,*,#15366,.T.) ;
#19668 = ORIENTED_EDGE('',*,*,#15367,.T.) ;
#19669 = ORIENTED_EDGE('',*,*,#15368,.T.) ;
#19670 = ORIENTED_EDGE('',*,*,#15369,.T.) ;
#19671 = ORIENTED_EDGE('',*,*,#15370,.T.) ;
#19672 = ORIENTED_EDGE('',*,*,#15371,.T.) ;
#19673 = ORIENTED_EDGE('',*,*,#15372,.T.) ;
#19674 = ORIENTED_EDGE('',*,*,#15373,.T.) ;
#19675 = ORIENTED_EDGE('',*,*,#15374,.T.) ;
#19676 = ORIENTED_EDGE('',*,*,#15375,.T.) ;
#19677 = ORIENTED_EDGE('',*,*,#15376,.T.) ;
#19678 = ORIENTED_EDGE('',*,*,#15377,.T.) ;
#19679 = ORIENTED_EDGE('',*,*,#15378,.T.) ;
#19680 = ORIENTED_EDGE('',*,*,#15379,.T.) ;
#19681 = ORIENTED_EDGE('',*,*,#15380,.T.) ;
#19682 = ORIENTED_EDGE('',*,*,#15381,.T.) ;
#19683 = ORIENTED_EDGE('',*,*,#15382,.T.) ;
#19684 = ORIENTED_EDGE('',*,*,#15383,.T.) ;
#19685 = ORIENTED_EDGE('',*,*,#15384,.T.) ;
#19686 = ORIENTED_EDGE('',*,*,#15385,.T.) ;
#19687 = ORIENTED_EDGE('',*,*,#15386,.T.) ;
#19688 = ORIENTED_EDGE('',*,*,#15387,.T.) ;
#19689 = ORIENTED_EDGE('',*,*,#14814,.T.) ;
#19690 = ORIENTED_EDGE('',*,*,#14918,.F.) ;
#19691 = ORIENTED_EDGE('',*,*,#15388,.T.) ;
#19692 = ORIENTED_EDGE('',*,*,#15138,.F.) ;
#19693 = ORIENTED_EDGE('',*,*,#14794,.T.) ;
#19694 = ORIENTED_EDGE('',*,*,#15137,.F.) ;
#19695 = ORIENTED_EDGE('',*,*,#15389,.T.) ;
#19696 = ORIENTED_EDGE('',*,*,#14919,.F.) ;
#19697 = ORIENTED_EDGE('',*,*,#14824,.F.) ;
#19698 = ORIENTED_EDGE('',*,*,#15203,.F.) ;
#19699 = ORIENTED_EDGE('',*,*,#15390,.F.) ;
#19700 = ORIENTED_EDGE('',*,*,#14853,.F.) ;
#19701 = ORIENTED_EDGE('',*,*,#15391,.F.) ;
#19702 = ORIENTED_EDGE('',*,*,#14983,.F.) ;
#19703 = ORIENTED_EDGE('',*,*,#15392,.F.) ;
#19704 = ORIENTED_EDGE('',*,*,#15224,.F.) ;
#19705 = ORIENTED_EDGE('',*,*,#15393,.F.) ;
#19706 = ORIENTED_EDGE('',*,*,#14966,.F.) ;
#19707 = ORIENTED_EDGE('',*,*,#15394,.F.) ;
#19708 = ORIENTED_EDGE('',*,*,#15358,.F.) ;
#19709 = ORIENTED_EDGE('',*,*,#15395,.F.) ;
#19710 = ORIENTED_EDGE('',*,*,#14962,.F.) ;
#19711 = ORIENTED_EDGE('',*,*,#15396,.F.) ;
#19712 = ORIENTED_EDGE('',*,*,#15362,.F.) ;
#19713 = ORIENTED_EDGE('',*,*,#15397,.F.) ;
#19714 = ORIENTED_EDGE('',*,*,#15213,.F.) ;
#19715 = ORIENTED_EDGE('',*,*,#15398,.F.) ;
#19716 = ORIENTED_EDGE('',*,*,#14950,.F.) ;
#19717 = ORIENTED_EDGE('',*,*,#15399,.F.) ;
#19718 = ORIENTED_EDGE('',*,*,#15387,.F.) ;
#19719 = ORIENTED_EDGE('',*,*,#15400,.F.) ;
#19720 = ORIENTED_EDGE('',*,*,#14967,.F.) ;
#19721 = ORIENTED_EDGE('',*,*,#15401,.F.) ;
#19722 = ORIENTED_EDGE('',*,*,#14958,.F.) ;
#19723 = ORIENTED_EDGE('',*,*,#15402,.F.) ;
#19724 = ORIENTED_EDGE('',*,*,#15366,.F.) ;
#19725 = ORIENTED_EDGE('',*,*,#15403,.F.) ;
#19726 = ORIENTED_EDGE('',*,*,#15184,.F.) ;
#19727 = ORIENTED_EDGE('',*,*,#15404,.F.) ;
#19728 = ORIENTED_EDGE('',*,*,#14872,.F.) ;
#19729 = ORIENTED_EDGE('',*,*,#15405,.F.) ;
#19730 = ORIENTED_EDGE('',*,*,#15375,.F.) ;
#19731 = ORIENTED_EDGE('',*,*,#15406,.F.) ;
#19732 = ORIENTED_EDGE('',*,*,#14984,.F.) ;
#19733 = ORIENTED_EDGE('',*,*,#15407,.F.) ;
#19734 = ORIENTED_EDGE('',*,*,#15379,.F.) ;
#19735 = ORIENTED_EDGE('',*,*,#15408,.F.) ;
#19736 = ORIENTED_EDGE('',*,*,#14975,.F.) ;
#19737 = ORIENTED_EDGE('',*,*,#15409,.F.) ;
#19738 = ORIENTED_EDGE('',*,*,#15383,.F.) ;
#19739 = ORIENTED_EDGE('',*,*,#15410,.F.) ;
#19740 = ORIENTED_EDGE('',*,*,#14971,.F.) ;
#19741 = ORIENTED_EDGE('',*,*,#15411,.F.) ;
#19742 = ORIENTED_EDGE('',*,*,#14854,.F.) ;
#19743 = ORIENTED_EDGE('',*,*,#15390,.T.) ;
#19744 = ORIENTED_EDGE('',*,*,#15202,.F.) ;
#19745 = ORIENTED_EDGE('',*,*,#15412,.F.) ;
#19746 = ORIENTED_EDGE('',*,*,#14873,.F.) ;
#19747 = ORIENTED_EDGE('',*,*,#15404,.T.) ;
#19748 = ORIENTED_EDGE('',*,*,#15183,.F.) ;
#19749 = ORIENTED_EDGE('',*,*,#15413,.F.) ;
#19750 = ORIENTED_EDGE('',*,*,#14954,.F.) ;
#19751 = ORIENTED_EDGE('',*,*,#15414,.F.) ;
#19752 = ORIENTED_EDGE('',*,*,#15370,.F.) ;
#19753 = ORIENTED_EDGE('',*,*,#15413,.T.) ;
#19754 = ORIENTED_EDGE('',*,*,#15372,.F.) ;
#19755 = ORIENTED_EDGE('',*,*,#15415,.F.) ;
#19756 = ORIENTED_EDGE('',*,*,#14952,.F.) ;
#19757 = ORIENTED_EDGE('',*,*,#15401,.T.) ;
#19758 = ORIENTED_EDGE('',*,*,#15369,.F.) ;
#19759 = ORIENTED_EDGE('',*,*,#15416,.T.) ;
#19760 = ORIENTED_EDGE('',*,*,#14955,.F.) ;
#19761 = ORIENTED_EDGE('',*,*,#15400,.T.) ;
#19762 = ORIENTED_EDGE('',*,*,#15386,.F.) ;
#19763 = ORIENTED_EDGE('',*,*,#15417,.F.) ;
#19764 = ORIENTED_EDGE('',*,*,#14968,.F.) ;
#19765 = ORIENTED_EDGE('',*,*,#14786,.T.) ;
#19766 = ORIENTED_EDGE('',*,*,#14951,.F.) ;
#19767 = ORIENTED_EDGE('',*,*,#15398,.T.) ;
#19768 = ORIENTED_EDGE('',*,*,#15212,.F.) ;
#19769 = ORIENTED_EDGE('',*,*,#15411,.T.) ;
#19770 = ORIENTED_EDGE('',*,*,#15201,.F.) ;
#19771 = ORIENTED_EDGE('',*,*,#15418,.T.) ;
#19772 = ORIENTED_EDGE('',*,*,#14855,.F.) ;
#19773 = ORIENTED_EDGE('',*,*,#15410,.T.) ;
#19774 = ORIENTED_EDGE('',*,*,#15382,.F.) ;
#19775 = ORIENTED_EDGE('',*,*,#15419,.F.) ;
#19776 = ORIENTED_EDGE('',*,*,#14972,.F.) ;
#19777 = ORIENTED_EDGE('',*,*,#15395,.T.) ;
#19778 = ORIENTED_EDGE('',*,*,#15365,.F.) ;
#19779 = ORIENTED_EDGE('',*,*,#15420,.T.) ;
#19780 = ORIENTED_EDGE('',*,*,#14959,.F.) ;
#19781 = ORIENTED_EDGE('',*,*,#15408,.T.) ;
#19782 = ORIENTED_EDGE('',*,*,#15378,.F.) ;
#19783 = ORIENTED_EDGE('',*,*,#15421,.F.) ;
#19784 = ORIENTED_EDGE('',*,*,#14976,.F.) ;
#19785 = ORIENTED_EDGE('',*,*,#15393,.T.) ;
#19786 = ORIENTED_EDGE('',*,*,#15361,.F.) ;
#19787 = ORIENTED_EDGE('',*,*,#15422,.T.) ;
#19788 = ORIENTED_EDGE('',*,*,#14963,.F.) ;
#19789 = ORIENTED_EDGE('',*,*,#15391,.T.) ;
#19790 = ORIENTED_EDGE('',*,*,#15228,.F.) ;
#19791 = ORIENTED_EDGE('',*,*,#15423,.T.) ;
#19792 = ORIENTED_EDGE('',*,*,#14979,.F.) ;
#19793 = ORIENTED_EDGE('',*,*,#15406,.T.) ;
#19794 = ORIENTED_EDGE('',*,*,#15374,.F.) ;
#19795 = ORIENTED_EDGE('',*,*,#15424,.T.) ;
#19796 = ORIENTED_EDGE('',*,*,#14985,.F.) ;
#19797 = ORIENTED_EDGE('',*,*,#15403,.T.) ;
#19798 = ORIENTED_EDGE('',*,*,#14871,.F.) ;
#19799 = ORIENTED_EDGE('',*,*,#15425,.T.) ;
#19800 = ORIENTED_EDGE('',*,*,#15185,.F.) ;
#19801 = ORIENTED_EDGE('',*,*,#15412,.T.) ;
#19802 = ORIENTED_EDGE('',*,*,#15182,.F.) ;
#19803 = ORIENTED_EDGE('',*,*,#15426,.T.) ;
#19804 = ORIENTED_EDGE('',*,*,#14874,.F.) ;
#19805 = ORIENTED_EDGE('',*,*,#15427,.F.) ;
#19806 = ORIENTED_EDGE('',*,*,#15143,.F.) ;
#19807 = ORIENTED_EDGE('',*,*,#15428,.F.) ;
#19808 = ORIENTED_EDGE('',*,*,#14913,.F.) ;
#19809 = ORIENTED_EDGE('',*,*,#15418,.F.) ;
#19810 = ORIENTED_EDGE('',*,*,#15200,.F.) ;
#19811 = ORIENTED_EDGE('',*,*,#15429,.F.) ;
#19812 = ORIENTED_EDGE('',*,*,#14856,.F.) ;
#19813 = ORIENTED_EDGE('',*,*,#15430,.F.) ;
#19814 = ORIENTED_EDGE('',*,*,#14914,.F.) ;
#19815 = ORIENTED_EDGE('',*,*,#15428,.T.) ;
#19816 = ORIENTED_EDGE('',*,*,#15142,.F.) ;
#19817 = ORIENTED_EDGE('',*,*,#15431,.F.) ;
#19818 = ORIENTED_EDGE('',*,*,#15118,.F.) ;
#19819 = ORIENTED_EDGE('',*,*,#15432,.F.) ;
#19820 = ORIENTED_EDGE('',*,*,#15221,.F.) ;
#19821 = ORIENTED_EDGE('',*,*,#15433,.F.) ;
#19822 = ORIENTED_EDGE('',*,*,#14947,.F.) ;
#19823 = ORIENTED_EDGE('',*,*,#14851,.F.) ;
#19824 = ORIENTED_EDGE('',*,*,#15211,.F.) ;
#19825 = ORIENTED_EDGE('',*,*,#15434,.F.) ;
#19826 = ORIENTED_EDGE('',*,*,#14945,.F.) ;
#19827 = ORIENTED_EDGE('',*,*,#14848,.F.) ;
#19828 = ORIENTED_EDGE('',*,*,#15209,.F.) ;
#19829 = ORIENTED_EDGE('',*,*,#15435,.F.) ;
#19830 = ORIENTED_EDGE('',*,*,#14943,.F.) ;
#19831 = ORIENTED_EDGE('',*,*,#14842,.F.) ;
#19832 = ORIENTED_EDGE('',*,*,#15207,.F.) ;
#19833 = ORIENTED_EDGE('',*,*,#15397,.T.) ;
#19834 = ORIENTED_EDGE('',*,*,#14949,.F.) ;
#19835 = ORIENTED_EDGE('',*,*,#14830,.F.) ;
#19836 = ORIENTED_EDGE('',*,*,#15214,.F.) ;
#19837 = ORIENTED_EDGE('',*,*,#15436,.F.) ;
#19838 = ORIENTED_EDGE('',*,*,#15341,.F.) ;
#19839 = ORIENTED_EDGE('',*,*,#15437,.F.) ;
#19840 = ORIENTED_EDGE('',*,*,#15096,.F.) ;
#19841 = ORIENTED_EDGE('',*,*,#15438,.F.) ;
#19842 = ORIENTED_EDGE('',*,*,#15345,.F.) ;
#19843 = ORIENTED_EDGE('',*,*,#15439,.F.) ;
#19844 = ORIENTED_EDGE('',*,*,#15100,.F.) ;
#19845 = ORIENTED_EDGE('',*,*,#15440,.F.) ;
#19846 = ORIENTED_EDGE('',*,*,#15349,.F.) ;
#19847 = ORIENTED_EDGE('',*,*,#15441,.F.) ;
#19848 = ORIENTED_EDGE('',*,*,#15104,.F.) ;
#19849 = ORIENTED_EDGE('',*,*,#15442,.F.) ;
#19850 = ORIENTED_EDGE('',*,*,#15353,.F.) ;
#19851 = ORIENTED_EDGE('',*,*,#15443,.F.) ;
#19852 = ORIENTED_EDGE('',*,*,#15108,.F.) ;
#19853 = ORIENTED_EDGE('',*,*,#15444,.F.) ;
#19854 = ORIENTED_EDGE('',*,*,#15357,.F.) ;
#19855 = ORIENTED_EDGE('',*,*,#15445,.F.) ;
#19856 = ORIENTED_EDGE('',*,*,#15112,.F.) ;
#19857 = ORIENTED_EDGE('',*,*,#15446,.F.) ;
#19858 = ORIENTED_EDGE('',*,*,#14857,.F.) ;
#19859 = ORIENTED_EDGE('',*,*,#15429,.T.) ;
#19860 = ORIENTED_EDGE('',*,*,#15199,.F.) ;
#19861 = ORIENTED_EDGE('',*,*,#15447,.F.) ;
#19862 = ORIENTED_EDGE('',*,*,#14941,.F.) ;
#19863 = ORIENTED_EDGE('',*,*,#14836,.F.) ;
#19864 = ORIENTED_EDGE('',*,*,#15205,.F.) ;
#19865 = ORIENTED_EDGE('',*,*,#14782,.T.) ;
#19866 = ORIENTED_EDGE('',*,*,#14942,.F.) ;
#19867 = ORIENTED_EDGE('',*,*,#15447,.T.) ;
#19868 = ORIENTED_EDGE('',*,*,#15204,.F.) ;
#19869 = ORIENTED_EDGE('',*,*,#15417,.T.) ;
#19870 = ORIENTED_EDGE('',*,*,#15385,.F.) ;
#19871 = ORIENTED_EDGE('',*,*,#15448,.F.) ;
#19872 = ORIENTED_EDGE('',*,*,#14969,.F.) ;
#19873 = ORIENTED_EDGE('',*,*,#15446,.T.) ;
#19874 = ORIENTED_EDGE('',*,*,#15198,.F.) ;
#19875 = ORIENTED_EDGE('',*,*,#15449,.T.) ;
#19876 = ORIENTED_EDGE('',*,*,#14858,.F.) ;
#19877 = ORIENTED_EDGE('',*,*,#14778,.T.) ;
#19878 = ORIENTED_EDGE('',*,*,#14944,.F.) ;
#19879 = ORIENTED_EDGE('',*,*,#15435,.T.) ;
#19880 = ORIENTED_EDGE('',*,*,#15206,.F.) ;
#19881 = ORIENTED_EDGE('',*,*,#15445,.T.) ;
#19882 = ORIENTED_EDGE('',*,*,#15356,.F.) ;
#19883 = ORIENTED_EDGE('',*,*,#15450,.T.) ;
#19884 = ORIENTED_EDGE('',*,*,#15113,.F.) ;
#19885 = ORIENTED_EDGE('',*,*,#14774,.T.) ;
#19886 = ORIENTED_EDGE('',*,*,#14946,.F.) ;
#19887 = ORIENTED_EDGE('',*,*,#15434,.T.) ;
#19888 = ORIENTED_EDGE('',*,*,#15208,.F.) ;
#19889 = ORIENTED_EDGE('',*,*,#15443,.T.) ;
#19890 = ORIENTED_EDGE('',*,*,#15352,.F.) ;
#19891 = ORIENTED_EDGE('',*,*,#15451,.T.) ;
#19892 = ORIENTED_EDGE('',*,*,#15109,.F.) ;
#19893 = ORIENTED_EDGE('',*,*,#14770,.T.) ;
#19894 = ORIENTED_EDGE('',*,*,#14948,.F.) ;
#19895 = ORIENTED_EDGE('',*,*,#15433,.T.) ;
#19896 = ORIENTED_EDGE('',*,*,#15210,.F.) ;
#19897 = ORIENTED_EDGE('',*,*,#15441,.T.) ;
#19898 = ORIENTED_EDGE('',*,*,#15348,.F.) ;
#19899 = ORIENTED_EDGE('',*,*,#15452,.T.) ;
#19900 = ORIENTED_EDGE('',*,*,#15105,.F.) ;
#19901 = ORIENTED_EDGE('',*,*,#14766,.T.) ;
#19902 = ORIENTED_EDGE('',*,*,#15119,.F.) ;
#19903 = ORIENTED_EDGE('',*,*,#15431,.T.) ;
#19904 = ORIENTED_EDGE('',*,*,#15220,.F.) ;
#19905 = ORIENTED_EDGE('',*,*,#15439,.T.) ;
#19906 = ORIENTED_EDGE('',*,*,#15344,.F.) ;
#19907 = ORIENTED_EDGE('',*,*,#15453,.T.) ;
#19908 = ORIENTED_EDGE('',*,*,#15101,.F.) ;
#19909 = ORIENTED_EDGE('',*,*,#15430,.T.) ;
#19910 = ORIENTED_EDGE('',*,*,#15141,.F.) ;
#19911 = ORIENTED_EDGE('',*,*,#15454,.T.) ;
#19912 = ORIENTED_EDGE('',*,*,#14915,.F.) ;
#19913 = ORIENTED_EDGE('',*,*,#15437,.T.) ;
#19914 = ORIENTED_EDGE('',*,*,#15340,.F.) ;
#19915 = ORIENTED_EDGE('',*,*,#15455,.T.) ;
#19916 = ORIENTED_EDGE('',*,*,#15097,.F.) ;
#19917 = ORIENTED_EDGE('',*,*,#15456,.F.) ;
#19918 = ORIENTED_EDGE('',*,*,#15123,.F.) ;
#19919 = ORIENTED_EDGE('',*,*,#15457,.F.) ;
#19920 = ORIENTED_EDGE('',*,*,#14933,.F.) ;
#19921 = ORIENTED_EDGE('',*,*,#15458,.F.) ;
#19922 = ORIENTED_EDGE('',*,*,#15178,.F.) ;
#19923 = ORIENTED_EDGE('',*,*,#15459,.F.) ;
#19924 = ORIENTED_EDGE('',*,*,#14878,.F.) ;
#19925 = ORIENTED_EDGE('',*,*,#15422,.F.) ;
#19926 = ORIENTED_EDGE('',*,*,#15360,.F.) ;
#19927 = ORIENTED_EDGE('',*,*,#15460,.F.) ;
#19928 = ORIENTED_EDGE('',*,*,#14964,.F.) ;
#19929 = ORIENTED_EDGE('',*,*,#15420,.F.) ;
#19930 = ORIENTED_EDGE('',*,*,#15364,.F.) ;
#19931 = ORIENTED_EDGE('',*,*,#15461,.F.) ;
#19932 = ORIENTED_EDGE('',*,*,#14960,.F.) ;
#19933 = ORIENTED_EDGE('',*,*,#15462,.F.) ;
#19934 = ORIENTED_EDGE('',*,*,#14980,.F.) ;
#19935 = ORIENTED_EDGE('',*,*,#15423,.F.) ;
#19936 = ORIENTED_EDGE('',*,*,#15227,.F.) ;
#19937 = ORIENTED_EDGE('',*,*,#14821,.F.) ;
#19938 = ORIENTED_EDGE('',*,*,#14934,.F.) ;
#19939 = ORIENTED_EDGE('',*,*,#15457,.T.) ;
#19940 = ORIENTED_EDGE('',*,*,#15122,.F.) ;
#19941 = ORIENTED_EDGE('',*,*,#15416,.F.) ;
#19942 = ORIENTED_EDGE('',*,*,#15368,.F.) ;
#19943 = ORIENTED_EDGE('',*,*,#15463,.F.) ;
#19944 = ORIENTED_EDGE('',*,*,#14956,.F.) ;
#19945 = ORIENTED_EDGE('',*,*,#15464,.F.) ;
#19946 = ORIENTED_EDGE('',*,*,#15232,.F.) ;
#19947 = ORIENTED_EDGE('',*,*,#15465,.F.) ;
#19948 = ORIENTED_EDGE('',*,*,#15080,.F.) ;
#19949 = ORIENTED_EDGE('',*,*,#15466,.F.) ;
#19950 = ORIENTED_EDGE('',*,*,#15087,.F.) ;
#19951 = ORIENTED_EDGE('',*,*,#15467,.F.) ;
#19952 = ORIENTED_EDGE('',*,*,#15241,.F.) ;
#19953 = ORIENTED_EDGE('',*,*,#15444,.T.) ;
#19954 = ORIENTED_EDGE('',*,*,#15115,.F.) ;
#19955 = ORIENTED_EDGE('',*,*,#15468,.F.) ;
#19956 = ORIENTED_EDGE('',*,*,#15354,.F.) ;
#19957 = ORIENTED_EDGE('',*,*,#15469,.F.) ;
#19958 = ORIENTED_EDGE('',*,*,#15091,.F.) ;
#19959 = ORIENTED_EDGE('',*,*,#15470,.F.) ;
#19960 = ORIENTED_EDGE('',*,*,#15237,.F.) ;
#19961 = ORIENTED_EDGE('',*,*,#15471,.F.) ;
#19962 = ORIENTED_EDGE('',*,*,#15095,.F.) ;
#19963 = ORIENTED_EDGE('',*,*,#15472,.F.) ;
#19964 = ORIENTED_EDGE('',*,*,#15233,.F.) ;
#19965 = ORIENTED_EDGE('',*,*,#15473,.F.) ;
#19966 = ORIENTED_EDGE('',*,*,#14879,.F.) ;
#19967 = ORIENTED_EDGE('',*,*,#15459,.T.) ;
#19968 = ORIENTED_EDGE('',*,*,#15177,.F.) ;
#19969 = ORIENTED_EDGE('',*,*,#15399,.T.) ;
#19970 = ORIENTED_EDGE('',*,*,#14970,.F.) ;
#19971 = ORIENTED_EDGE('',*,*,#15448,.T.) ;
#19972 = ORIENTED_EDGE('',*,*,#15384,.F.) ;
#19973 = ORIENTED_EDGE('',*,*,#15409,.T.) ;
#19974 = ORIENTED_EDGE('',*,*,#14974,.F.) ;
#19975 = ORIENTED_EDGE('',*,*,#15474,.F.) ;
#19976 = ORIENTED_EDGE('',*,*,#15380,.F.) ;
#19977 = ORIENTED_EDGE('',*,*,#15471,.T.) ;
#19978 = ORIENTED_EDGE('',*,*,#15236,.F.) ;
#19979 = ORIENTED_EDGE('',*,*,#15475,.F.) ;
#19980 = ORIENTED_EDGE('',*,*,#15092,.F.) ;
#19981 = ORIENTED_EDGE('',*,*,#15402,.T.) ;
#19982 = ORIENTED_EDGE('',*,*,#14957,.F.) ;
#19983 = ORIENTED_EDGE('',*,*,#15463,.T.) ;
#19984 = ORIENTED_EDGE('',*,*,#15367,.F.) ;
#19985 = ORIENTED_EDGE('',*,*,#15469,.T.) ;
#19986 = ORIENTED_EDGE('',*,*,#15240,.F.) ;
#19987 = ORIENTED_EDGE('',*,*,#15476,.T.) ;
#19988 = ORIENTED_EDGE('',*,*,#15088,.F.) ;
#19989 = ORIENTED_EDGE('',*,*,#15414,.T.) ;
#19990 = ORIENTED_EDGE('',*,*,#14953,.F.) ;
#19991 = ORIENTED_EDGE('',*,*,#15415,.T.) ;
#19992 = ORIENTED_EDGE('',*,*,#15371,.F.) ;
#19993 = ORIENTED_EDGE('',*,*,#15456,.T.) ;
#19994 = ORIENTED_EDGE('',*,*,#14932,.F.) ;
#19995 = ORIENTED_EDGE('',*,*,#15477,.T.) ;
#19996 = ORIENTED_EDGE('',*,*,#15124,.F.) ;
#19997 = ORIENTED_EDGE('',*,*,#15462,.T.) ;
#19998 = ORIENTED_EDGE('',*,*,#15226,.F.) ;
#19999 = ORIENTED_EDGE('',*,*,#15478,.F.) ;
#20000 = ORIENTED_EDGE('',*,*,#14981,.F.) ;
#20001 = ORIENTED_EDGE('',*,*,#15458,.T.) ;
#20002 = ORIENTED_EDGE('',*,*,#14877,.F.) ;
#20003 = ORIENTED_EDGE('',*,*,#15479,.T.) ;
#20004 = ORIENTED_EDGE('',*,*,#15179,.F.) ;
#20005 = ORIENTED_EDGE('',*,*,#15473,.T.) ;
#20006 = ORIENTED_EDGE('',*,*,#15176,.F.) ;
#20007 = ORIENTED_EDGE('',*,*,#15480,.T.) ;
#20008 = ORIENTED_EDGE('',*,*,#14880,.F.) ;
#20009 = ORIENTED_EDGE('',*,*,#15396,.T.) ;
#20010 = ORIENTED_EDGE('',*,*,#14961,.F.) ;
#20011 = ORIENTED_EDGE('',*,*,#15461,.T.) ;
#20012 = ORIENTED_EDGE('',*,*,#15363,.F.) ;
#20013 = ORIENTED_EDGE('',*,*,#15466,.T.) ;
#20014 = ORIENTED_EDGE('',*,*,#15244,.F.) ;
#20015 = ORIENTED_EDGE('',*,*,#15481,.T.) ;
#20016 = ORIENTED_EDGE('',*,*,#15084,.F.) ;
#20017 = ORIENTED_EDGE('',*,*,#15394,.T.) ;
#20018 = ORIENTED_EDGE('',*,*,#14965,.F.) ;
#20019 = ORIENTED_EDGE('',*,*,#15460,.T.) ;
#20020 = ORIENTED_EDGE('',*,*,#15359,.F.) ;
#20021 = ORIENTED_EDGE('',*,*,#15465,.T.) ;
#20022 = ORIENTED_EDGE('',*,*,#15231,.F.) ;
#20023 = ORIENTED_EDGE('',*,*,#15482,.T.) ;
#20024 = ORIENTED_EDGE('',*,*,#15081,.F.) ;
#20025 = ORIENTED_EDGE('',*,*,#15483,.F.) ;
#20026 = ORIENTED_EDGE('',*,*,#15146,.F.) ;
#20027 = ORIENTED_EDGE('',*,*,#15484,.F.) ;
#20028 = ORIENTED_EDGE('',*,*,#14910,.F.) ;
#20029 = ORIENTED_EDGE('',*,*,#15449,.F.) ;
#20030 = ORIENTED_EDGE('',*,*,#15197,.F.) ;
#20031 = ORIENTED_EDGE('',*,*,#15485,.F.) ;
#20032 = ORIENTED_EDGE('',*,*,#14859,.F.) ;
#20033 = ORIENTED_EDGE('',*,*,#15486,.F.) ;
#20034 = ORIENTED_EDGE('',*,*,#15333,.F.) ;
#20035 = ORIENTED_EDGE('',*,*,#15487,.F.) ;
#20036 = ORIENTED_EDGE('',*,*,#15069,.F.) ;
#20037 = ORIENTED_EDGE('',*,*,#15488,.F.) ;
#20038 = ORIENTED_EDGE('',*,*,#15098,.F.) ;
#20039 = ORIENTED_EDGE('',*,*,#15455,.F.) ;
#20040 = ORIENTED_EDGE('',*,*,#15339,.F.) ;
#20041 = ORIENTED_EDGE('',*,*,#15489,.F.) ;
#20042 = ORIENTED_EDGE('',*,*,#15102,.F.) ;
#20043 = ORIENTED_EDGE('',*,*,#15453,.F.) ;
#20044 = ORIENTED_EDGE('',*,*,#15343,.F.) ;
#20045 = ORIENTED_EDGE('',*,*,#15490,.F.) ;
#20046 = ORIENTED_EDGE('',*,*,#15106,.F.) ;
#20047 = ORIENTED_EDGE('',*,*,#15452,.F.) ;
#20048 = ORIENTED_EDGE('',*,*,#15347,.F.) ;
#20049 = ORIENTED_EDGE('',*,*,#15491,.F.) ;
#20050 = ORIENTED_EDGE('',*,*,#14911,.F.) ;
#20051 = ORIENTED_EDGE('',*,*,#15484,.T.) ;
#20052 = ORIENTED_EDGE('',*,*,#15145,.F.) ;
#20053 = ORIENTED_EDGE('',*,*,#15468,.T.) ;
#20054 = ORIENTED_EDGE('',*,*,#15114,.F.) ;
#20055 = ORIENTED_EDGE('',*,*,#15450,.F.) ;
#20056 = ORIENTED_EDGE('',*,*,#15355,.F.) ;
#20057 = ORIENTED_EDGE('',*,*,#15492,.F.) ;
#20058 = ORIENTED_EDGE('',*,*,#15322,.F.) ;
#20059 = ORIENTED_EDGE('',*,*,#15493,.F.) ;
#20060 = ORIENTED_EDGE('',*,*,#15057,.F.) ;
#20061 = ORIENTED_EDGE('',*,*,#15494,.F.) ;
#20062 = ORIENTED_EDGE('',*,*,#15326,.F.) ;
#20063 = ORIENTED_EDGE('',*,*,#15495,.F.) ;
#20064 = ORIENTED_EDGE('',*,*,#15061,.F.) ;
#20065 = ORIENTED_EDGE('',*,*,#15496,.F.) ;
#20066 = ORIENTED_EDGE('',*,*,#15330,.F.) ;
#20067 = ORIENTED_EDGE('',*,*,#15497,.F.) ;
#20068 = ORIENTED_EDGE('',*,*,#15065,.F.) ;
#20069 = ORIENTED_EDGE('',*,*,#15498,.F.) ;
#20070 = ORIENTED_EDGE('',*,*,#15337,.F.) ;
#20071 = ORIENTED_EDGE('',*,*,#15499,.F.) ;
#20072 = ORIENTED_EDGE('',*,*,#15072,.F.) ;
#20073 = ORIENTED_EDGE('',*,*,#15500,.F.) ;
#20074 = ORIENTED_EDGE('',*,*,#15079,.F.) ;
#20075 = ORIENTED_EDGE('',*,*,#15501,.F.) ;
#20076 = ORIENTED_EDGE('',*,*,#15315,.F.) ;
#20077 = ORIENTED_EDGE('',*,*,#15502,.F.) ;
#20078 = ORIENTED_EDGE('',*,*,#14860,.F.) ;
#20079 = ORIENTED_EDGE('',*,*,#15485,.T.) ;
#20080 = ORIENTED_EDGE('',*,*,#15196,.F.) ;
#20081 = ORIENTED_EDGE('',*,*,#15503,.F.) ;
#20082 = ORIENTED_EDGE('',*,*,#15110,.F.) ;
#20083 = ORIENTED_EDGE('',*,*,#15451,.F.) ;
#20084 = ORIENTED_EDGE('',*,*,#15351,.F.) ;
#20085 = ORIENTED_EDGE('',*,*,#15442,.T.) ;
#20086 = ORIENTED_EDGE('',*,*,#15111,.F.) ;
#20087 = ORIENTED_EDGE('',*,*,#15503,.T.) ;
#20088 = ORIENTED_EDGE('',*,*,#15350,.F.) ;
#20089 = ORIENTED_EDGE('',*,*,#14812,.T.) ;
#20090 = ORIENTED_EDGE('',*,*,#14935,.F.) ;
#20091 = ORIENTED_EDGE('',*,*,#14827,.F.) ;
#20092 = ORIENTED_EDGE('',*,*,#15223,.F.) ;
#20093 = ORIENTED_EDGE('',*,*,#15475,.T.) ;
#20094 = ORIENTED_EDGE('',*,*,#15235,.F.) ;
#20095 = ORIENTED_EDGE('',*,*,#15504,.F.) ;
#20096 = ORIENTED_EDGE('',*,*,#15093,.F.) ;
#20097 = ORIENTED_EDGE('',*,*,#15502,.T.) ;
#20098 = ORIENTED_EDGE('',*,*,#15195,.F.) ;
#20099 = ORIENTED_EDGE('',*,*,#15505,.T.) ;
#20100 = ORIENTED_EDGE('',*,*,#14861,.F.) ;
#20101 = ORIENTED_EDGE('',*,*,#15427,.T.) ;
#20102 = ORIENTED_EDGE('',*,*,#14912,.F.) ;
#20103 = ORIENTED_EDGE('',*,*,#15491,.T.) ;
#20104 = ORIENTED_EDGE('',*,*,#15144,.F.) ;
#20105 = ORIENTED_EDGE('',*,*,#15486,.T.) ;
#20106 = ORIENTED_EDGE('',*,*,#15071,.F.) ;
#20107 = ORIENTED_EDGE('',*,*,#15506,.T.) ;
#20108 = ORIENTED_EDGE('',*,*,#15331,.F.) ;
#20109 = ORIENTED_EDGE('',*,*,#15500,.T.) ;
#20110 = ORIENTED_EDGE('',*,*,#15318,.F.) ;
#20111 = ORIENTED_EDGE('',*,*,#15507,.T.) ;
#20112 = ORIENTED_EDGE('',*,*,#15076,.F.) ;
#20113 = ORIENTED_EDGE('',*,*,#15440,.T.) ;
#20114 = ORIENTED_EDGE('',*,*,#15107,.F.) ;
#20115 = ORIENTED_EDGE('',*,*,#15490,.T.) ;
#20116 = ORIENTED_EDGE('',*,*,#15346,.F.) ;
#20117 = ORIENTED_EDGE('',*,*,#15499,.T.) ;
#20118 = ORIENTED_EDGE('',*,*,#15336,.F.) ;
#20119 = ORIENTED_EDGE('',*,*,#15508,.T.) ;
#20120 = ORIENTED_EDGE('',*,*,#15073,.F.) ;
#20121 = ORIENTED_EDGE('',*,*,#15438,.T.) ;
#20122 = ORIENTED_EDGE('',*,*,#15103,.F.) ;
#20123 = ORIENTED_EDGE('',*,*,#15489,.T.) ;
#20124 = ORIENTED_EDGE('',*,*,#15342,.F.) ;
#20125 = ORIENTED_EDGE('',*,*,#15497,.T.) ;
#20126 = ORIENTED_EDGE('',*,*,#15329,.F.) ;
#20127 = ORIENTED_EDGE('',*,*,#15509,.T.) ;
#20128 = ORIENTED_EDGE('',*,*,#15066,.F.) ;
#20129 = ORIENTED_EDGE('',*,*,#15436,.T.) ;
#20130 = ORIENTED_EDGE('',*,*,#15099,.F.) ;
#20131 = ORIENTED_EDGE('',*,*,#15488,.T.) ;
#20132 = ORIENTED_EDGE('',*,*,#15338,.F.) ;
#20133 = ORIENTED_EDGE('',*,*,#15495,.T.) ;
#20134 = ORIENTED_EDGE('',*,*,#15325,.F.) ;
#20135 = ORIENTED_EDGE('',*,*,#15510,.T.) ;
#20136 = ORIENTED_EDGE('',*,*,#15062,.F.) ;
#20137 = ORIENTED_EDGE('',*,*,#15487,.T.) ;
#20138 = ORIENTED_EDGE('',*,*,#15332,.F.) ;
#20139 = ORIENTED_EDGE('',*,*,#15506,.F.) ;
#20140 = ORIENTED_EDGE('',*,*,#15070,.F.) ;
#20141 = ORIENTED_EDGE('',*,*,#15493,.T.) ;
#20142 = ORIENTED_EDGE('',*,*,#15321,.F.) ;
#20143 = ORIENTED_EDGE('',*,*,#15511,.T.) ;
#20144 = ORIENTED_EDGE('',*,*,#15058,.F.) ;
#20145 = ORIENTED_EDGE('',*,*,#15512,.F.) ;
#20146 = ORIENTED_EDGE('',*,*,#15126,.F.) ;
#20147 = ORIENTED_EDGE('',*,*,#15513,.F.) ;
#20148 = ORIENTED_EDGE('',*,*,#14930,.F.) ;
#20149 = ORIENTED_EDGE('',*,*,#15514,.F.) ;
#20150 = ORIENTED_EDGE('',*,*,#15044,.F.) ;
#20151 = ORIENTED_EDGE('',*,*,#15515,.F.) ;
#20152 = ORIENTED_EDGE('',*,*,#15311,.F.) ;
#20153 = ORIENTED_EDGE('',*,*,#15516,.F.) ;
#20154 = ORIENTED_EDGE('',*,*,#15048,.F.) ;
#20155 = ORIENTED_EDGE('',*,*,#15517,.F.) ;
#20156 = ORIENTED_EDGE('',*,*,#15256,.F.) ;
#20157 = ORIENTED_EDGE('',*,*,#15518,.F.) ;
#20158 = ORIENTED_EDGE('',*,*,#15052,.F.) ;
#20159 = ORIENTED_EDGE('',*,*,#15519,.F.) ;
#20160 = ORIENTED_EDGE('',*,*,#15252,.F.) ;
#20161 = ORIENTED_EDGE('',*,*,#15498,.T.) ;
#20162 = ORIENTED_EDGE('',*,*,#15075,.F.) ;
#20163 = ORIENTED_EDGE('',*,*,#15520,.F.) ;
#20164 = ORIENTED_EDGE('',*,*,#15334,.F.) ;
#20165 = ORIENTED_EDGE('',*,*,#15521,.F.) ;
#20166 = ORIENTED_EDGE('',*,*,#15056,.F.) ;
#20167 = ORIENTED_EDGE('',*,*,#15522,.F.) ;
#20168 = ORIENTED_EDGE('',*,*,#15248,.F.) ;
#20169 = ORIENTED_EDGE('',*,*,#15480,.F.) ;
#20170 = ORIENTED_EDGE('',*,*,#15175,.F.) ;
#20171 = ORIENTED_EDGE('',*,*,#15523,.F.) ;
#20172 = ORIENTED_EDGE('',*,*,#14881,.F.) ;
#20173 = ORIENTED_EDGE('',*,*,#15524,.F.) ;
#20174 = ORIENTED_EDGE('',*,*,#15247,.F.) ;
#20175 = ORIENTED_EDGE('',*,*,#15525,.F.) ;
#20176 = ORIENTED_EDGE('',*,*,#15038,.F.) ;
#20177 = ORIENTED_EDGE('',*,*,#15482,.F.) ;
#20178 = ORIENTED_EDGE('',*,*,#15230,.F.) ;
#20179 = ORIENTED_EDGE('',*,*,#15526,.F.) ;
#20180 = ORIENTED_EDGE('',*,*,#15082,.F.) ;
#20181 = ORIENTED_EDGE('',*,*,#15481,.F.) ;
#20182 = ORIENTED_EDGE('',*,*,#15243,.F.) ;
#20183 = ORIENTED_EDGE('',*,*,#15527,.F.) ;
#20184 = ORIENTED_EDGE('',*,*,#15085,.F.) ;
#20185 = ORIENTED_EDGE('',*,*,#15476,.F.) ;
#20186 = ORIENTED_EDGE('',*,*,#15239,.F.) ;
#20187 = ORIENTED_EDGE('',*,*,#15528,.F.) ;
#20188 = ORIENTED_EDGE('',*,*,#15089,.F.) ;
#20189 = ORIENTED_EDGE('',*,*,#15477,.F.) ;
#20190 = ORIENTED_EDGE('',*,*,#14931,.F.) ;
#20191 = ORIENTED_EDGE('',*,*,#15513,.T.) ;
#20192 = ORIENTED_EDGE('',*,*,#15125,.F.) ;
#20193 = ORIENTED_EDGE('',*,*,#15529,.F.) ;
#20194 = ORIENTED_EDGE('',*,*,#14882,.F.) ;
#20195 = ORIENTED_EDGE('',*,*,#15523,.T.) ;
#20196 = ORIENTED_EDGE('',*,*,#15174,.F.) ;
#20197 = ORIENTED_EDGE('',*,*,#15472,.T.) ;
#20198 = ORIENTED_EDGE('',*,*,#15094,.F.) ;
#20199 = ORIENTED_EDGE('',*,*,#15504,.T.) ;
#20200 = ORIENTED_EDGE('',*,*,#15234,.F.) ;
#20201 = ORIENTED_EDGE('',*,*,#15407,.T.) ;
#20202 = ORIENTED_EDGE('',*,*,#14978,.F.) ;
#20203 = ORIENTED_EDGE('',*,*,#15530,.F.) ;
#20204 = ORIENTED_EDGE('',*,*,#15376,.F.) ;
#20205 = ORIENTED_EDGE('',*,*,#15521,.T.) ;
#20206 = ORIENTED_EDGE('',*,*,#15251,.F.) ;
#20207 = ORIENTED_EDGE('',*,*,#15531,.F.) ;
#20208 = ORIENTED_EDGE('',*,*,#15053,.F.) ;
#20209 = ORIENTED_EDGE('',*,*,#15474,.T.) ;
#20210 = ORIENTED_EDGE('',*,*,#14973,.F.) ;
#20211 = ORIENTED_EDGE('',*,*,#15419,.T.) ;
#20212 = ORIENTED_EDGE('',*,*,#15381,.F.) ;
#20213 = ORIENTED_EDGE('',*,*,#14833,.T.) ;
#20214 = ORIENTED_EDGE('',*,*,#15216,.F.) ;
#20215 = ORIENTED_EDGE('',*,*,#15532,.T.) ;
#20216 = ORIENTED_EDGE('',*,*,#14936,.F.) ;
#20217 = ORIENTED_EDGE('',*,*,#15512,.T.) ;
#20218 = ORIENTED_EDGE('',*,*,#14929,.F.) ;
#20219 = ORIENTED_EDGE('',*,*,#15533,.T.) ;
#20220 = ORIENTED_EDGE('',*,*,#15127,.F.) ;
#20221 = ORIENTED_EDGE('',*,*,#15470,.T.) ;
#20222 = ORIENTED_EDGE('',*,*,#15090,.F.) ;
#20223 = ORIENTED_EDGE('',*,*,#15528,.T.) ;
#20224 = ORIENTED_EDGE('',*,*,#15238,.F.) ;
#20225 = ORIENTED_EDGE('',*,*,#15518,.T.) ;
#20226 = ORIENTED_EDGE('',*,*,#15255,.F.) ;
#20227 = ORIENTED_EDGE('',*,*,#15534,.T.) ;
#20228 = ORIENTED_EDGE('',*,*,#15049,.F.) ;
#20229 = ORIENTED_EDGE('',*,*,#15467,.T.) ;
#20230 = ORIENTED_EDGE('',*,*,#15086,.F.) ;
#20231 = ORIENTED_EDGE('',*,*,#15527,.T.) ;
#20232 = ORIENTED_EDGE('',*,*,#15242,.F.) ;
#20233 = ORIENTED_EDGE('',*,*,#15516,.T.) ;
#20234 = ORIENTED_EDGE('',*,*,#15259,.F.) ;
#20235 = ORIENTED_EDGE('',*,*,#15535,.T.) ;
#20236 = ORIENTED_EDGE('',*,*,#15045,.F.) ;
#20237 = ORIENTED_EDGE('',*,*,#15464,.T.) ;
#20238 = ORIENTED_EDGE('',*,*,#15083,.F.) ;
#20239 = ORIENTED_EDGE('',*,*,#15526,.T.) ;
#20240 = ORIENTED_EDGE('',*,*,#15229,.F.) ;
#20241 = ORIENTED_EDGE('',*,*,#15514,.T.) ;
#20242 = ORIENTED_EDGE('',*,*,#15314,.F.) ;
#20243 = ORIENTED_EDGE('',*,*,#15536,.T.) ;
#20244 = ORIENTED_EDGE('',*,*,#15041,.F.) ;
#20245 = ORIENTED_EDGE('',*,*,#15525,.T.) ;
#20246 = ORIENTED_EDGE('',*,*,#15246,.F.) ;
#20247 = ORIENTED_EDGE('',*,*,#15537,.T.) ;
#20248 = ORIENTED_EDGE('',*,*,#15039,.F.) ;
#20249 = ORIENTED_EDGE('',*,*,#15529,.T.) ;
#20250 = ORIENTED_EDGE('',*,*,#15173,.F.) ;
#20251 = ORIENTED_EDGE('',*,*,#15538,.T.) ;
#20252 = ORIENTED_EDGE('',*,*,#14883,.F.) ;
#20253 = ORIENTED_EDGE('',*,*,#15505,.F.) ;
#20254 = ORIENTED_EDGE('',*,*,#15194,.F.) ;
#20255 = ORIENTED_EDGE('',*,*,#15539,.F.) ;
#20256 = ORIENTED_EDGE('',*,*,#14862,.F.) ;
#20257 = ORIENTED_EDGE('',*,*,#15507,.F.) ;
#20258 = ORIENTED_EDGE('',*,*,#15317,.F.) ;
#20259 = ORIENTED_EDGE('',*,*,#15540,.F.) ;
#20260 = ORIENTED_EDGE('',*,*,#15077,.F.) ;
#20261 = ORIENTED_EDGE('',*,*,#15541,.F.) ;
#20262 = ORIENTED_EDGE('',*,*,#15059,.F.) ;
#20263 = ORIENTED_EDGE('',*,*,#15511,.F.) ;
#20264 = ORIENTED_EDGE('',*,*,#15320,.F.) ;
#20265 = ORIENTED_EDGE('',*,*,#15542,.F.) ;
#20266 = ORIENTED_EDGE('',*,*,#14908,.F.) ;
#20267 = ORIENTED_EDGE('',*,*,#15543,.T.) ;
#20268 = ORIENTED_EDGE('',*,*,#15148,.F.) ;
#20269 = ORIENTED_EDGE('',*,*,#15544,.F.) ;
#20270 = ORIENTED_EDGE('',*,*,#15063,.F.) ;
#20271 = ORIENTED_EDGE('',*,*,#15510,.F.) ;
#20272 = ORIENTED_EDGE('',*,*,#15324,.F.) ;
#20273 = ORIENTED_EDGE('',*,*,#15520,.T.) ;
#20274 = ORIENTED_EDGE('',*,*,#15074,.F.) ;
#20275 = ORIENTED_EDGE('',*,*,#15508,.F.) ;
#20276 = ORIENTED_EDGE('',*,*,#15335,.F.) ;
#20277 = ORIENTED_EDGE('',*,*,#15545,.F.) ;
#20278 = ORIENTED_EDGE('',*,*,#15067,.F.) ;
#20279 = ORIENTED_EDGE('',*,*,#15509,.F.) ;
#20280 = ORIENTED_EDGE('',*,*,#15328,.F.) ;
#20281 = ORIENTED_EDGE('',*,*,#15546,.F.) ;
#20282 = ORIENTED_EDGE('',*,*,#15150,.F.) ;
#20283 = ORIENTED_EDGE('',*,*,#15547,.F.) ;
#20284 = ORIENTED_EDGE('',*,*,#14906,.F.) ;
#20285 = ORIENTED_EDGE('',*,*,#15548,.F.) ;
#20286 = ORIENTED_EDGE('',*,*,#15271,.F.) ;
#20287 = ORIENTED_EDGE('',*,*,#15549,.F.) ;
#20288 = ORIENTED_EDGE('',*,*,#14999,.F.) ;
#20289 = ORIENTED_EDGE('',*,*,#15550,.F.) ;
#20290 = ORIENTED_EDGE('',*,*,#15267,.F.) ;
#20291 = ORIENTED_EDGE('',*,*,#15551,.F.) ;
#20292 = ORIENTED_EDGE('',*,*,#14995,.F.) ;
#20293 = ORIENTED_EDGE('',*,*,#15552,.F.) ;
#20294 = ORIENTED_EDGE('',*,*,#14990,.F.) ;
#20295 = ORIENTED_EDGE('',*,*,#15553,.F.) ;
#20296 = ORIENTED_EDGE('',*,*,#15272,.F.) ;
#20297 = ORIENTED_EDGE('',*,*,#15554,.F.) ;
#20298 = ORIENTED_EDGE('',*,*,#15263,.F.) ;
#20299 = ORIENTED_EDGE('',*,*,#15555,.F.) ;
#20300 = ORIENTED_EDGE('',*,*,#14991,.F.) ;
#20301 = ORIENTED_EDGE('',*,*,#15556,.F.) ;
#20302 = ORIENTED_EDGE('',*,*,#14864,.F.) ;
#20303 = ORIENTED_EDGE('',*,*,#15557,.T.) ;
#20304 = ORIENTED_EDGE('',*,*,#15192,.F.) ;
#20305 = ORIENTED_EDGE('',*,*,#14907,.F.) ;
#20306 = ORIENTED_EDGE('',*,*,#15547,.T.) ;
#20307 = ORIENTED_EDGE('',*,*,#15149,.F.) ;
#20308 = ORIENTED_EDGE('',*,*,#15543,.F.) ;
#20309 = ORIENTED_EDGE('',*,*,#14863,.F.) ;
#20310 = ORIENTED_EDGE('',*,*,#15539,.T.) ;
#20311 = ORIENTED_EDGE('',*,*,#15193,.F.) ;
#20312 = ORIENTED_EDGE('',*,*,#15557,.F.) ;
#20313 = ORIENTED_EDGE('',*,*,#15531,.T.) ;
#20314 = ORIENTED_EDGE('',*,*,#15250,.F.) ;
#20315 = ORIENTED_EDGE('',*,*,#15558,.F.) ;
#20316 = ORIENTED_EDGE('',*,*,#15054,.F.) ;
#20317 = ORIENTED_EDGE('',*,*,#15554,.T.) ;
#20318 = ORIENTED_EDGE('',*,*,#14994,.F.) ;
#20319 = ORIENTED_EDGE('',*,*,#15559,.F.) ;
#20320 = ORIENTED_EDGE('',*,*,#15260,.F.) ;
#20321 = ORIENTED_EDGE('',*,*,#15496,.T.) ;
#20322 = ORIENTED_EDGE('',*,*,#15068,.F.) ;
#20323 = ORIENTED_EDGE('',*,*,#15545,.T.) ;
#20324 = ORIENTED_EDGE('',*,*,#15327,.F.) ;
#20325 = ORIENTED_EDGE('',*,*,#15530,.T.) ;
#20326 = ORIENTED_EDGE('',*,*,#14977,.F.) ;
#20327 = ORIENTED_EDGE('',*,*,#15421,.T.) ;
#20328 = ORIENTED_EDGE('',*,*,#15377,.F.) ;
#20329 = ORIENTED_EDGE('',*,*,#15556,.T.) ;
#20330 = ORIENTED_EDGE('',*,*,#15191,.F.) ;
#20331 = ORIENTED_EDGE('',*,*,#15560,.T.) ;
#20332 = ORIENTED_EDGE('',*,*,#14865,.F.) ;
#20333 = ORIENTED_EDGE('',*,*,#15494,.T.) ;
#20334 = ORIENTED_EDGE('',*,*,#15064,.F.) ;
#20335 = ORIENTED_EDGE('',*,*,#15544,.T.) ;
#20336 = ORIENTED_EDGE('',*,*,#15323,.F.) ;
#20337 = ORIENTED_EDGE('',*,*,#15555,.T.) ;
#20338 = ORIENTED_EDGE('',*,*,#15262,.F.) ;
#20339 = ORIENTED_EDGE('',*,*,#15561,.T.) ;
#20340 = ORIENTED_EDGE('',*,*,#14992,.F.) ;
#20341 = ORIENTED_EDGE('',*,*,#15483,.T.) ;
#20342 = ORIENTED_EDGE('',*,*,#14909,.F.) ;
#20343 = ORIENTED_EDGE('',*,*,#15542,.T.) ;
#20344 = ORIENTED_EDGE('',*,*,#15147,.F.) ;
#20345 = ORIENTED_EDGE('',*,*,#15546,.T.) ;
#20346 = ORIENTED_EDGE('',*,*,#14905,.F.) ;
#20347 = ORIENTED_EDGE('',*,*,#15562,.T.) ;
#20348 = ORIENTED_EDGE('',*,*,#15151,.F.) ;
#20349 = ORIENTED_EDGE('',*,*,#15552,.T.) ;
#20350 = ORIENTED_EDGE('',*,*,#15275,.F.) ;
#20351 = ORIENTED_EDGE('',*,*,#15563,.T.) ;
#20352 = ORIENTED_EDGE('',*,*,#14987,.F.) ;
#20353 = ORIENTED_EDGE('',*,*,#15492,.T.) ;
#20354 = ORIENTED_EDGE('',*,*,#15060,.F.) ;
#20355 = ORIENTED_EDGE('',*,*,#15541,.T.) ;
#20356 = ORIENTED_EDGE('',*,*,#15319,.F.) ;
#20357 = ORIENTED_EDGE('',*,*,#15551,.T.) ;
#20358 = ORIENTED_EDGE('',*,*,#15266,.F.) ;
#20359 = ORIENTED_EDGE('',*,*,#15564,.T.) ;
#20360 = ORIENTED_EDGE('',*,*,#14996,.F.) ;
#20361 = ORIENTED_EDGE('',*,*,#15501,.T.) ;
#20362 = ORIENTED_EDGE('',*,*,#15078,.F.) ;
#20363 = ORIENTED_EDGE('',*,*,#15540,.T.) ;
#20364 = ORIENTED_EDGE('',*,*,#15316,.F.) ;
#20365 = ORIENTED_EDGE('',*,*,#15549,.T.) ;
#20366 = ORIENTED_EDGE('',*,*,#15270,.F.) ;
#20367 = ORIENTED_EDGE('',*,*,#15565,.T.) ;
#20368 = ORIENTED_EDGE('',*,*,#15000,.F.) ;
#20369 = ORIENTED_EDGE('',*,*,#15538,.F.) ;
#20370 = ORIENTED_EDGE('',*,*,#15172,.F.) ;
#20371 = ORIENTED_EDGE('',*,*,#15566,.F.) ;
#20372 = ORIENTED_EDGE('',*,*,#14884,.F.) ;
#20373 = ORIENTED_EDGE('',*,*,#15536,.F.) ;
#20374 = ORIENTED_EDGE('',*,*,#15313,.F.) ;
#20375 = ORIENTED_EDGE('',*,*,#15567,.F.) ;
#20376 = ORIENTED_EDGE('',*,*,#15042,.F.) ;
#20377 = ORIENTED_EDGE('',*,*,#15535,.F.) ;
#20378 = ORIENTED_EDGE('',*,*,#15258,.F.) ;
#20379 = ORIENTED_EDGE('',*,*,#15568,.F.) ;
#20380 = ORIENTED_EDGE('',*,*,#15046,.F.) ;
#20381 = ORIENTED_EDGE('',*,*,#15533,.F.) ;
#20382 = ORIENTED_EDGE('',*,*,#14928,.F.) ;
#20383 = ORIENTED_EDGE('',*,*,#15569,.T.) ;
#20384 = ORIENTED_EDGE('',*,*,#15128,.F.) ;
#20385 = ORIENTED_EDGE('',*,*,#15534,.F.) ;
#20386 = ORIENTED_EDGE('',*,*,#15254,.F.) ;
#20387 = ORIENTED_EDGE('',*,*,#15570,.F.) ;
#20388 = ORIENTED_EDGE('',*,*,#15050,.F.) ;
#20389 = ORIENTED_EDGE('',*,*,#14808,.T.) ;
#20390 = ORIENTED_EDGE('',*,*,#14937,.F.) ;
#20391 = ORIENTED_EDGE('',*,*,#15532,.F.) ;
#20392 = ORIENTED_EDGE('',*,*,#15215,.F.) ;
#20393 = ORIENTED_EDGE('',*,*,#15571,.F.) ;
#20394 = ORIENTED_EDGE('',*,*,#15130,.F.) ;
#20395 = ORIENTED_EDGE('',*,*,#15572,.F.) ;
#20396 = ORIENTED_EDGE('',*,*,#14926,.F.) ;
#20397 = ORIENTED_EDGE('',*,*,#15573,.F.) ;
#20398 = ORIENTED_EDGE('',*,*,#14886,.F.) ;
#20399 = ORIENTED_EDGE('',*,*,#15574,.T.) ;
#20400 = ORIENTED_EDGE('',*,*,#15170,.F.) ;
#20401 = ORIENTED_EDGE('',*,*,#15575,.F.) ;
#20402 = ORIENTED_EDGE('',*,*,#15014,.F.) ;
#20403 = ORIENTED_EDGE('',*,*,#15576,.F.) ;
#20404 = ORIENTED_EDGE('',*,*,#15276,.F.) ;
#20405 = ORIENTED_EDGE('',*,*,#15577,.F.) ;
#20406 = ORIENTED_EDGE('',*,*,#15010,.F.) ;
#20407 = ORIENTED_EDGE('',*,*,#15578,.F.) ;
#20408 = ORIENTED_EDGE('',*,*,#15303,.F.) ;
#20409 = ORIENTED_EDGE('',*,*,#15579,.F.) ;
#20410 = ORIENTED_EDGE('',*,*,#15006,.F.) ;
#20411 = ORIENTED_EDGE('',*,*,#15580,.F.) ;
#20412 = ORIENTED_EDGE('',*,*,#15307,.F.) ;
#20413 = ORIENTED_EDGE('',*,*,#14885,.F.) ;
#20414 = ORIENTED_EDGE('',*,*,#15566,.T.) ;
#20415 = ORIENTED_EDGE('',*,*,#15171,.F.) ;
#20416 = ORIENTED_EDGE('',*,*,#15574,.F.) ;
#20417 = ORIENTED_EDGE('',*,*,#14927,.F.) ;
#20418 = ORIENTED_EDGE('',*,*,#15572,.T.) ;
#20419 = ORIENTED_EDGE('',*,*,#15129,.F.) ;
#20420 = ORIENTED_EDGE('',*,*,#15569,.F.) ;
#20421 = ORIENTED_EDGE('',*,*,#15579,.T.) ;
#20422 = ORIENTED_EDGE('',*,*,#15310,.F.) ;
#20423 = ORIENTED_EDGE('',*,*,#15581,.F.) ;
#20424 = ORIENTED_EDGE('',*,*,#15003,.F.) ;
#20425 = ORIENTED_EDGE('',*,*,#15559,.T.) ;
#20426 = ORIENTED_EDGE('',*,*,#14993,.F.) ;
#20427 = ORIENTED_EDGE('',*,*,#15561,.F.) ;
#20428 = ORIENTED_EDGE('',*,*,#15261,.F.) ;
#20429 = ORIENTED_EDGE('',*,*,#15522,.T.) ;
#20430 = ORIENTED_EDGE('',*,*,#15055,.F.) ;
#20431 = ORIENTED_EDGE('',*,*,#15558,.T.) ;
#20432 = ORIENTED_EDGE('',*,*,#15249,.F.) ;
#20433 = ORIENTED_EDGE('',*,*,#15519,.T.) ;
#20434 = ORIENTED_EDGE('',*,*,#15051,.F.) ;
#20435 = ORIENTED_EDGE('',*,*,#15570,.T.) ;
#20436 = ORIENTED_EDGE('',*,*,#15253,.F.) ;
#20437 = ORIENTED_EDGE('',*,*,#15577,.T.) ;
#20438 = ORIENTED_EDGE('',*,*,#15306,.F.) ;
#20439 = ORIENTED_EDGE('',*,*,#15582,.T.) ;
#20440 = ORIENTED_EDGE('',*,*,#15007,.F.) ;
#20441 = ORIENTED_EDGE('',*,*,#14839,.T.) ;
#20442 = ORIENTED_EDGE('',*,*,#15218,.F.) ;
#20443 = ORIENTED_EDGE('',*,*,#15583,.T.) ;
#20444 = ORIENTED_EDGE('',*,*,#14938,.F.) ;
#20445 = ORIENTED_EDGE('',*,*,#15517,.T.) ;
#20446 = ORIENTED_EDGE('',*,*,#15047,.F.) ;
#20447 = ORIENTED_EDGE('',*,*,#15568,.T.) ;
#20448 = ORIENTED_EDGE('',*,*,#15257,.F.) ;
#20449 = ORIENTED_EDGE('',*,*,#15575,.T.) ;
#20450 = ORIENTED_EDGE('',*,*,#15279,.F.) ;
#20451 = ORIENTED_EDGE('',*,*,#15584,.T.) ;
#20452 = ORIENTED_EDGE('',*,*,#15011,.F.) ;
#20453 = ORIENTED_EDGE('',*,*,#15576,.T.) ;
#20454 = ORIENTED_EDGE('',*,*,#15013,.F.) ;
#20455 = ORIENTED_EDGE('',*,*,#15585,.T.) ;
#20456 = ORIENTED_EDGE('',*,*,#15277,.F.) ;
#20457 = ORIENTED_EDGE('',*,*,#15515,.T.) ;
#20458 = ORIENTED_EDGE('',*,*,#15043,.F.) ;
#20459 = ORIENTED_EDGE('',*,*,#15567,.T.) ;
#20460 = ORIENTED_EDGE('',*,*,#15312,.F.) ;
#20461 = ORIENTED_EDGE('',*,*,#15573,.T.) ;
#20462 = ORIENTED_EDGE('',*,*,#15169,.F.) ;
#20463 = ORIENTED_EDGE('',*,*,#15586,.T.) ;
#20464 = ORIENTED_EDGE('',*,*,#14887,.F.) ;
#20465 = ORIENTED_EDGE('',*,*,#15560,.F.) ;
#20466 = ORIENTED_EDGE('',*,*,#15190,.F.) ;
#20467 = ORIENTED_EDGE('',*,*,#15587,.F.) ;
#20468 = ORIENTED_EDGE('',*,*,#14866,.F.) ;
#20469 = ORIENTED_EDGE('',*,*,#15588,.F.) ;
#20470 = ORIENTED_EDGE('',*,*,#15153,.F.) ;
#20471 = ORIENTED_EDGE('',*,*,#15589,.F.) ;
#20472 = ORIENTED_EDGE('',*,*,#14903,.F.) ;
#20473 = ORIENTED_EDGE('',*,*,#15590,.F.) ;
#20474 = ORIENTED_EDGE('',*,*,#15294,.F.) ;
#20475 = ORIENTED_EDGE('',*,*,#15591,.F.) ;
#20476 = ORIENTED_EDGE('',*,*,#15023,.F.) ;
#20477 = ORIENTED_EDGE('',*,*,#15592,.F.) ;
#20478 = ORIENTED_EDGE('',*,*,#15298,.F.) ;
#20479 = ORIENTED_EDGE('',*,*,#15593,.F.) ;
#20480 = ORIENTED_EDGE('',*,*,#15015,.F.) ;
#20481 = ORIENTED_EDGE('',*,*,#15594,.F.) ;
#20482 = ORIENTED_EDGE('',*,*,#14867,.F.) ;
#20483 = ORIENTED_EDGE('',*,*,#15587,.T.) ;
#20484 = ORIENTED_EDGE('',*,*,#15189,.F.) ;
#20485 = ORIENTED_EDGE('',*,*,#15595,.F.) ;
#20486 = ORIENTED_EDGE('',*,*,#15302,.F.) ;
#20487 = ORIENTED_EDGE('',*,*,#15596,.F.) ;
#20488 = ORIENTED_EDGE('',*,*,#15019,.F.) ;
#20489 = ORIENTED_EDGE('',*,*,#15405,.T.) ;
#20490 = ORIENTED_EDGE('',*,*,#14986,.F.) ;
#20491 = ORIENTED_EDGE('',*,*,#15424,.F.) ;
#20492 = ORIENTED_EDGE('',*,*,#15373,.F.) ;
#20493 = ORIENTED_EDGE('',*,*,#15597,.F.) ;
#20494 = ORIENTED_EDGE('',*,*,#14988,.F.) ;
#20495 = ORIENTED_EDGE('',*,*,#15563,.F.) ;
#20496 = ORIENTED_EDGE('',*,*,#15274,.F.) ;
#20497 = ORIENTED_EDGE('',*,*,#15598,.F.) ;
#20498 = ORIENTED_EDGE('',*,*,#15001,.F.) ;
#20499 = ORIENTED_EDGE('',*,*,#15565,.F.) ;
#20500 = ORIENTED_EDGE('',*,*,#15269,.F.) ;
#20501 = ORIENTED_EDGE('',*,*,#15562,.F.) ;
#20502 = ORIENTED_EDGE('',*,*,#14904,.F.) ;
#20503 = ORIENTED_EDGE('',*,*,#15589,.T.) ;
#20504 = ORIENTED_EDGE('',*,*,#15152,.F.) ;
#20505 = ORIENTED_EDGE('',*,*,#15599,.F.) ;
#20506 = ORIENTED_EDGE('',*,*,#14997,.F.) ;
#20507 = ORIENTED_EDGE('',*,*,#15564,.F.) ;
#20508 = ORIENTED_EDGE('',*,*,#15265,.F.) ;
#20509 = ORIENTED_EDGE('',*,*,#15550,.T.) ;
#20510 = ORIENTED_EDGE('',*,*,#14998,.F.) ;
#20511 = ORIENTED_EDGE('',*,*,#15599,.T.) ;
#20512 = ORIENTED_EDGE('',*,*,#15264,.F.) ;
#20513 = ORIENTED_EDGE('',*,*,#14804,.T.) ;
#20514 = ORIENTED_EDGE('',*,*,#14939,.F.) ;
#20515 = ORIENTED_EDGE('',*,*,#15583,.F.) ;
#20516 = ORIENTED_EDGE('',*,*,#15217,.F.) ;
#20517 = ORIENTED_EDGE('',*,*,#15581,.T.) ;
#20518 = ORIENTED_EDGE('',*,*,#15309,.F.) ;
#20519 = ORIENTED_EDGE('',*,*,#15600,.F.) ;
#20520 = ORIENTED_EDGE('',*,*,#15004,.F.) ;
#20521 = ORIENTED_EDGE('',*,*,#15548,.T.) ;
#20522 = ORIENTED_EDGE('',*,*,#15002,.F.) ;
#20523 = ORIENTED_EDGE('',*,*,#15598,.T.) ;
#20524 = ORIENTED_EDGE('',*,*,#15268,.F.) ;
#20525 = ORIENTED_EDGE('',*,*,#15596,.T.) ;
#20526 = ORIENTED_EDGE('',*,*,#15301,.F.) ;
#20527 = ORIENTED_EDGE('',*,*,#15601,.T.) ;
#20528 = ORIENTED_EDGE('',*,*,#15020,.F.) ;
#20529 = ORIENTED_EDGE('',*,*,#15594,.T.) ;
#20530 = ORIENTED_EDGE('',*,*,#15188,.F.) ;
#20531 = ORIENTED_EDGE('',*,*,#15602,.T.) ;
#20532 = ORIENTED_EDGE('',*,*,#14868,.F.) ;
#20533 = ORIENTED_EDGE('',*,*,#15593,.T.) ;
#20534 = ORIENTED_EDGE('',*,*,#15297,.F.) ;
#20535 = ORIENTED_EDGE('',*,*,#15603,.T.) ;
#20536 = ORIENTED_EDGE('',*,*,#15016,.F.) ;
#20537 = ORIENTED_EDGE('',*,*,#15553,.T.) ;
#20538 = ORIENTED_EDGE('',*,*,#14989,.F.) ;
#20539 = ORIENTED_EDGE('',*,*,#15597,.T.) ;
#20540 = ORIENTED_EDGE('',*,*,#15273,.F.) ;
#20541 = ORIENTED_EDGE('',*,*,#15588,.T.) ;
#20542 = ORIENTED_EDGE('',*,*,#14902,.F.) ;
#20543 = ORIENTED_EDGE('',*,*,#15604,.T.) ;
#20544 = ORIENTED_EDGE('',*,*,#15154,.F.) ;
#20545 = ORIENTED_EDGE('',*,*,#15591,.T.) ;
#20546 = ORIENTED_EDGE('',*,*,#15293,.F.) ;
#20547 = ORIENTED_EDGE('',*,*,#15605,.T.) ;
#20548 = ORIENTED_EDGE('',*,*,#15024,.F.) ;
#20549 = ORIENTED_EDGE('',*,*,#15586,.F.) ;
#20550 = ORIENTED_EDGE('',*,*,#15168,.F.) ;
#20551 = ORIENTED_EDGE('',*,*,#15606,.F.) ;
#20552 = ORIENTED_EDGE('',*,*,#14888,.F.) ;
#20553 = ORIENTED_EDGE('',*,*,#15584,.F.) ;
#20554 = ORIENTED_EDGE('',*,*,#15278,.F.) ;
#20555 = ORIENTED_EDGE('',*,*,#15585,.F.) ;
#20556 = ORIENTED_EDGE('',*,*,#15012,.F.) ;
#20557 = ORIENTED_EDGE('',*,*,#15582,.F.) ;
#20558 = ORIENTED_EDGE('',*,*,#15305,.F.) ;
#20559 = ORIENTED_EDGE('',*,*,#15607,.F.) ;
#20560 = ORIENTED_EDGE('',*,*,#15008,.F.) ;
#20561 = ORIENTED_EDGE('',*,*,#15608,.F.) ;
#20562 = ORIENTED_EDGE('',*,*,#14889,.F.) ;
#20563 = ORIENTED_EDGE('',*,*,#15606,.T.) ;
#20564 = ORIENTED_EDGE('',*,*,#15167,.F.) ;
#20565 = ORIENTED_EDGE('',*,*,#15609,.F.) ;
#20566 = ORIENTED_EDGE('',*,*,#15033,.F.) ;
#20567 = ORIENTED_EDGE('',*,*,#15610,.F.) ;
#20568 = ORIENTED_EDGE('',*,*,#15285,.F.) ;
#20569 = ORIENTED_EDGE('',*,*,#15611,.F.) ;
#20570 = ORIENTED_EDGE('',*,*,#15133,.F.) ;
#20571 = ORIENTED_EDGE('',*,*,#15612,.F.) ;
#20572 = ORIENTED_EDGE('',*,*,#14923,.F.) ;
#20573 = ORIENTED_EDGE('',*,*,#15613,.F.) ;
#20574 = ORIENTED_EDGE('',*,*,#15037,.F.) ;
#20575 = ORIENTED_EDGE('',*,*,#15614,.F.) ;
#20576 = ORIENTED_EDGE('',*,*,#15288,.F.) ;
#20577 = ORIENTED_EDGE('',*,*,#15595,.T.) ;
#20578 = ORIENTED_EDGE('',*,*,#15022,.F.) ;
#20579 = ORIENTED_EDGE('',*,*,#15615,.F.) ;
#20580 = ORIENTED_EDGE('',*,*,#15299,.F.) ;
#20581 = ORIENTED_EDGE('',*,*,#15616,.F.) ;
#20582 = ORIENTED_EDGE('',*,*,#14924,.F.) ;
#20583 = ORIENTED_EDGE('',*,*,#15612,.T.) ;
#20584 = ORIENTED_EDGE('',*,*,#15132,.F.) ;
#20585 = ORIENTED_EDGE('',*,*,#15580,.T.) ;
#20586 = ORIENTED_EDGE('',*,*,#15005,.F.) ;
#20587 = ORIENTED_EDGE('',*,*,#15600,.T.) ;
#20588 = ORIENTED_EDGE('',*,*,#15308,.F.) ;
#20589 = ORIENTED_EDGE('',*,*,#15613,.T.) ;
#20590 = ORIENTED_EDGE('',*,*,#15291,.F.) ;
#20591 = ORIENTED_EDGE('',*,*,#15617,.F.) ;
#20592 = ORIENTED_EDGE('',*,*,#15034,.F.) ;
#20593 = ORIENTED_EDGE('',*,*,#14800,.T.) ;
#20594 = ORIENTED_EDGE('',*,*,#14940,.F.) ;
#20595 = ORIENTED_EDGE('',*,*,#14845,.T.) ;
#20596 = ORIENTED_EDGE('',*,*,#15219,.F.) ;
#20597 = ORIENTED_EDGE('',*,*,#15611,.T.) ;
#20598 = ORIENTED_EDGE('',*,*,#14922,.F.) ;
#20599 = ORIENTED_EDGE('',*,*,#15618,.T.) ;
#20600 = ORIENTED_EDGE('',*,*,#15134,.F.) ;
#20601 = ORIENTED_EDGE('',*,*,#15571,.T.) ;
#20602 = ORIENTED_EDGE('',*,*,#14925,.F.) ;
#20603 = ORIENTED_EDGE('',*,*,#15616,.T.) ;
#20604 = ORIENTED_EDGE('',*,*,#15131,.F.) ;
#20605 = ORIENTED_EDGE('',*,*,#15578,.T.) ;
#20606 = ORIENTED_EDGE('',*,*,#15009,.F.) ;
#20607 = ORIENTED_EDGE('',*,*,#15607,.T.) ;
#20608 = ORIENTED_EDGE('',*,*,#15304,.F.) ;
#20609 = ORIENTED_EDGE('',*,*,#15609,.T.) ;
#20610 = ORIENTED_EDGE('',*,*,#15287,.F.) ;
#20611 = ORIENTED_EDGE('',*,*,#15619,.F.) ;
#20612 = ORIENTED_EDGE('',*,*,#15031,.F.) ;
#20613 = ORIENTED_EDGE('',*,*,#15608,.T.) ;
#20614 = ORIENTED_EDGE('',*,*,#15166,.F.) ;
#20615 = ORIENTED_EDGE('',*,*,#15620,.T.) ;
#20616 = ORIENTED_EDGE('',*,*,#14890,.F.) ;
#20617 = ORIENTED_EDGE('',*,*,#15610,.T.) ;
#20618 = ORIENTED_EDGE('',*,*,#15032,.F.) ;
#20619 = ORIENTED_EDGE('',*,*,#15619,.T.) ;
#20620 = ORIENTED_EDGE('',*,*,#15286,.F.) ;
#20621 = ORIENTED_EDGE('',*,*,#15602,.F.) ;
#20622 = ORIENTED_EDGE('',*,*,#15187,.F.) ;
#20623 = ORIENTED_EDGE('',*,*,#15621,.F.) ;
#20624 = ORIENTED_EDGE('',*,*,#14869,.F.) ;
#20625 = ORIENTED_EDGE('',*,*,#15615,.T.) ;
#20626 = ORIENTED_EDGE('',*,*,#15021,.F.) ;
#20627 = ORIENTED_EDGE('',*,*,#15601,.F.) ;
#20628 = ORIENTED_EDGE('',*,*,#15300,.F.) ;
#20629 = ORIENTED_EDGE('',*,*,#15622,.F.) ;
#20630 = ORIENTED_EDGE('',*,*,#15156,.F.) ;
#20631 = ORIENTED_EDGE('',*,*,#15623,.F.) ;
#20632 = ORIENTED_EDGE('',*,*,#14900,.F.) ;
#20633 = ORIENTED_EDGE('',*,*,#15425,.F.) ;
#20634 = ORIENTED_EDGE('',*,*,#14870,.F.) ;
#20635 = ORIENTED_EDGE('',*,*,#15621,.T.) ;
#20636 = ORIENTED_EDGE('',*,*,#15186,.F.) ;
#20637 = ORIENTED_EDGE('',*,*,#15624,.F.) ;
#20638 = ORIENTED_EDGE('',*,*,#15284,.F.) ;
#20639 = ORIENTED_EDGE('',*,*,#15625,.F.) ;
#20640 = ORIENTED_EDGE('',*,*,#15026,.F.) ;
#20641 = ORIENTED_EDGE('',*,*,#15604,.F.) ;
#20642 = ORIENTED_EDGE('',*,*,#14901,.F.) ;
#20643 = ORIENTED_EDGE('',*,*,#15623,.T.) ;
#20644 = ORIENTED_EDGE('',*,*,#15155,.F.) ;
#20645 = ORIENTED_EDGE('',*,*,#15626,.F.) ;
#20646 = ORIENTED_EDGE('',*,*,#15017,.F.) ;
#20647 = ORIENTED_EDGE('',*,*,#15603,.F.) ;
#20648 = ORIENTED_EDGE('',*,*,#15296,.F.) ;
#20649 = ORIENTED_EDGE('',*,*,#15592,.T.) ;
#20650 = ORIENTED_EDGE('',*,*,#15018,.F.) ;
#20651 = ORIENTED_EDGE('',*,*,#15626,.T.) ;
#20652 = ORIENTED_EDGE('',*,*,#15295,.F.) ;
#20653 = ORIENTED_EDGE('',*,*,#15617,.T.) ;
#20654 = ORIENTED_EDGE('',*,*,#15290,.F.) ;
#20655 = ORIENTED_EDGE('',*,*,#15627,.F.) ;
#20656 = ORIENTED_EDGE('',*,*,#15035,.F.) ;
#20657 = ORIENTED_EDGE('',*,*,#15392,.T.) ;
#20658 = ORIENTED_EDGE('',*,*,#14982,.F.) ;
#20659 = ORIENTED_EDGE('',*,*,#15478,.T.) ;
#20660 = ORIENTED_EDGE('',*,*,#15225,.F.) ;
#20661 = ORIENTED_EDGE('',*,*,#15625,.T.) ;
#20662 = ORIENTED_EDGE('',*,*,#15283,.F.) ;
#20663 = ORIENTED_EDGE('',*,*,#15628,.F.) ;
#20664 = ORIENTED_EDGE('',*,*,#15027,.F.) ;
#20665 = ORIENTED_EDGE('',*,*,#15622,.T.) ;
#20666 = ORIENTED_EDGE('',*,*,#14899,.F.) ;
#20667 = ORIENTED_EDGE('',*,*,#15629,.T.) ;
#20668 = ORIENTED_EDGE('',*,*,#15157,.F.) ;
#20669 = ORIENTED_EDGE('',*,*,#15620,.F.) ;
#20670 = ORIENTED_EDGE('',*,*,#15165,.F.) ;
#20671 = ORIENTED_EDGE('',*,*,#15630,.F.) ;
#20672 = ORIENTED_EDGE('',*,*,#14891,.F.) ;
#20673 = ORIENTED_EDGE('',*,*,#15389,.F.) ;
#20674 = ORIENTED_EDGE('',*,*,#15136,.F.) ;
#20675 = ORIENTED_EDGE('',*,*,#15631,.F.) ;
#20676 = ORIENTED_EDGE('',*,*,#14920,.F.) ;
#20677 = ORIENTED_EDGE('',*,*,#15632,.F.) ;
#20678 = ORIENTED_EDGE('',*,*,#14892,.F.) ;
#20679 = ORIENTED_EDGE('',*,*,#15630,.T.) ;
#20680 = ORIENTED_EDGE('',*,*,#15164,.F.) ;
#20681 = ORIENTED_EDGE('',*,*,#15624,.T.) ;
#20682 = ORIENTED_EDGE('',*,*,#15030,.F.) ;
#20683 = ORIENTED_EDGE('',*,*,#15633,.F.) ;
#20684 = ORIENTED_EDGE('',*,*,#15280,.F.) ;
#20685 = ORIENTED_EDGE('',*,*,#15618,.F.) ;
#20686 = ORIENTED_EDGE('',*,*,#14921,.F.) ;
#20687 = ORIENTED_EDGE('',*,*,#15631,.T.) ;
#20688 = ORIENTED_EDGE('',*,*,#15135,.F.) ;
#20689 = ORIENTED_EDGE('',*,*,#15633,.T.) ;
#20690 = ORIENTED_EDGE('',*,*,#15029,.F.) ;
#20691 = ORIENTED_EDGE('',*,*,#15634,.F.) ;
#20692 = ORIENTED_EDGE('',*,*,#15281,.F.) ;
#20693 = ORIENTED_EDGE('',*,*,#15614,.T.) ;
#20694 = ORIENTED_EDGE('',*,*,#15036,.F.) ;
#20695 = ORIENTED_EDGE('',*,*,#15627,.T.) ;
#20696 = ORIENTED_EDGE('',*,*,#15289,.F.) ;
#20697 = ORIENTED_EDGE('',*,*,#15632,.T.) ;
#20698 = ORIENTED_EDGE('',*,*,#15163,.F.) ;
#20699 = ORIENTED_EDGE('',*,*,#15635,.T.) ;
#20700 = ORIENTED_EDGE('',*,*,#14893,.F.) ;
#20701 = ORIENTED_EDGE('',*,*,#15426,.F.) ;
#20702 = ORIENTED_EDGE('',*,*,#15181,.F.) ;
#20703 = ORIENTED_EDGE('',*,*,#15636,.F.) ;
#20704 = ORIENTED_EDGE('',*,*,#14875,.F.) ;
#20705 = ORIENTED_EDGE('',*,*,#15479,.F.) ;
#20706 = ORIENTED_EDGE('',*,*,#14876,.F.) ;
#20707 = ORIENTED_EDGE('',*,*,#15636,.T.) ;
#20708 = ORIENTED_EDGE('',*,*,#15180,.F.) ;
#20709 = ORIENTED_EDGE('',*,*,#15524,.T.) ;
#20710 = ORIENTED_EDGE('',*,*,#15040,.F.) ;
#20711 = ORIENTED_EDGE('',*,*,#15537,.F.) ;
#20712 = ORIENTED_EDGE('',*,*,#15245,.F.) ;
#20713 = ORIENTED_EDGE('',*,*,#15635,.F.) ;
#20714 = ORIENTED_EDGE('',*,*,#15162,.F.) ;
#20715 = ORIENTED_EDGE('',*,*,#15637,.F.) ;
#20716 = ORIENTED_EDGE('',*,*,#14894,.F.) ;
#20717 = ORIENTED_EDGE('',*,*,#15638,.F.) ;
#20718 = ORIENTED_EDGE('',*,*,#14895,.F.) ;
#20719 = ORIENTED_EDGE('',*,*,#15637,.T.) ;
#20720 = ORIENTED_EDGE('',*,*,#15161,.F.) ;
#20721 = ORIENTED_EDGE('',*,*,#15638,.T.) ;
#20722 = ORIENTED_EDGE('',*,*,#15160,.F.) ;
#20723 = ORIENTED_EDGE('',*,*,#15639,.T.) ;
#20724 = ORIENTED_EDGE('',*,*,#14896,.F.) ;
#20725 = ORIENTED_EDGE('',*,*,#15634,.T.) ;
#20726 = ORIENTED_EDGE('',*,*,#15028,.F.) ;
#20727 = ORIENTED_EDGE('',*,*,#15628,.T.) ;
#20728 = ORIENTED_EDGE('',*,*,#15282,.F.) ;
#20729 = ORIENTED_EDGE('',*,*,#15432,.T.) ;
#20730 = ORIENTED_EDGE('',*,*,#15117,.F.) ;
#20731 = ORIENTED_EDGE('',*,*,#15121,.F.) ;
#20732 = ORIENTED_EDGE('',*,*,#15222,.F.) ;
#20733 = ORIENTED_EDGE('',*,*,#15639,.F.) ;
#20734 = ORIENTED_EDGE('',*,*,#15159,.F.) ;
#20735 = ORIENTED_EDGE('',*,*,#15640,.F.) ;
#20736 = ORIENTED_EDGE('',*,*,#14897,.F.) ;
#20737 = ORIENTED_EDGE('',*,*,#15454,.F.) ;
#20738 = ORIENTED_EDGE('',*,*,#15140,.F.) ;
#20739 = ORIENTED_EDGE('',*,*,#15641,.F.) ;
#20740 = ORIENTED_EDGE('',*,*,#14916,.F.) ;
#20741 = ORIENTED_EDGE('',*,*,#15629,.F.) ;
#20742 = ORIENTED_EDGE('',*,*,#14898,.F.) ;
#20743 = ORIENTED_EDGE('',*,*,#15640,.T.) ;
#20744 = ORIENTED_EDGE('',*,*,#15158,.F.) ;
#20745 = ORIENTED_EDGE('',*,*,#15590,.T.) ;
#20746 = ORIENTED_EDGE('',*,*,#15025,.F.) ;
#20747 = ORIENTED_EDGE('',*,*,#15605,.F.) ;
#20748 = ORIENTED_EDGE('',*,*,#15292,.F.) ;
#20749 = ORIENTED_EDGE('',*,*,#15388,.F.) ;
#20750 = ORIENTED_EDGE('',*,*,#14917,.F.) ;
#20751 = ORIENTED_EDGE('',*,*,#15641,.T.) ;
#20752 = ORIENTED_EDGE('',*,*,#15139,.F.) ;
#20753 = ORIENTED_EDGE('',*,*,#15642,.T.) ;
#20754 = ORIENTED_EDGE('',*,*,#15643,.T.) ;
#20755 = ORIENTED_EDGE('',*,*,#15644,.T.) ;
#20756 = ORIENTED_EDGE('',*,*,#15645,.T.) ;
#20757 = ORIENTED_EDGE('',*,*,#15646,.T.) ;
#20758 = ORIENTED_EDGE('',*,*,#15647,.T.) ;
#20759 = ORIENTED_EDGE('',*,*,#15648,.T.) ;
#20760 = ORIENTED_EDGE('',*,*,#15649,.T.) ;
#20761 = ORIENTED_EDGE('',*,*,#15650,.T.) ;
#20762 = ORIENTED_EDGE('',*,*,#15651,.T.) ;
#20763 = ORIENTED_EDGE('',*,*,#15652,.T.) ;
#20764 = ORIENTED_EDGE('',*,*,#15653,.T.) ;
#20765 = ORIENTED_EDGE('',*,*,#15654,.T.) ;
#20766 = ORIENTED_EDGE('',*,*,#15655,.T.) ;
#20767 = ORIENTED_EDGE('',*,*,#15656,.T.) ;
#20768 = ORIENTED_EDGE('',*,*,#15657,.T.) ;
#20769 = ORIENTED_EDGE('',*,*,#15658,.T.) ;
#20770 = ORIENTED_EDGE('',*,*,#15659,.T.) ;
#20771 = ORIENTED_EDGE('',*,*,#15660,.T.) ;
#20772 = ORIENTED_EDGE('',*,*,#15661,.T.) ;
#20773 = ORIENTED_EDGE('',*,*,#15662,.T.) ;
#20774 = ORIENTED_EDGE('',*,*,#15663,.T.) ;
#20775 = ORIENTED_EDGE('',*,*,#15664,.T.) ;
#20776 = ORIENTED_EDGE('',*,*,#15665,.T.) ;
#20777 = ORIENTED_EDGE('',*,*,#15666,.T.) ;
#20778 = ORIENTED_EDGE('',*,*,#15667,.T.) ;
#20779 = ORIENTED_EDGE('',*,*,#15668,.T.) ;
#20780 = ORIENTED_EDGE('',*,*,#15669,.T.) ;
#20781 = ORIENTED_EDGE('',*,*,#15670,.T.) ;
#20782 = ORIENTED_EDGE('',*,*,#15671,.T.) ;
#20783 = ORIENTED_EDGE('',*,*,#15672,.T.) ;
#20784 = ORIENTED_EDGE('',*,*,#15673,.T.) ;
#20785 = ORIENTED_EDGE('',*,*,#15674,.T.) ;
#20786 = ORIENTED_EDGE('',*,*,#15675,.T.) ;
#20787 = ORIENTED_EDGE('',*,*,#15676,.T.) ;
#20788 = ORIENTED_EDGE('',*,*,#15677,.T.) ;
#20789 = ORIENTED_EDGE('',*,*,#15678,.T.) ;
#20790 = ORIENTED_EDGE('',*,*,#15679,.T.) ;
#20791 = ORIENTED_EDGE('',*,*,#15680,.T.) ;
#20792 = ORIENTED_EDGE('',*,*,#15681,.T.) ;
#20793 = ORIENTED_EDGE('',*,*,#15682,.T.) ;
#20794 = ORIENTED_EDGE('',*,*,#15683,.T.) ;
#20795 = ORIENTED_EDGE('',*,*,#15684,.T.) ;
#20796 = ORIENTED_EDGE('',*,*,#15685,.T.) ;
#20797 = ORIENTED_EDGE('',*,*,#15686,.T.) ;
#20798 = ORIENTED_EDGE('',*,*,#15687,.T.) ;
#20799 = ORIENTED_EDGE('',*,*,#15688,.T.) ;
#20800 = ORIENTED_EDGE('',*,*,#15689,.T.) ;
#20801 = ORIENTED_EDGE('',*,*,#15690,.T.) ;
#20802 = ORIENTED_EDGE('',*,*,#15691,.T.) ;
#20803 = ORIENTED_EDGE('',*,*,#15692,.T.) ;
#20804 = ORIENTED_EDGE('',*,*,#15693,.T.) ;
#20805 = ORIENTED_EDGE('',*,*,#15694,.T.) ;
#20806 = ORIENTED_EDGE('',*,*,#15695,.T.) ;
#20807 = ORIENTED_EDGE('',*,*,#15696,.T.) ;
#20808 = ORIENTED_EDGE('',*,*,#15697,.T.) ;
#20809 = ORIENTED_EDGE('',*,*,#15698,.T.) ;
#20810 = ORIENTED_EDGE('',*,*,#15699,.T.) ;
#20811 = ORIENTED_EDGE('',*,*,#15700,.T.) ;
#20812 = ORIENTED_EDGE('',*,*,#15701,.T.) ;
#20813 = ORIENTED_EDGE('',*,*,#15702,.T.) ;
#20814 = ORIENTED_EDGE('',*,*,#15703,.T.) ;
#20815 = ORIENTED_EDGE('',*,*,#15704,.T.) ;
#20816 = ORIENTED_EDGE('',*,*,#15705,.T.) ;
#20817 = ORIENTED_EDGE('',*,*,#15706,.T.) ;
#20818 = ORIENTED_EDGE('',*,*,#15707,.T.) ;
#20819 = ORIENTED_EDGE('',*,*,#15708,.T.) ;
#20820 = ORIENTED_EDGE('',*,*,#15709,.T.) ;
#20821 = ORIENTED_EDGE('',*,*,#15710,.T.) ;
#20822 = ORIENTED_EDGE('',*,*,#15711,.T.) ;
#20823 = ORIENTED_EDGE('',*,*,#15712,.T.) ;
#20824 = ORIENTED_EDGE('',*,*,#15713,.T.) ;
#20825 = ORIENTED_EDGE('',*,*,#15714,.T.) ;
#20826 = ORIENTED_EDGE('',*,*,#15715,.T.) ;
#20827 = ORIENTED_EDGE('',*,*,#15716,.T.) ;
#20828 = ORIENTED_EDGE('',*,*,#15717,.T.) ;
#20829 = ORIENTED_EDGE('',*,*,#15718,.T.) ;
#20830 = ORIENTED_EDGE('',*,*,#15719,.T.) ;
#20831 = ORIENTED_EDGE('',*,*,#15720,.T.) ;
#20832 = ORIENTED_EDGE('',*,*,#15721,.T.) ;
#20833 = ORIENTED_EDGE('',*,*,#15722,.T.) ;
#20834 = ORIENTED_EDGE('',*,*,#15723,.T.) ;
#20835 = ORIENTED_EDGE('',*,*,#15724,.T.) ;
#20836 = ORIENTED_EDGE('',*,*,#15725,.T.) ;
#20837 = ORIENTED_EDGE('',*,*,#15726,.F.) ;
#20838 = ORIENTED_EDGE('',*,*,#15642,.F.) ;
#20839 = ORIENTED_EDGE('',*,*,#15727,.F.) ;
#20840 = ORIENTED_EDGE('',*,*,#15728,.T.) ;
#20841 = ORIENTED_EDGE('',*,*,#15729,.F.) ;
#20842 = ORIENTED_EDGE('',*,*,#15644,.F.) ;
#20843 = ORIENTED_EDGE('',*,*,#15730,.F.) ;
#20844 = ORIENTED_EDGE('',*,*,#15728,.F.) ;
#20845 = ORIENTED_EDGE('',*,*,#15729,.T.) ;
#20846 = ORIENTED_EDGE('',*,*,#15731,.T.) ;
#20847 = ORIENTED_EDGE('',*,*,#15732,.F.) ;
#20848 = ORIENTED_EDGE('',*,*,#15646,.F.) ;
#20849 = ORIENTED_EDGE('',*,*,#15733,.F.) ;
#20850 = ORIENTED_EDGE('',*,*,#15731,.F.) ;
#20851 = ORIENTED_EDGE('',*,*,#15730,.T.) ;
#20852 = ORIENTED_EDGE('',*,*,#15645,.F.) ;
#20853 = ORIENTED_EDGE('',*,*,#15732,.T.) ;
#20854 = ORIENTED_EDGE('',*,*,#15734,.T.) ;
#20855 = ORIENTED_EDGE('',*,*,#15735,.F.) ;
#20856 = ORIENTED_EDGE('',*,*,#15648,.F.) ;
#20857 = ORIENTED_EDGE('',*,*,#15736,.F.) ;
#20858 = ORIENTED_EDGE('',*,*,#15734,.F.) ;
#20859 = ORIENTED_EDGE('',*,*,#15733,.T.) ;
#20860 = ORIENTED_EDGE('',*,*,#15647,.F.) ;
#20861 = ORIENTED_EDGE('',*,*,#15735,.T.) ;
#20862 = ORIENTED_EDGE('',*,*,#15737,.T.) ;
#20863 = ORIENTED_EDGE('',*,*,#15738,.F.) ;
#20864 = ORIENTED_EDGE('',*,*,#15650,.F.) ;
#20865 = ORIENTED_EDGE('',*,*,#15739,.F.) ;
#20866 = ORIENTED_EDGE('',*,*,#15737,.F.) ;
#20867 = ORIENTED_EDGE('',*,*,#15736,.T.) ;
#20868 = ORIENTED_EDGE('',*,*,#15649,.F.) ;
#20869 = ORIENTED_EDGE('',*,*,#15738,.T.) ;
#20870 = ORIENTED_EDGE('',*,*,#15740,.T.) ;
#20871 = ORIENTED_EDGE('',*,*,#15741,.F.) ;
#20872 = ORIENTED_EDGE('',*,*,#15652,.F.) ;
#20873 = ORIENTED_EDGE('',*,*,#15742,.F.) ;
#20874 = ORIENTED_EDGE('',*,*,#15740,.F.) ;
#20875 = ORIENTED_EDGE('',*,*,#15739,.T.) ;
#20876 = ORIENTED_EDGE('',*,*,#15651,.F.) ;
#20877 = ORIENTED_EDGE('',*,*,#15741,.T.) ;
#20878 = ORIENTED_EDGE('',*,*,#15743,.T.) ;
#20879 = ORIENTED_EDGE('',*,*,#15744,.F.) ;
#20880 = ORIENTED_EDGE('',*,*,#15654,.F.) ;
#20881 = ORIENTED_EDGE('',*,*,#15745,.F.) ;
#20882 = ORIENTED_EDGE('',*,*,#15743,.F.) ;
#20883 = ORIENTED_EDGE('',*,*,#15742,.T.) ;
#20884 = ORIENTED_EDGE('',*,*,#15653,.F.) ;
#20885 = ORIENTED_EDGE('',*,*,#15744,.T.) ;
#20886 = ORIENTED_EDGE('',*,*,#15746,.T.) ;
#20887 = ORIENTED_EDGE('',*,*,#15747,.F.) ;
#20888 = ORIENTED_EDGE('',*,*,#15656,.F.) ;
#20889 = ORIENTED_EDGE('',*,*,#15748,.F.) ;
#20890 = ORIENTED_EDGE('',*,*,#15746,.F.) ;
#20891 = ORIENTED_EDGE('',*,*,#15745,.T.) ;
#20892 = ORIENTED_EDGE('',*,*,#15655,.F.) ;
#20893 = ORIENTED_EDGE('',*,*,#15747,.T.) ;
#20894 = ORIENTED_EDGE('',*,*,#15748,.T.) ;
#20895 = ORIENTED_EDGE('',*,*,#15658,.F.) ;
#20896 = ORIENTED_EDGE('',*,*,#15749,.T.) ;
#20897 = ORIENTED_EDGE('',*,*,#15659,.F.) ;
#20898 = ORIENTED_EDGE('',*,*,#15750,.F.) ;
#20899 = ORIENTED_EDGE('',*,*,#15660,.F.) ;
#20900 = ORIENTED_EDGE('',*,*,#15749,.F.) ;
#20901 = ORIENTED_EDGE('',*,*,#15657,.F.) ;
#20902 = ORIENTED_EDGE('',*,*,#15750,.T.) ;
#20903 = ORIENTED_EDGE('',*,*,#15662,.F.) ;
#20904 = ORIENTED_EDGE('',*,*,#15751,.T.) ;
#20905 = ORIENTED_EDGE('',*,*,#15663,.F.) ;
#20906 = ORIENTED_EDGE('',*,*,#15752,.F.) ;
#20907 = ORIENTED_EDGE('',*,*,#15664,.F.) ;
#20908 = ORIENTED_EDGE('',*,*,#15751,.F.) ;
#20909 = ORIENTED_EDGE('',*,*,#15661,.F.) ;
#20910 = ORIENTED_EDGE('',*,*,#15752,.T.) ;
#20911 = ORIENTED_EDGE('',*,*,#15666,.F.) ;
#20912 = ORIENTED_EDGE('',*,*,#15753,.T.) ;
#20913 = ORIENTED_EDGE('',*,*,#15667,.F.) ;
#20914 = ORIENTED_EDGE('',*,*,#15754,.F.) ;
#20915 = ORIENTED_EDGE('',*,*,#15668,.F.) ;
#20916 = ORIENTED_EDGE('',*,*,#15753,.F.) ;
#20917 = ORIENTED_EDGE('',*,*,#15665,.F.) ;
#20918 = ORIENTED_EDGE('',*,*,#15754,.T.) ;
#20919 = ORIENTED_EDGE('',*,*,#15670,.F.) ;
#20920 = ORIENTED_EDGE('',*,*,#15755,.T.) ;
#20921 = ORIENTED_EDGE('',*,*,#15671,.F.) ;
#20922 = ORIENTED_EDGE('',*,*,#15756,.F.) ;
#20923 = ORIENTED_EDGE('',*,*,#15672,.F.) ;
#20924 = ORIENTED_EDGE('',*,*,#15755,.F.) ;
#20925 = ORIENTED_EDGE('',*,*,#15669,.F.) ;
#20926 = ORIENTED_EDGE('',*,*,#15756,.T.) ;
#20927 = ORIENTED_EDGE('',*,*,#15674,.F.) ;
#20928 = ORIENTED_EDGE('',*,*,#15757,.T.) ;
#20929 = ORIENTED_EDGE('',*,*,#15675,.F.) ;
#20930 = ORIENTED_EDGE('',*,*,#15758,.F.) ;
#20931 = ORIENTED_EDGE('',*,*,#15676,.F.) ;
#20932 = ORIENTED_EDGE('',*,*,#15757,.F.) ;
#20933 = ORIENTED_EDGE('',*,*,#15673,.F.) ;
#20934 = ORIENTED_EDGE('',*,*,#15758,.T.) ;
#20935 = ORIENTED_EDGE('',*,*,#15678,.F.) ;
#20936 = ORIENTED_EDGE('',*,*,#15759,.T.) ;
#20937 = ORIENTED_EDGE('',*,*,#15679,.F.) ;
#20938 = ORIENTED_EDGE('',*,*,#15760,.F.) ;
#20939 = ORIENTED_EDGE('',*,*,#15680,.F.) ;
#20940 = ORIENTED_EDGE('',*,*,#15759,.F.) ;
#20941 = ORIENTED_EDGE('',*,*,#15677,.F.) ;
#20942 = ORIENTED_EDGE('',*,*,#15760,.T.) ;
#20943 = ORIENTED_EDGE('',*,*,#15682,.F.) ;
#20944 = ORIENTED_EDGE('',*,*,#15761,.T.) ;
#20945 = ORIENTED_EDGE('',*,*,#15683,.F.) ;
#20946 = ORIENTED_EDGE('',*,*,#15762,.F.) ;
#20947 = ORIENTED_EDGE('',*,*,#15684,.F.) ;
#20948 = ORIENTED_EDGE('',*,*,#15761,.F.) ;
#20949 = ORIENTED_EDGE('',*,*,#15681,.F.) ;
#20950 = ORIENTED_EDGE('',*,*,#15762,.T.) ;
#20951 = ORIENTED_EDGE('',*,*,#15686,.F.) ;
#20952 = ORIENTED_EDGE('',*,*,#15763,.T.) ;
#20953 = ORIENTED_EDGE('',*,*,#15687,.F.) ;
#20954 = ORIENTED_EDGE('',*,*,#15764,.F.) ;
#20955 = ORIENTED_EDGE('',*,*,#15688,.F.) ;
#20956 = ORIENTED_EDGE('',*,*,#15763,.F.) ;
#20957 = ORIENTED_EDGE('',*,*,#15685,.F.) ;
#20958 = ORIENTED_EDGE('',*,*,#15764,.T.) ;
#20959 = ORIENTED_EDGE('',*,*,#15690,.F.) ;
#20960 = ORIENTED_EDGE('',*,*,#15765,.T.) ;
#20961 = ORIENTED_EDGE('',*,*,#15691,.F.) ;
#20962 = ORIENTED_EDGE('',*,*,#15766,.F.) ;
#20963 = ORIENTED_EDGE('',*,*,#15692,.F.) ;
#20964 = ORIENTED_EDGE('',*,*,#15765,.F.) ;
#20965 = ORIENTED_EDGE('',*,*,#15689,.F.) ;
#20966 = ORIENTED_EDGE('',*,*,#15766,.T.) ;
#20967 = ORIENTED_EDGE('',*,*,#15694,.F.) ;
#20968 = ORIENTED_EDGE('',*,*,#15767,.T.) ;
#20969 = ORIENTED_EDGE('',*,*,#15695,.F.) ;
#20970 = ORIENTED_EDGE('',*,*,#15768,.F.) ;
#20971 = ORIENTED_EDGE('',*,*,#15696,.F.) ;
#20972 = ORIENTED_EDGE('',*,*,#15767,.F.) ;
#20973 = ORIENTED_EDGE('',*,*,#15693,.F.) ;
#20974 = ORIENTED_EDGE('',*,*,#15768,.T.) ;
#20975 = ORIENTED_EDGE('',*,*,#15698,.F.) ;
#20976 = ORIENTED_EDGE('',*,*,#15769,.T.) ;
#20977 = ORIENTED_EDGE('',*,*,#15699,.F.) ;
#20978 = ORIENTED_EDGE('',*,*,#15770,.F.) ;
#20979 = ORIENTED_EDGE('',*,*,#15700,.F.) ;
#20980 = ORIENTED_EDGE('',*,*,#15769,.F.) ;
#20981 = ORIENTED_EDGE('',*,*,#15697,.F.) ;
#20982 = ORIENTED_EDGE('',*,*,#15770,.T.) ;
#20983 = ORIENTED_EDGE('',*,*,#15702,.F.) ;
#20984 = ORIENTED_EDGE('',*,*,#15771,.T.) ;
#20985 = ORIENTED_EDGE('',*,*,#15703,.F.) ;
#20986 = ORIENTED_EDGE('',*,*,#15772,.F.) ;
#20987 = ORIENTED_EDGE('',*,*,#15704,.F.) ;
#20988 = ORIENTED_EDGE('',*,*,#15771,.F.) ;
#20989 = ORIENTED_EDGE('',*,*,#15701,.F.) ;
#20990 = ORIENTED_EDGE('',*,*,#15772,.T.) ;
#20991 = ORIENTED_EDGE('',*,*,#15706,.F.) ;
#20992 = ORIENTED_EDGE('',*,*,#15773,.T.) ;
#20993 = ORIENTED_EDGE('',*,*,#15707,.F.) ;
#20994 = ORIENTED_EDGE('',*,*,#15774,.F.) ;
#20995 = ORIENTED_EDGE('',*,*,#15708,.F.) ;
#20996 = ORIENTED_EDGE('',*,*,#15773,.F.) ;
#20997 = ORIENTED_EDGE('',*,*,#15705,.F.) ;
#20998 = ORIENTED_EDGE('',*,*,#15774,.T.) ;
#20999 = ORIENTED_EDGE('',*,*,#15710,.F.) ;
#21000 = ORIENTED_EDGE('',*,*,#15775,.T.) ;
#21001 = ORIENTED_EDGE('',*,*,#15711,.F.) ;
#21002 = ORIENTED_EDGE('',*,*,#15776,.F.) ;
#21003 = ORIENTED_EDGE('',*,*,#15777,.F.) ;
#21004 = ORIENTED_EDGE('',*,*,#15712,.F.) ;
#21005 = ORIENTED_EDGE('',*,*,#15775,.F.) ;
#21006 = ORIENTED_EDGE('',*,*,#15709,.F.) ;
#21007 = ORIENTED_EDGE('',*,*,#15777,.T.) ;
#21008 = ORIENTED_EDGE('',*,*,#15778,.T.) ;
#21009 = ORIENTED_EDGE('',*,*,#15779,.F.) ;
#21010 = ORIENTED_EDGE('',*,*,#15714,.F.) ;
#21011 = ORIENTED_EDGE('',*,*,#15780,.F.) ;
#21012 = ORIENTED_EDGE('',*,*,#15778,.F.) ;
#21013 = ORIENTED_EDGE('',*,*,#15776,.T.) ;
#21014 = ORIENTED_EDGE('',*,*,#15713,.F.) ;
#21015 = ORIENTED_EDGE('',*,*,#15779,.T.) ;
#21016 = ORIENTED_EDGE('',*,*,#15781,.T.) ;
#21017 = ORIENTED_EDGE('',*,*,#15782,.F.) ;
#21018 = ORIENTED_EDGE('',*,*,#15716,.F.) ;
#21019 = ORIENTED_EDGE('',*,*,#15783,.F.) ;
#21020 = ORIENTED_EDGE('',*,*,#15781,.F.) ;
#21021 = ORIENTED_EDGE('',*,*,#15780,.T.) ;
#21022 = ORIENTED_EDGE('',*,*,#15715,.F.) ;
#21023 = ORIENTED_EDGE('',*,*,#15782,.T.) ;
#21024 = ORIENTED_EDGE('',*,*,#15784,.T.) ;
#21025 = ORIENTED_EDGE('',*,*,#15785,.F.) ;
#21026 = ORIENTED_EDGE('',*,*,#15718,.F.) ;
#21027 = ORIENTED_EDGE('',*,*,#15786,.F.) ;
#21028 = ORIENTED_EDGE('',*,*,#15784,.F.) ;
#21029 = ORIENTED_EDGE('',*,*,#15783,.T.) ;
#21030 = ORIENTED_EDGE('',*,*,#15717,.F.) ;
#21031 = ORIENTED_EDGE('',*,*,#15785,.T.) ;
#21032 = ORIENTED_EDGE('',*,*,#15787,.T.) ;
#21033 = ORIENTED_EDGE('',*,*,#15788,.F.) ;
#21034 = ORIENTED_EDGE('',*,*,#15720,.F.) ;
#21035 = ORIENTED_EDGE('',*,*,#15789,.F.) ;
#21036 = ORIENTED_EDGE('',*,*,#15787,.F.) ;
#21037 = ORIENTED_EDGE('',*,*,#15786,.T.) ;
#21038 = ORIENTED_EDGE('',*,*,#15719,.F.) ;
#21039 = ORIENTED_EDGE('',*,*,#15788,.T.) ;
#21040 = ORIENTED_EDGE('',*,*,#15790,.T.) ;
#21041 = ORIENTED_EDGE('',*,*,#15791,.F.) ;
#21042 = ORIENTED_EDGE('',*,*,#15722,.F.) ;
#21043 = ORIENTED_EDGE('',*,*,#15792,.F.) ;
#21044 = ORIENTED_EDGE('',*,*,#15790,.F.) ;
#21045 = ORIENTED_EDGE('',*,*,#15789,.T.) ;
#21046 = ORIENTED_EDGE('',*,*,#15721,.F.) ;
#21047 = ORIENTED_EDGE('',*,*,#15791,.T.) ;
#21048 = ORIENTED_EDGE('',*,*,#15793,.T.) ;
#21049 = ORIENTED_EDGE('',*,*,#15794,.F.) ;
#21050 = ORIENTED_EDGE('',*,*,#15724,.F.) ;
#21051 = ORIENTED_EDGE('',*,*,#15795,.F.) ;
#21052 = ORIENTED_EDGE('',*,*,#15793,.F.) ;
#21053 = ORIENTED_EDGE('',*,*,#15792,.T.) ;
#21054 = ORIENTED_EDGE('',*,*,#15723,.F.) ;
#21055 = ORIENTED_EDGE('',*,*,#15794,.T.) ;
#21056 = ORIENTED_EDGE('',*,*,#15796,.T.) ;
#21057 = ORIENTED_EDGE('',*,*,#15727,.T.) ;
#21058 = ORIENTED_EDGE('',*,*,#15643,.F.) ;
#21059 = ORIENTED_EDGE('',*,*,#15726,.T.) ;
#21060 = ORIENTED_EDGE('',*,*,#15796,.F.) ;
#21061 = ORIENTED_EDGE('',*,*,#15795,.T.) ;
#21062 = ORIENTED_EDGE('',*,*,#15725,.F.) ;
#21063 = ORIENTED_EDGE('',*,*,#15797,.F.) ;
#21064 = ORIENTED_EDGE('',*,*,#15798,.T.) ;
#21065 = ORIENTED_EDGE('',*,*,#15799,.F.) ;
#21066 = ORIENTED_EDGE('',*,*,#15798,.F.) ;
#21067 = ORIENTED_EDGE('',*,*,#15800,.F.) ;
#21068 = ORIENTED_EDGE('',*,*,#15801,.T.) ;
#21069 = ORIENTED_EDGE('',*,*,#15802,.F.) ;
#21070 = ORIENTED_EDGE('',*,*,#15801,.F.) ;
#21071 = ORIENTED_EDGE('',*,*,#15803,.F.) ;
#21072 = ORIENTED_EDGE('',*,*,#15804,.T.) ;
#21073 = ORIENTED_EDGE('',*,*,#15805,.F.) ;
#21074 = ORIENTED_EDGE('',*,*,#15804,.F.) ;
#21075 = ORIENTED_EDGE('',*,*,#15806,.F.) ;
#21076 = ORIENTED_EDGE('',*,*,#15807,.T.) ;
#21077 = ORIENTED_EDGE('',*,*,#15808,.F.) ;
#21078 = ORIENTED_EDGE('',*,*,#15807,.F.) ;
#21079 = ORIENTED_EDGE('',*,*,#15809,.F.) ;
#21080 = ORIENTED_EDGE('',*,*,#15810,.T.) ;
#21081 = ORIENTED_EDGE('',*,*,#15811,.F.) ;
#21082 = ORIENTED_EDGE('',*,*,#15810,.F.) ;
#21083 = ORIENTED_EDGE('',*,*,#15812,.F.) ;
#21084 = ORIENTED_EDGE('',*,*,#15813,.T.) ;
#21085 = ORIENTED_EDGE('',*,*,#15814,.F.) ;
#21086 = ORIENTED_EDGE('',*,*,#15813,.F.) ;
#21087 = ORIENTED_EDGE('',*,*,#15815,.T.) ;
#21088 = ORIENTED_EDGE('',*,*,#15816,.T.) ;
#21089 = ORIENTED_EDGE('',*,*,#15817,.T.) ;
#21090 = ORIENTED_EDGE('',*,*,#15818,.T.) ;
#21091 = ORIENTED_EDGE('',*,*,#15819,.F.) ;
#21092 = ORIENTED_EDGE('',*,*,#15820,.T.) ;
#21093 = ORIENTED_EDGE('',*,*,#15821,.T.) ;
#21094 = ORIENTED_EDGE('',*,*,#15822,.T.) ;
#21095 = ORIENTED_EDGE('',*,*,#15818,.F.) ;
#21096 = ORIENTED_EDGE('',*,*,#15823,.T.) ;
#21097 = ORIENTED_EDGE('',*,*,#15821,.F.) ;
#21098 = ORIENTED_EDGE('',*,*,#15824,.T.) ;
#21099 = ORIENTED_EDGE('',*,*,#15825,.T.) ;
#21100 = ORIENTED_EDGE('',*,*,#15826,.T.) ;
#21101 = ORIENTED_EDGE('',*,*,#15825,.F.) ;
#21102 = ORIENTED_EDGE('',*,*,#15827,.T.) ;
#21103 = ORIENTED_EDGE('',*,*,#15828,.T.) ;
#21104 = ORIENTED_EDGE('',*,*,#15829,.T.) ;
#21105 = ORIENTED_EDGE('',*,*,#15817,.F.) ;
#21106 = ORIENTED_EDGE('',*,*,#15830,.F.) ;
#21107 = ORIENTED_EDGE('',*,*,#15822,.F.) ;
#21108 = ORIENTED_EDGE('',*,*,#15823,.F.) ;
#21109 = ORIENTED_EDGE('',*,*,#15802,.T.) ;
#21110 = ORIENTED_EDGE('',*,*,#15814,.T.) ;
#21111 = ORIENTED_EDGE('',*,*,#15820,.F.) ;
#21112 = ORIENTED_EDGE('',*,*,#15831,.F.) ;
#21113 = ORIENTED_EDGE('',*,*,#15827,.F.) ;
#21114 = ORIENTED_EDGE('',*,*,#15824,.F.) ;
#21115 = ORIENTED_EDGE('',*,*,#15797,.T.) ;
#21116 = ORIENTED_EDGE('',*,*,#15809,.T.) ;
#21117 = ORIENTED_EDGE('',*,*,#15815,.F.) ;
#21118 = ORIENTED_EDGE('',*,*,#15826,.F.) ;
#21119 = ORIENTED_EDGE('',*,*,#15829,.F.) ;
#21120 = ORIENTED_EDGE('',*,*,#15832,.F.) ;
#21121 = ORIENTED_EDGE('',*,*,#15816,.F.) ;
#21122 = ORIENTED_EDGE('',*,*,#15832,.T.) ;
#21123 = ORIENTED_EDGE('',*,*,#15828,.F.) ;
#21124 = ORIENTED_EDGE('',*,*,#15831,.T.) ;
#21125 = ORIENTED_EDGE('',*,*,#15819,.T.) ;
#21126 = ORIENTED_EDGE('',*,*,#15830,.T.) ;
#21127 = ORIENTED_EDGE('',*,*,#15833,.F.) ;
#21128 = ORIENTED_EDGE('',*,*,#15834,.T.) ;
#21129 = ORIENTED_EDGE('',*,*,#15835,.F.) ;
#21130 = ORIENTED_EDGE('',*,*,#15834,.F.) ;
#21131 = ORIENTED_EDGE('',*,*,#15836,.F.) ;
#21132 = ORIENTED_EDGE('',*,*,#15837,.T.) ;
#21133 = ORIENTED_EDGE('',*,*,#15838,.F.) ;
#21134 = ORIENTED_EDGE('',*,*,#15837,.F.) ;
#21135 = ORIENTED_EDGE('',*,*,#15839,.T.) ;
#21136 = ORIENTED_EDGE('',*,*,#15840,.T.) ;
#21137 = ORIENTED_EDGE('',*,*,#15841,.T.) ;
#21138 = ORIENTED_EDGE('',*,*,#15842,.T.) ;
#21139 = ORIENTED_EDGE('',*,*,#15843,.F.) ;
#21140 = ORIENTED_EDGE('',*,*,#15844,.T.) ;
#21141 = ORIENTED_EDGE('',*,*,#15845,.T.) ;
#21142 = ORIENTED_EDGE('',*,*,#15846,.T.) ;
#21143 = ORIENTED_EDGE('',*,*,#15842,.F.) ;
#21144 = ORIENTED_EDGE('',*,*,#15847,.T.) ;
#21145 = ORIENTED_EDGE('',*,*,#15845,.F.) ;
#21146 = ORIENTED_EDGE('',*,*,#15848,.T.) ;
#21147 = ORIENTED_EDGE('',*,*,#15849,.T.) ;
#21148 = ORIENTED_EDGE('',*,*,#15850,.T.) ;
#21149 = ORIENTED_EDGE('',*,*,#15849,.F.) ;
#21150 = ORIENTED_EDGE('',*,*,#15851,.T.) ;
#21151 = ORIENTED_EDGE('',*,*,#15852,.T.) ;
#21152 = ORIENTED_EDGE('',*,*,#15853,.T.) ;
#21153 = ORIENTED_EDGE('',*,*,#15841,.F.) ;
#21154 = ORIENTED_EDGE('',*,*,#15854,.F.) ;
#21155 = ORIENTED_EDGE('',*,*,#15846,.F.) ;
#21156 = ORIENTED_EDGE('',*,*,#15847,.F.) ;
#21157 = ORIENTED_EDGE('',*,*,#15808,.T.) ;
#21158 = ORIENTED_EDGE('',*,*,#15838,.T.) ;
#21159 = ORIENTED_EDGE('',*,*,#15844,.F.) ;
#21160 = ORIENTED_EDGE('',*,*,#15855,.F.) ;
#21161 = ORIENTED_EDGE('',*,*,#15851,.F.) ;
#21162 = ORIENTED_EDGE('',*,*,#15848,.F.) ;
#21163 = ORIENTED_EDGE('',*,*,#15803,.T.) ;
#21164 = ORIENTED_EDGE('',*,*,#15833,.T.) ;
#21165 = ORIENTED_EDGE('',*,*,#15839,.F.) ;
#21166 = ORIENTED_EDGE('',*,*,#15850,.F.) ;
#21167 = ORIENTED_EDGE('',*,*,#15853,.F.) ;
#21168 = ORIENTED_EDGE('',*,*,#15856,.F.) ;
#21169 = ORIENTED_EDGE('',*,*,#15840,.F.) ;
#21170 = ORIENTED_EDGE('',*,*,#15856,.T.) ;
#21171 = ORIENTED_EDGE('',*,*,#15852,.F.) ;
#21172 = ORIENTED_EDGE('',*,*,#15855,.T.) ;
#21173 = ORIENTED_EDGE('',*,*,#15843,.T.) ;
#21174 = ORIENTED_EDGE('',*,*,#15854,.T.) ;
#21175 = ORIENTED_EDGE('',*,*,#15857,.F.) ;
#21176 = ORIENTED_EDGE('',*,*,#15858,.T.) ;
#21177 = ORIENTED_EDGE('',*,*,#15859,.F.) ;
#21178 = ORIENTED_EDGE('',*,*,#15858,.F.) ;
#21179 = ORIENTED_EDGE('',*,*,#15860,.F.) ;
#21180 = ORIENTED_EDGE('',*,*,#15861,.T.) ;
#21181 = ORIENTED_EDGE('',*,*,#15862,.F.) ;
#21182 = ORIENTED_EDGE('',*,*,#15861,.F.) ;
#21183 = ORIENTED_EDGE('',*,*,#15863,.F.) ;
#21184 = ORIENTED_EDGE('',*,*,#15864,.T.) ;
#21185 = ORIENTED_EDGE('',*,*,#15865,.F.) ;
#21186 = ORIENTED_EDGE('',*,*,#15864,.F.) ;
#21187 = ORIENTED_EDGE('',*,*,#15866,.F.) ;
#21188 = ORIENTED_EDGE('',*,*,#15867,.T.) ;
#21189 = ORIENTED_EDGE('',*,*,#15868,.F.) ;
#21190 = ORIENTED_EDGE('',*,*,#15867,.F.) ;
#21191 = ORIENTED_EDGE('',*,*,#15866,.T.) ;
#21192 = ORIENTED_EDGE('',*,*,#15865,.T.) ;
#21193 = ORIENTED_EDGE('',*,*,#15869,.T.) ;
#21194 = ORIENTED_EDGE('',*,*,#15870,.T.) ;
#21195 = ORIENTED_EDGE('',*,*,#15871,.T.) ;
#21196 = ORIENTED_EDGE('',*,*,#15872,.F.) ;
#21197 = ORIENTED_EDGE('',*,*,#15873,.T.) ;
#21198 = ORIENTED_EDGE('',*,*,#15799,.T.) ;
#21199 = ORIENTED_EDGE('',*,*,#15811,.T.) ;
#21200 = ORIENTED_EDGE('',*,*,#15874,.T.) ;
#21201 = ORIENTED_EDGE('',*,*,#15868,.T.) ;
#21202 = ORIENTED_EDGE('',*,*,#15875,.F.) ;
#21203 = ORIENTED_EDGE('',*,*,#15876,.T.) ;
#21204 = ORIENTED_EDGE('',*,*,#15877,.F.) ;
#21205 = ORIENTED_EDGE('',*,*,#15876,.F.) ;
#21206 = ORIENTED_EDGE('',*,*,#15878,.F.) ;
#21207 = ORIENTED_EDGE('',*,*,#15879,.T.) ;
#21208 = ORIENTED_EDGE('',*,*,#15874,.F.) ;
#21209 = ORIENTED_EDGE('',*,*,#15879,.F.) ;
#21210 = ORIENTED_EDGE('',*,*,#15878,.T.) ;
#21211 = ORIENTED_EDGE('',*,*,#15877,.T.) ;
#21212 = ORIENTED_EDGE('',*,*,#15863,.T.) ;
#21213 = ORIENTED_EDGE('',*,*,#15880,.F.) ;
#21214 = ORIENTED_EDGE('',*,*,#15881,.T.) ;
#21215 = ORIENTED_EDGE('',*,*,#15882,.F.) ;
#21216 = ORIENTED_EDGE('',*,*,#15883,.F.) ;
#21217 = ORIENTED_EDGE('',*,*,#15884,.F.) ;
#21218 = ORIENTED_EDGE('',*,*,#15883,.T.) ;
#21219 = ORIENTED_EDGE('',*,*,#15885,.F.) ;
#21220 = ORIENTED_EDGE('',*,*,#15886,.F.) ;
#21221 = ORIENTED_EDGE('',*,*,#15887,.F.) ;
#21222 = ORIENTED_EDGE('',*,*,#15886,.T.) ;
#21223 = ORIENTED_EDGE('',*,*,#15888,.F.) ;
#21224 = ORIENTED_EDGE('',*,*,#15889,.F.) ;
#21225 = ORIENTED_EDGE('',*,*,#15890,.F.) ;
#21226 = ORIENTED_EDGE('',*,*,#15889,.T.) ;
#21227 = ORIENTED_EDGE('',*,*,#15891,.F.) ;
#21228 = ORIENTED_EDGE('',*,*,#15881,.F.) ;
#21229 = ORIENTED_EDGE('',*,*,#15892,.T.) ;
#21230 = ORIENTED_EDGE('',*,*,#15893,.T.) ;
#21231 = ORIENTED_EDGE('',*,*,#15894,.T.) ;
#21232 = ORIENTED_EDGE('',*,*,#15895,.T.) ;
#21233 = ORIENTED_EDGE('',*,*,#15888,.T.) ;
#21234 = ORIENTED_EDGE('',*,*,#15885,.T.) ;
#21235 = ORIENTED_EDGE('',*,*,#15882,.T.) ;
#21236 = ORIENTED_EDGE('',*,*,#15891,.T.) ;
#21237 = ORIENTED_EDGE('',*,*,#15896,.T.) ;
#21238 = ORIENTED_EDGE('',*,*,#15894,.F.) ;
#21239 = ORIENTED_EDGE('',*,*,#15897,.F.) ;
#21240 = ORIENTED_EDGE('',*,*,#15898,.F.) ;
#21241 = ORIENTED_EDGE('',*,*,#15899,.T.) ;
#21242 = ORIENTED_EDGE('',*,*,#15892,.F.) ;
#21243 = ORIENTED_EDGE('',*,*,#15900,.F.) ;
#21244 = ORIENTED_EDGE('',*,*,#15901,.F.) ;
#21245 = ORIENTED_EDGE('',*,*,#15898,.T.) ;
#21246 = ORIENTED_EDGE('',*,*,#15902,.T.) ;
#21247 = ORIENTED_EDGE('',*,*,#15903,.F.) ;
#21248 = ORIENTED_EDGE('',*,*,#15904,.F.) ;
#21249 = ORIENTED_EDGE('',*,*,#15905,.T.) ;
#21250 = ORIENTED_EDGE('',*,*,#15800,.T.) ;
#21251 = ORIENTED_EDGE('',*,*,#15812,.T.) ;
#21252 = ORIENTED_EDGE('',*,*,#15880,.T.) ;
#21253 = ORIENTED_EDGE('',*,*,#15884,.T.) ;
#21254 = ORIENTED_EDGE('',*,*,#15887,.T.) ;
#21255 = ORIENTED_EDGE('',*,*,#15890,.T.) ;
#21256 = ORIENTED_EDGE('',*,*,#15906,.F.) ;
#21257 = ORIENTED_EDGE('',*,*,#15907,.T.) ;
#21258 = ORIENTED_EDGE('',*,*,#15908,.T.) ;
#21259 = ORIENTED_EDGE('',*,*,#15909,.F.) ;
#21260 = ORIENTED_EDGE('',*,*,#15910,.T.) ;
#21261 = ORIENTED_EDGE('',*,*,#15911,.T.) ;
#21262 = ORIENTED_EDGE('',*,*,#15912,.T.) ;
#21263 = ORIENTED_EDGE('',*,*,#15913,.T.) ;
#21264 = ORIENTED_EDGE('',*,*,#15914,.T.) ;
#21265 = ORIENTED_EDGE('',*,*,#15915,.F.) ;
#21266 = ORIENTED_EDGE('',*,*,#15916,.F.) ;
#21267 = ORIENTED_EDGE('',*,*,#15917,.T.) ;
#21268 = ORIENTED_EDGE('',*,*,#15918,.F.) ;
#21269 = ORIENTED_EDGE('',*,*,#15919,.F.) ;
#21270 = ORIENTED_EDGE('',*,*,#15914,.F.) ;
#21271 = ORIENTED_EDGE('',*,*,#15920,.F.) ;
#21272 = ORIENTED_EDGE('',*,*,#15921,.F.) ;
#21273 = ORIENTED_EDGE('',*,*,#15922,.T.) ;
#21274 = ORIENTED_EDGE('',*,*,#15907,.F.) ;
#21275 = ORIENTED_EDGE('',*,*,#15923,.F.) ;
#21276 = ORIENTED_EDGE('',*,*,#15924,.F.) ;
#21277 = ORIENTED_EDGE('',*,*,#15925,.T.) ;
#21278 = ORIENTED_EDGE('',*,*,#15912,.F.) ;
#21279 = ORIENTED_EDGE('',*,*,#15926,.T.) ;
#21280 = ORIENTED_EDGE('',*,*,#15927,.F.) ;
#21281 = ORIENTED_EDGE('',*,*,#15928,.F.) ;
#21282 = ORIENTED_EDGE('',*,*,#15929,.F.) ;
#21283 = ORIENTED_EDGE('',*,*,#15920,.T.) ;
#21284 = ORIENTED_EDGE('',*,*,#15913,.F.) ;
#21285 = ORIENTED_EDGE('',*,*,#15925,.F.) ;
#21286 = ORIENTED_EDGE('',*,*,#15930,.F.) ;
#21287 = ORIENTED_EDGE('',*,*,#15931,.T.) ;
#21288 = ORIENTED_EDGE('',*,*,#15932,.T.) ;
#21289 = ORIENTED_EDGE('',*,*,#15933,.T.) ;
#21290 = ORIENTED_EDGE('',*,*,#15934,.F.) ;
#21291 = ORIENTED_EDGE('',*,*,#15909,.T.) ;
#21292 = ORIENTED_EDGE('',*,*,#15935,.T.) ;
#21293 = ORIENTED_EDGE('',*,*,#15936,.T.) ;
#21294 = ORIENTED_EDGE('',*,*,#15937,.T.) ;
#21295 = ORIENTED_EDGE('',*,*,#15933,.F.) ;
#21296 = ORIENTED_EDGE('',*,*,#15938,.F.) ;
#21297 = ORIENTED_EDGE('',*,*,#15939,.F.) ;
#21298 = ORIENTED_EDGE('',*,*,#15940,.T.) ;
#21299 = ORIENTED_EDGE('',*,*,#15941,.F.) ;
#21300 = ORIENTED_EDGE('',*,*,#15942,.F.) ;
#21301 = ORIENTED_EDGE('',*,*,#15943,.F.) ;
#21302 = ORIENTED_EDGE('',*,*,#15944,.F.) ;
#21303 = ORIENTED_EDGE('',*,*,#15945,.F.) ;
#21304 = ORIENTED_EDGE('',*,*,#15946,.F.) ;
#21305 = ORIENTED_EDGE('',*,*,#15947,.F.) ;
#21306 = ORIENTED_EDGE('',*,*,#15948,.F.) ;
#21307 = ORIENTED_EDGE('',*,*,#15949,.F.) ;
#21308 = ORIENTED_EDGE('',*,*,#15950,.T.) ;
#21309 = ORIENTED_EDGE('',*,*,#15951,.F.) ;
#21310 = ORIENTED_EDGE('',*,*,#15952,.T.) ;
#21311 = ORIENTED_EDGE('',*,*,#15936,.F.) ;
#21312 = ORIENTED_EDGE('',*,*,#15953,.T.) ;
#21313 = ORIENTED_EDGE('',*,*,#15954,.F.) ;
#21314 = ORIENTED_EDGE('',*,*,#15955,.F.) ;
#21315 = ORIENTED_EDGE('',*,*,#15956,.F.) ;
#21316 = ORIENTED_EDGE('',*,*,#15957,.F.) ;
#21317 = ORIENTED_EDGE('',*,*,#15958,.T.) ;
#21318 = ORIENTED_EDGE('',*,*,#15959,.T.) ;
#21319 = ORIENTED_EDGE('',*,*,#15960,.T.) ;
#21320 = ORIENTED_EDGE('',*,*,#15961,.F.) ;
#21321 = ORIENTED_EDGE('',*,*,#15962,.F.) ;
#21322 = ORIENTED_EDGE('',*,*,#15963,.T.) ;
#21323 = ORIENTED_EDGE('',*,*,#15964,.T.) ;
#21324 = ORIENTED_EDGE('',*,*,#15965,.F.) ;
#21325 = ORIENTED_EDGE('',*,*,#15966,.T.) ;
#21326 = ORIENTED_EDGE('',*,*,#15967,.T.) ;
#21327 = ORIENTED_EDGE('',*,*,#15968,.T.) ;
#21328 = ORIENTED_EDGE('',*,*,#15969,.F.) ;
#21329 = ORIENTED_EDGE('',*,*,#15956,.T.) ;
#21330 = ORIENTED_EDGE('',*,*,#15962,.T.) ;
#21331 = ORIENTED_EDGE('',*,*,#15970,.F.) ;
#21332 = ORIENTED_EDGE('',*,*,#15971,.F.) ;
#21333 = ORIENTED_EDGE('',*,*,#15952,.F.) ;
#21334 = ORIENTED_EDGE('',*,*,#15972,.T.) ;
#21335 = ORIENTED_EDGE('',*,*,#15973,.F.) ;
#21336 = ORIENTED_EDGE('',*,*,#15974,.F.) ;
#21337 = ORIENTED_EDGE('',*,*,#15975,.F.) ;
#21338 = ORIENTED_EDGE('',*,*,#15976,.F.) ;
#21339 = ORIENTED_EDGE('',*,*,#15977,.T.) ;
#21340 = ORIENTED_EDGE('',*,*,#15978,.T.) ;
#21341 = ORIENTED_EDGE('',*,*,#15979,.F.) ;
#21342 = ORIENTED_EDGE('',*,*,#15980,.F.) ;
#21343 = ORIENTED_EDGE('',*,*,#15981,.T.) ;
#21344 = ORIENTED_EDGE('',*,*,#15871,.F.) ;
#21345 = ORIENTED_EDGE('',*,*,#15982,.T.) ;
#21346 = ORIENTED_EDGE('',*,*,#15983,.F.) ;
#21347 = ORIENTED_EDGE('',*,*,#15984,.T.) ;
#21348 = ORIENTED_EDGE('',*,*,#15953,.F.) ;
#21349 = ORIENTED_EDGE('',*,*,#15935,.F.) ;
#21350 = ORIENTED_EDGE('',*,*,#15908,.F.) ;
#21351 = ORIENTED_EDGE('',*,*,#15922,.F.) ;
#21352 = ORIENTED_EDGE('',*,*,#15985,.F.) ;
#21353 = ORIENTED_EDGE('',*,*,#15986,.T.) ;
#21354 = ORIENTED_EDGE('',*,*,#15987,.F.) ;
#21355 = ORIENTED_EDGE('',*,*,#15988,.F.) ;
#21356 = ORIENTED_EDGE('',*,*,#15975,.T.) ;
#21357 = ORIENTED_EDGE('',*,*,#15949,.T.) ;
#21358 = ORIENTED_EDGE('',*,*,#15971,.T.) ;
#21359 = ORIENTED_EDGE('',*,*,#15989,.F.) ;
#21360 = ORIENTED_EDGE('',*,*,#15990,.F.) ;
#21361 = ORIENTED_EDGE('',*,*,#15951,.T.) ;
#21362 = ORIENTED_EDGE('',*,*,#15991,.T.) ;
#21363 = ORIENTED_EDGE('',*,*,#15992,.F.) ;
#21364 = ORIENTED_EDGE('',*,*,#15972,.F.) ;
#21365 = ORIENTED_EDGE('',*,*,#15948,.T.) ;
#21366 = ORIENTED_EDGE('',*,*,#15993,.T.) ;
#21367 = ORIENTED_EDGE('',*,*,#15994,.F.) ;
#21368 = ORIENTED_EDGE('',*,*,#15995,.F.) ;
#21369 = ORIENTED_EDGE('',*,*,#15945,.T.) ;
#21370 = ORIENTED_EDGE('',*,*,#15995,.T.) ;
#21371 = ORIENTED_EDGE('',*,*,#15996,.F.) ;
#21372 = ORIENTED_EDGE('',*,*,#15997,.F.) ;
#21373 = ORIENTED_EDGE('',*,*,#15944,.T.) ;
#21374 = ORIENTED_EDGE('',*,*,#15998,.T.) ;
#21375 = ORIENTED_EDGE('',*,*,#15999,.F.) ;
#21376 = ORIENTED_EDGE('',*,*,#16000,.F.) ;
#21377 = ORIENTED_EDGE('',*,*,#15941,.T.) ;
#21378 = ORIENTED_EDGE('',*,*,#16000,.T.) ;
#21379 = ORIENTED_EDGE('',*,*,#16001,.F.) ;
#21380 = ORIENTED_EDGE('',*,*,#16002,.F.) ;
#21381 = ORIENTED_EDGE('',*,*,#16003,.T.) ;
#21382 = ORIENTED_EDGE('',*,*,#15989,.T.) ;
#21383 = ORIENTED_EDGE('',*,*,#15970,.T.) ;
#21384 = ORIENTED_EDGE('',*,*,#15961,.T.) ;
#21385 = ORIENTED_EDGE('',*,*,#16004,.T.) ;
#21386 = ORIENTED_EDGE('',*,*,#16005,.T.) ;
#21387 = ORIENTED_EDGE('',*,*,#15996,.T.) ;
#21388 = ORIENTED_EDGE('',*,*,#15994,.T.) ;
#21389 = ORIENTED_EDGE('',*,*,#16006,.T.) ;
#21390 = ORIENTED_EDGE('',*,*,#16007,.T.) ;
#21391 = ORIENTED_EDGE('',*,*,#15957,.T.) ;
#21392 = ORIENTED_EDGE('',*,*,#15969,.T.) ;
#21393 = ORIENTED_EDGE('',*,*,#16008,.T.) ;
#21394 = ORIENTED_EDGE('',*,*,#16009,.T.) ;
#21395 = ORIENTED_EDGE('',*,*,#16010,.T.) ;
#21396 = ORIENTED_EDGE('',*,*,#16011,.T.) ;
#21397 = ORIENTED_EDGE('',*,*,#15973,.T.) ;
#21398 = ORIENTED_EDGE('',*,*,#15992,.T.) ;
#21399 = ORIENTED_EDGE('',*,*,#16012,.T.) ;
#21400 = ORIENTED_EDGE('',*,*,#16013,.T.) ;
#21401 = ORIENTED_EDGE('',*,*,#16001,.T.) ;
#21402 = ORIENTED_EDGE('',*,*,#15999,.T.) ;
#21403 = ORIENTED_EDGE('',*,*,#16014,.F.) ;
#21404 = ORIENTED_EDGE('',*,*,#16015,.T.) ;
#21405 = ORIENTED_EDGE('',*,*,#16016,.F.) ;
#21406 = ORIENTED_EDGE('',*,*,#15980,.T.) ;
#21407 = ORIENTED_EDGE('',*,*,#16017,.T.) ;
#21408 = ORIENTED_EDGE('',*,*,#16018,.F.) ;
#21409 = ORIENTED_EDGE('',*,*,#16014,.T.) ;
#21410 = ORIENTED_EDGE('',*,*,#15979,.T.) ;
#21411 = ORIENTED_EDGE('',*,*,#15974,.T.) ;
#21412 = ORIENTED_EDGE('',*,*,#16011,.F.) ;
#21413 = ORIENTED_EDGE('',*,*,#16019,.F.) ;
#21414 = ORIENTED_EDGE('',*,*,#16020,.T.) ;
#21415 = ORIENTED_EDGE('',*,*,#15947,.T.) ;
#21416 = ORIENTED_EDGE('',*,*,#16021,.T.) ;
#21417 = ORIENTED_EDGE('',*,*,#16004,.F.) ;
#21418 = ORIENTED_EDGE('',*,*,#15993,.F.) ;
#21419 = ORIENTED_EDGE('',*,*,#15946,.T.) ;
#21420 = ORIENTED_EDGE('',*,*,#15997,.T.) ;
#21421 = ORIENTED_EDGE('',*,*,#16005,.F.) ;
#21422 = ORIENTED_EDGE('',*,*,#16021,.F.) ;
#21423 = ORIENTED_EDGE('',*,*,#15943,.T.) ;
#21424 = ORIENTED_EDGE('',*,*,#16022,.T.) ;
#21425 = ORIENTED_EDGE('',*,*,#16012,.F.) ;
#21426 = ORIENTED_EDGE('',*,*,#15998,.F.) ;
#21427 = ORIENTED_EDGE('',*,*,#15942,.T.) ;
#21428 = ORIENTED_EDGE('',*,*,#16002,.T.) ;
#21429 = ORIENTED_EDGE('',*,*,#16013,.F.) ;
#21430 = ORIENTED_EDGE('',*,*,#16022,.F.) ;
#21431 = ORIENTED_EDGE('',*,*,#16023,.T.) ;
#21432 = ORIENTED_EDGE('',*,*,#16024,.T.) ;
#21433 = ORIENTED_EDGE('',*,*,#16025,.T.) ;
#21434 = ORIENTED_EDGE('',*,*,#16026,.T.) ;
#21435 = ORIENTED_EDGE('',*,*,#15986,.F.) ;
#21436 = ORIENTED_EDGE('',*,*,#16027,.T.) ;
#21437 = ORIENTED_EDGE('',*,*,#16025,.F.) ;
#21438 = ORIENTED_EDGE('',*,*,#16027,.F.) ;
#21439 = ORIENTED_EDGE('',*,*,#16020,.F.) ;
#21440 = ORIENTED_EDGE('',*,*,#16023,.F.) ;
#21441 = ORIENTED_EDGE('',*,*,#16028,.T.) ;
#21442 = ORIENTED_EDGE('',*,*,#15959,.F.) ;
#21443 = ORIENTED_EDGE('',*,*,#15963,.F.) ;
#21444 = ORIENTED_EDGE('',*,*,#16028,.F.) ;
#21445 = ORIENTED_EDGE('',*,*,#16026,.F.) ;
#21446 = ORIENTED_EDGE('',*,*,#16029,.T.) ;
#21447 = ORIENTED_EDGE('',*,*,#16009,.F.) ;
#21448 = ORIENTED_EDGE('',*,*,#16029,.F.) ;
#21449 = ORIENTED_EDGE('',*,*,#16008,.F.) ;
#21450 = ORIENTED_EDGE('',*,*,#16030,.T.) ;
#21451 = ORIENTED_EDGE('',*,*,#16024,.F.) ;
#21452 = ORIENTED_EDGE('',*,*,#16030,.F.) ;
#21453 = ORIENTED_EDGE('',*,*,#16031,.T.) ;
#21454 = ORIENTED_EDGE('',*,*,#16032,.T.) ;
#21455 = ORIENTED_EDGE('',*,*,#16033,.T.) ;
#21456 = ORIENTED_EDGE('',*,*,#15965,.T.) ;
#21457 = ORIENTED_EDGE('',*,*,#16034,.T.) ;
#21458 = ORIENTED_EDGE('',*,*,#16035,.F.) ;
#21459 = ORIENTED_EDGE('',*,*,#16036,.F.) ;
#21460 = ORIENTED_EDGE('',*,*,#16037,.F.) ;
#21461 = ORIENTED_EDGE('',*,*,#16038,.T.) ;
#21462 = ORIENTED_EDGE('',*,*,#16039,.F.) ;
#21463 = ORIENTED_EDGE('',*,*,#16040,.F.) ;
#21464 = ORIENTED_EDGE('',*,*,#16041,.F.) ;
#21465 = ORIENTED_EDGE('',*,*,#16037,.T.) ;
#21466 = ORIENTED_EDGE('',*,*,#16042,.T.) ;
#21467 = ORIENTED_EDGE('',*,*,#16041,.T.) ;
#21468 = ORIENTED_EDGE('',*,*,#16043,.T.) ;
#21469 = ORIENTED_EDGE('',*,*,#16044,.F.) ;
#21470 = ORIENTED_EDGE('',*,*,#16045,.T.) ;
#21471 = ORIENTED_EDGE('',*,*,#16035,.T.) ;
#21472 = ORIENTED_EDGE('',*,*,#16046,.T.) ;
#21473 = ORIENTED_EDGE('',*,*,#15967,.F.) ;
#21474 = ORIENTED_EDGE('',*,*,#16047,.T.) ;
#21475 = ORIENTED_EDGE('',*,*,#16039,.T.) ;
#21476 = ORIENTED_EDGE('',*,*,#16048,.T.) ;
#21477 = ORIENTED_EDGE('',*,*,#16049,.F.) ;
#21478 = ORIENTED_EDGE('',*,*,#16046,.F.) ;
#21479 = ORIENTED_EDGE('',*,*,#16034,.F.) ;
#21480 = ORIENTED_EDGE('',*,*,#16043,.F.) ;
#21481 = ORIENTED_EDGE('',*,*,#16040,.T.) ;
#21482 = ORIENTED_EDGE('',*,*,#16047,.F.) ;
#21483 = ORIENTED_EDGE('',*,*,#15966,.F.) ;
#21484 = ORIENTED_EDGE('',*,*,#16033,.F.) ;
#21485 = ORIENTED_EDGE('',*,*,#15860,.T.) ;
#21486 = ORIENTED_EDGE('',*,*,#16050,.F.) ;
#21487 = ORIENTED_EDGE('',*,*,#16006,.F.) ;
#21488 = ORIENTED_EDGE('',*,*,#15968,.F.) ;
#21489 = ORIENTED_EDGE('',*,*,#16048,.F.) ;
#21490 = ORIENTED_EDGE('',*,*,#16038,.F.) ;
#21491 = ORIENTED_EDGE('',*,*,#16042,.F.) ;
#21492 = ORIENTED_EDGE('',*,*,#16036,.T.) ;
#21493 = ORIENTED_EDGE('',*,*,#16045,.F.) ;
#21494 = ORIENTED_EDGE('',*,*,#15862,.T.) ;
#21495 = ORIENTED_EDGE('',*,*,#16051,.T.) ;
#21496 = ORIENTED_EDGE('',*,*,#16052,.T.) ;
#21497 = ORIENTED_EDGE('',*,*,#16053,.T.) ;
#21498 = ORIENTED_EDGE('',*,*,#16054,.T.) ;
#21499 = ORIENTED_EDGE('',*,*,#16055,.T.) ;
#21500 = ORIENTED_EDGE('',*,*,#15916,.T.) ;
#21501 = ORIENTED_EDGE('',*,*,#16056,.F.) ;
#21502 = ORIENTED_EDGE('',*,*,#15931,.F.) ;
#21503 = ORIENTED_EDGE('',*,*,#15929,.T.) ;
#21504 = ORIENTED_EDGE('',*,*,#15806,.T.) ;
#21505 = ORIENTED_EDGE('',*,*,#15836,.T.) ;
#21506 = ORIENTED_EDGE('',*,*,#15919,.T.) ;
#21507 = ORIENTED_EDGE('',*,*,#16057,.F.) ;
#21508 = ORIENTED_EDGE('',*,*,#15926,.F.) ;
#21509 = ORIENTED_EDGE('',*,*,#15911,.F.) ;
#21510 = ORIENTED_EDGE('',*,*,#15928,.T.) ;
#21511 = ORIENTED_EDGE('',*,*,#16058,.F.) ;
#21512 = ORIENTED_EDGE('',*,*,#15917,.F.) ;
#21513 = ORIENTED_EDGE('',*,*,#16055,.F.) ;
#21514 = ORIENTED_EDGE('',*,*,#16057,.T.) ;
#21515 = ORIENTED_EDGE('',*,*,#15918,.T.) ;
#21516 = ORIENTED_EDGE('',*,*,#16058,.T.) ;
#21517 = ORIENTED_EDGE('',*,*,#15927,.T.) ;
#21518 = ORIENTED_EDGE('',*,*,#16059,.T.) ;
#21519 = ORIENTED_EDGE('',*,*,#16060,.T.) ;
#21520 = ORIENTED_EDGE('',*,*,#16061,.T.) ;
#21521 = ORIENTED_EDGE('',*,*,#16062,.T.) ;
#21522 = ORIENTED_EDGE('',*,*,#16054,.F.) ;
#21523 = ORIENTED_EDGE('',*,*,#16063,.T.) ;
#21524 = ORIENTED_EDGE('',*,*,#16062,.F.) ;
#21525 = ORIENTED_EDGE('',*,*,#16064,.F.) ;
#21526 = ORIENTED_EDGE('',*,*,#16053,.F.) ;
#21527 = ORIENTED_EDGE('',*,*,#16065,.T.) ;
#21528 = ORIENTED_EDGE('',*,*,#16059,.F.) ;
#21529 = ORIENTED_EDGE('',*,*,#16063,.F.) ;
#21530 = ORIENTED_EDGE('',*,*,#16052,.F.) ;
#21531 = ORIENTED_EDGE('',*,*,#16066,.T.) ;
#21532 = ORIENTED_EDGE('',*,*,#16060,.F.) ;
#21533 = ORIENTED_EDGE('',*,*,#16065,.F.) ;
#21534 = ORIENTED_EDGE('',*,*,#16051,.F.) ;
#21535 = ORIENTED_EDGE('',*,*,#16064,.T.) ;
#21536 = ORIENTED_EDGE('',*,*,#16061,.F.) ;
#21537 = ORIENTED_EDGE('',*,*,#16066,.F.) ;
#21538 = ORIENTED_EDGE('',*,*,#16067,.T.) ;
#21539 = ORIENTED_EDGE('',*,*,#16068,.T.) ;
#21540 = ORIENTED_EDGE('',*,*,#16069,.T.) ;
#21541 = ORIENTED_EDGE('',*,*,#16068,.F.) ;
#21542 = ORIENTED_EDGE('',*,*,#16070,.T.) ;
#21543 = ORIENTED_EDGE('',*,*,#16071,.F.) ;
#21544 = ORIENTED_EDGE('',*,*,#16070,.F.) ;
#21545 = ORIENTED_EDGE('',*,*,#15910,.F.) ;
#21546 = ORIENTED_EDGE('',*,*,#16072,.T.) ;
#21547 = ORIENTED_EDGE('',*,*,#16069,.F.) ;
#21548 = ORIENTED_EDGE('',*,*,#16072,.F.) ;
#21549 = ORIENTED_EDGE('',*,*,#15930,.T.) ;
#21550 = ORIENTED_EDGE('',*,*,#15924,.T.) ;
#21551 = ORIENTED_EDGE('',*,*,#16017,.F.) ;
#21552 = ORIENTED_EDGE('',*,*,#15985,.T.) ;
#21553 = ORIENTED_EDGE('',*,*,#15921,.T.) ;
#21554 = ORIENTED_EDGE('',*,*,#15805,.T.) ;
#21555 = ORIENTED_EDGE('',*,*,#15835,.T.) ;
#21556 = ORIENTED_EDGE('',*,*,#16071,.T.) ;
#21557 = ORIENTED_EDGE('',*,*,#16073,.T.) ;
#21558 = ORIENTED_EDGE('',*,*,#16074,.T.) ;
#21559 = ORIENTED_EDGE('',*,*,#16075,.T.) ;
#21560 = ORIENTED_EDGE('',*,*,#16074,.F.) ;
#21561 = ORIENTED_EDGE('',*,*,#16076,.T.) ;
#21562 = ORIENTED_EDGE('',*,*,#16073,.F.) ;
#21563 = ORIENTED_EDGE('',*,*,#16076,.F.) ;
#21564 = ORIENTED_EDGE('',*,*,#16067,.F.) ;
#21565 = ORIENTED_EDGE('',*,*,#16077,.T.) ;
#21566 = ORIENTED_EDGE('',*,*,#16075,.F.) ;
#21567 = ORIENTED_EDGE('',*,*,#16077,.F.) ;
#21568 = ORIENTED_EDGE('',*,*,#16078,.T.) ;
#21569 = ORIENTED_EDGE('',*,*,#16079,.T.) ;
#21570 = ORIENTED_EDGE('',*,*,#15904,.T.) ;
#21571 = ORIENTED_EDGE('',*,*,#16080,.F.) ;
#21572 = ORIENTED_EDGE('',*,*,#15938,.T.) ;
#21573 = ORIENTED_EDGE('',*,*,#15932,.F.) ;
#21574 = ORIENTED_EDGE('',*,*,#16056,.T.) ;
#21575 = ORIENTED_EDGE('',*,*,#15915,.T.) ;
#21576 = ORIENTED_EDGE('',*,*,#15906,.T.) ;
#21577 = ORIENTED_EDGE('',*,*,#15937,.F.) ;
#21578 = ORIENTED_EDGE('',*,*,#15955,.T.) ;
#21579 = ORIENTED_EDGE('',*,*,#16081,.F.) ;
#21580 = ORIENTED_EDGE('',*,*,#16082,.T.) ;
#21581 = ORIENTED_EDGE('',*,*,#16081,.T.) ;
#21582 = ORIENTED_EDGE('',*,*,#15954,.T.) ;
#21583 = ORIENTED_EDGE('',*,*,#15984,.F.) ;
#21584 = ORIENTED_EDGE('',*,*,#15872,.T.) ;
#21585 = ORIENTED_EDGE('',*,*,#15981,.F.) ;
#21586 = ORIENTED_EDGE('',*,*,#16016,.T.) ;
#21587 = ORIENTED_EDGE('',*,*,#16083,.T.) ;
#21588 = ORIENTED_EDGE('',*,*,#15903,.T.) ;
#21589 = ORIENTED_EDGE('',*,*,#16084,.T.) ;
#21590 = ORIENTED_EDGE('',*,*,#15939,.T.) ;
#21591 = ORIENTED_EDGE('',*,*,#16080,.T.) ;
#21592 = ORIENTED_EDGE('',*,*,#16085,.T.) ;
#21593 = ORIENTED_EDGE('',*,*,#16086,.F.) ;
#21594 = ORIENTED_EDGE('',*,*,#16087,.F.) ;
#21595 = ORIENTED_EDGE('',*,*,#15869,.F.) ;
#21596 = ORIENTED_EDGE('',*,*,#16079,.F.) ;
#21597 = ORIENTED_EDGE('',*,*,#16088,.F.) ;
#21598 = ORIENTED_EDGE('',*,*,#15982,.F.) ;
#21599 = ORIENTED_EDGE('',*,*,#15870,.F.) ;
#21600 = ORIENTED_EDGE('',*,*,#16087,.T.) ;
#21601 = ORIENTED_EDGE('',*,*,#16089,.F.) ;
#21602 = ORIENTED_EDGE('',*,*,#15900,.T.) ;
#21603 = ORIENTED_EDGE('',*,*,#15895,.F.) ;
#21604 = ORIENTED_EDGE('',*,*,#15896,.F.) ;
#21605 = ORIENTED_EDGE('',*,*,#15905,.F.) ;
#21606 = ORIENTED_EDGE('',*,*,#15875,.T.) ;
#21607 = ORIENTED_EDGE('',*,*,#16078,.F.) ;
#21608 = ORIENTED_EDGE('',*,*,#16082,.F.) ;
#21609 = ORIENTED_EDGE('',*,*,#15983,.T.) ;
#21610 = ORIENTED_EDGE('',*,*,#16088,.T.) ;
#21611 = ORIENTED_EDGE('',*,*,#15901,.T.) ;
#21612 = ORIENTED_EDGE('',*,*,#16089,.T.) ;
#21613 = ORIENTED_EDGE('',*,*,#16086,.T.) ;
#21614 = ORIENTED_EDGE('',*,*,#16090,.T.) ;
#21615 = ORIENTED_EDGE('',*,*,#16091,.T.) ;
#21616 = ORIENTED_EDGE('',*,*,#15902,.F.) ;
#21617 = ORIENTED_EDGE('',*,*,#15897,.T.) ;
#21618 = ORIENTED_EDGE('',*,*,#15893,.F.) ;
#21619 = ORIENTED_EDGE('',*,*,#15899,.F.) ;
#21620 = ORIENTED_EDGE('',*,*,#16090,.F.) ;
#21621 = ORIENTED_EDGE('',*,*,#16085,.F.) ;
#21622 = ORIENTED_EDGE('',*,*,#15873,.F.) ;
#21623 = ORIENTED_EDGE('',*,*,#16092,.T.) ;
#21624 = ORIENTED_EDGE('',*,*,#15976,.T.) ;
#21625 = ORIENTED_EDGE('',*,*,#15988,.T.) ;
#21626 = ORIENTED_EDGE('',*,*,#16093,.T.) ;
#21627 = ORIENTED_EDGE('',*,*,#16094,.T.) ;
#21628 = ORIENTED_EDGE('',*,*,#16095,.T.) ;
#21629 = ORIENTED_EDGE('',*,*,#16096,.T.) ;
#21630 = ORIENTED_EDGE('',*,*,#16093,.F.) ;
#21631 = ORIENTED_EDGE('',*,*,#15987,.T.) ;
#21632 = ORIENTED_EDGE('',*,*,#16019,.T.) ;
#21633 = ORIENTED_EDGE('',*,*,#16010,.F.) ;
#21634 = ORIENTED_EDGE('',*,*,#15991,.F.) ;
#21635 = ORIENTED_EDGE('',*,*,#15950,.F.) ;
#21636 = ORIENTED_EDGE('',*,*,#15990,.T.) ;
#21637 = ORIENTED_EDGE('',*,*,#16003,.F.) ;
#21638 = ORIENTED_EDGE('',*,*,#15960,.F.) ;
#21639 = ORIENTED_EDGE('',*,*,#15958,.F.) ;
#21640 = ORIENTED_EDGE('',*,*,#16007,.F.) ;
#21641 = ORIENTED_EDGE('',*,*,#16050,.T.) ;
#21642 = ORIENTED_EDGE('',*,*,#16044,.T.) ;
#21643 = ORIENTED_EDGE('',*,*,#16049,.T.) ;
#21644 = ORIENTED_EDGE('',*,*,#16032,.F.) ;
#21645 = ORIENTED_EDGE('',*,*,#15940,.F.) ;
#21646 = ORIENTED_EDGE('',*,*,#16084,.F.) ;
#21647 = ORIENTED_EDGE('',*,*,#16091,.F.) ;
#21648 = ORIENTED_EDGE('',*,*,#16083,.F.) ;
#21649 = ORIENTED_EDGE('',*,*,#16015,.F.) ;
#21650 = ORIENTED_EDGE('',*,*,#16018,.T.) ;
#21651 = ORIENTED_EDGE('',*,*,#15923,.T.) ;
#21652 = ORIENTED_EDGE('',*,*,#15934,.T.) ;
#21653 = ORIENTED_EDGE('',*,*,#16097,.T.) ;
#21654 = ORIENTED_EDGE('',*,*,#16098,.F.) ;
#21655 = ORIENTED_EDGE('',*,*,#16099,.F.) ;
#21656 = ORIENTED_EDGE('',*,*,#16100,.F.) ;
#21657 = ORIENTED_EDGE('',*,*,#16101,.T.) ;
#21658 = ORIENTED_EDGE('',*,*,#16102,.F.) ;
#21659 = ORIENTED_EDGE('',*,*,#16103,.F.) ;
#21660 = ORIENTED_EDGE('',*,*,#16104,.F.) ;
#21661 = ORIENTED_EDGE('',*,*,#16096,.F.) ;
#21662 = ORIENTED_EDGE('',*,*,#16105,.F.) ;
#21663 = ORIENTED_EDGE('',*,*,#16097,.F.) ;
#21664 = ORIENTED_EDGE('',*,*,#16106,.F.) ;
#21665 = ORIENTED_EDGE('',*,*,#16103,.T.) ;
#21666 = ORIENTED_EDGE('',*,*,#16107,.F.) ;
#21667 = ORIENTED_EDGE('',*,*,#15977,.F.) ;
#21668 = ORIENTED_EDGE('',*,*,#16092,.F.) ;
#21669 = ORIENTED_EDGE('',*,*,#15857,.T.) ;
#21670 = ORIENTED_EDGE('',*,*,#16095,.F.) ;
#21671 = ORIENTED_EDGE('',*,*,#16108,.T.) ;
#21672 = ORIENTED_EDGE('',*,*,#16098,.T.) ;
#21673 = ORIENTED_EDGE('',*,*,#16105,.T.) ;
#21674 = ORIENTED_EDGE('',*,*,#16100,.T.) ;
#21675 = ORIENTED_EDGE('',*,*,#16109,.T.) ;
#21676 = ORIENTED_EDGE('',*,*,#16104,.T.) ;
#21677 = ORIENTED_EDGE('',*,*,#16106,.T.) ;
#21678 = ORIENTED_EDGE('',*,*,#16094,.F.) ;
#21679 = ORIENTED_EDGE('',*,*,#16031,.F.) ;
#21680 = ORIENTED_EDGE('',*,*,#15964,.F.) ;
#21681 = ORIENTED_EDGE('',*,*,#16110,.F.) ;
#21682 = ORIENTED_EDGE('',*,*,#16101,.F.) ;
#21683 = ORIENTED_EDGE('',*,*,#16109,.F.) ;
#21684 = ORIENTED_EDGE('',*,*,#16099,.T.) ;
#21685 = ORIENTED_EDGE('',*,*,#16108,.F.) ;
#21686 = ORIENTED_EDGE('',*,*,#15859,.T.) ;
#21687 = ORIENTED_EDGE('',*,*,#15978,.F.) ;
#21688 = ORIENTED_EDGE('',*,*,#16107,.T.) ;
#21689 = ORIENTED_EDGE('',*,*,#16102,.T.) ;
#21690 = ORIENTED_EDGE('',*,*,#16110,.T.) ;
#21691 = ORIENTED_EDGE('',*,*,#16111,.F.) ;
#21692 = ORIENTED_EDGE('',*,*,#16112,.F.) ;
#21693 = ORIENTED_EDGE('',*,*,#16113,.F.) ;
#21694 = ORIENTED_EDGE('',*,*,#16114,.F.) ;
#21695 = ORIENTED_EDGE('',*,*,#16114,.T.) ;
#21696 = ORIENTED_EDGE('',*,*,#16115,.F.) ;
#21697 = ORIENTED_EDGE('',*,*,#16116,.T.) ;
#21698 = ORIENTED_EDGE('',*,*,#16117,.T.) ;
#21699 = ORIENTED_EDGE('',*,*,#16113,.T.) ;
#21700 = ORIENTED_EDGE('',*,*,#16118,.F.) ;
#21701 = ORIENTED_EDGE('',*,*,#16119,.T.) ;
#21702 = ORIENTED_EDGE('',*,*,#16115,.T.) ;
#21703 = ORIENTED_EDGE('',*,*,#16112,.T.) ;
#21704 = ORIENTED_EDGE('',*,*,#16120,.F.) ;
#21705 = ORIENTED_EDGE('',*,*,#16121,.T.) ;
#21706 = ORIENTED_EDGE('',*,*,#16118,.T.) ;
#21707 = ORIENTED_EDGE('',*,*,#16111,.T.) ;
#21708 = ORIENTED_EDGE('',*,*,#16117,.F.) ;
#21709 = ORIENTED_EDGE('',*,*,#16122,.T.) ;
#21710 = ORIENTED_EDGE('',*,*,#16120,.T.) ;
#21711 = ORIENTED_EDGE('',*,*,#16119,.F.) ;
#21712 = ORIENTED_EDGE('',*,*,#16121,.F.) ;
#21713 = ORIENTED_EDGE('',*,*,#16122,.F.) ;
#21714 = ORIENTED_EDGE('',*,*,#16116,.F.) ;
#21715 = ORIENTED_EDGE('',*,*,#16123,.F.) ;
#21716 = ORIENTED_EDGE('',*,*,#16124,.F.) ;
#21717 = ORIENTED_EDGE('',*,*,#16125,.F.) ;
#21718 = ORIENTED_EDGE('',*,*,#16126,.F.) ;
#21719 = ORIENTED_EDGE('',*,*,#16127,.T.) ;
#21720 = ORIENTED_EDGE('',*,*,#16128,.F.) ;
#21721 = ORIENTED_EDGE('',*,*,#16125,.T.) ;
#21722 = ORIENTED_EDGE('',*,*,#16129,.T.) ;
#21723 = ORIENTED_EDGE('',*,*,#16130,.T.) ;
#21724 = ORIENTED_EDGE('',*,*,#16129,.F.) ;
#21725 = ORIENTED_EDGE('',*,*,#16124,.T.) ;
#21726 = ORIENTED_EDGE('',*,*,#16131,.T.) ;
#21727 = ORIENTED_EDGE('',*,*,#16132,.T.) ;
#21728 = ORIENTED_EDGE('',*,*,#16131,.F.) ;
#21729 = ORIENTED_EDGE('',*,*,#16123,.T.) ;
#21730 = ORIENTED_EDGE('',*,*,#16133,.T.) ;
#21731 = ORIENTED_EDGE('',*,*,#16134,.T.) ;
#21732 = ORIENTED_EDGE('',*,*,#16133,.F.) ;
#21733 = ORIENTED_EDGE('',*,*,#16126,.T.) ;
#21734 = ORIENTED_EDGE('',*,*,#16128,.T.) ;
#21735 = ORIENTED_EDGE('',*,*,#16127,.F.) ;
#21736 = ORIENTED_EDGE('',*,*,#16130,.F.) ;
#21737 = ORIENTED_EDGE('',*,*,#16132,.F.) ;
#21738 = ORIENTED_EDGE('',*,*,#16134,.F.) ;
#21739 = ORIENTED_EDGE('',*,*,#16135,.F.) ;
#21740 = ORIENTED_EDGE('',*,*,#16136,.T.) ;
#21741 = ORIENTED_EDGE('',*,*,#16137,.F.) ;
#21742 = ORIENTED_EDGE('',*,*,#16138,.T.) ;
#21743 = ORIENTED_EDGE('',*,*,#16139,.F.) ;
#21744 = ORIENTED_EDGE('',*,*,#16136,.F.) ;
#21745 = ORIENTED_EDGE('',*,*,#16140,.F.) ;
#21746 = ORIENTED_EDGE('',*,*,#16138,.F.) ;
#21747 = ORIENTED_EDGE('',*,*,#16140,.T.) ;
#21748 = ORIENTED_EDGE('',*,*,#16135,.T.) ;
#21749 = ORIENTED_EDGE('',*,*,#16139,.T.) ;
#21750 = ORIENTED_EDGE('',*,*,#16137,.T.) ;
#21751 = ORIENTED_EDGE('',*,*,#16141,.F.) ;
#21752 = ORIENTED_EDGE('',*,*,#16142,.F.) ;
#21753 = ORIENTED_EDGE('',*,*,#16143,.F.) ;
#21754 = ORIENTED_EDGE('',*,*,#16144,.F.) ;
#21755 = ORIENTED_EDGE('',*,*,#16145,.F.) ;
#21756 = ORIENTED_EDGE('',*,*,#16144,.T.) ;
#21757 = ORIENTED_EDGE('',*,*,#16146,.F.) ;
#21758 = ORIENTED_EDGE('',*,*,#16147,.F.) ;
#21759 = ORIENTED_EDGE('',*,*,#16145,.T.) ;
#21760 = ORIENTED_EDGE('',*,*,#16148,.T.) ;
#21761 = ORIENTED_EDGE('',*,*,#16141,.T.) ;
#21762 = ORIENTED_EDGE('',*,*,#16146,.T.) ;
#21763 = ORIENTED_EDGE('',*,*,#16143,.T.) ;
#21764 = ORIENTED_EDGE('',*,*,#16149,.T.) ;
#21765 = ORIENTED_EDGE('',*,*,#16147,.T.) ;
#21766 = ORIENTED_EDGE('',*,*,#16149,.F.) ;
#21767 = ORIENTED_EDGE('',*,*,#16142,.T.) ;
#21768 = ORIENTED_EDGE('',*,*,#16148,.F.) ;
#21769 = ORIENTED_EDGE('',*,*,#16150,.T.) ;
#21770 = ORIENTED_EDGE('',*,*,#16151,.T.) ;
#21771 = ORIENTED_EDGE('',*,*,#16152,.T.) ;
#21772 = ORIENTED_EDGE('',*,*,#16153,.T.) ;
#21773 = ORIENTED_EDGE('',*,*,#16152,.F.) ;
#21774 = ORIENTED_EDGE('',*,*,#16154,.T.) ;
#21775 = ORIENTED_EDGE('',*,*,#16155,.T.) ;
#21776 = ORIENTED_EDGE('',*,*,#16156,.T.) ;
#21777 = ORIENTED_EDGE('',*,*,#16155,.F.) ;
#21778 = ORIENTED_EDGE('',*,*,#16157,.T.) ;
#21779 = ORIENTED_EDGE('',*,*,#16158,.T.) ;
#21780 = ORIENTED_EDGE('',*,*,#16157,.F.) ;
#21781 = ORIENTED_EDGE('',*,*,#16154,.F.) ;
#21782 = ORIENTED_EDGE('',*,*,#16151,.F.) ;
#21783 = ORIENTED_EDGE('',*,*,#16156,.F.) ;
#21784 = ORIENTED_EDGE('',*,*,#16158,.F.) ;
#21785 = ORIENTED_EDGE('',*,*,#16150,.F.) ;
#21786 = ORIENTED_EDGE('',*,*,#16153,.F.) ;
#21787 = ORIENTED_EDGE('',*,*,#16159,.F.) ;
#21788 = ORIENTED_EDGE('',*,*,#16160,.F.) ;
#21789 = ORIENTED_EDGE('',*,*,#16161,.F.) ;
#21790 = ORIENTED_EDGE('',*,*,#16162,.F.) ;
#21791 = ORIENTED_EDGE('',*,*,#16163,.F.) ;
#21792 = ORIENTED_EDGE('',*,*,#16164,.F.) ;
#21793 = ORIENTED_EDGE('',*,*,#16165,.F.) ;
#21794 = ORIENTED_EDGE('',*,*,#16160,.T.) ;
#21795 = ORIENTED_EDGE('',*,*,#16163,.T.) ;
#21796 = ORIENTED_EDGE('',*,*,#16159,.T.) ;
#21797 = ORIENTED_EDGE('',*,*,#16166,.T.) ;
#21798 = ORIENTED_EDGE('',*,*,#16165,.T.) ;
#21799 = ORIENTED_EDGE('',*,*,#16167,.T.) ;
#21800 = ORIENTED_EDGE('',*,*,#16161,.T.) ;
#21801 = ORIENTED_EDGE('',*,*,#16164,.T.) ;
#21802 = ORIENTED_EDGE('',*,*,#16166,.F.) ;
#21803 = ORIENTED_EDGE('',*,*,#16162,.T.) ;
#21804 = ORIENTED_EDGE('',*,*,#16167,.F.) ;
#21805 = ORIENTED_EDGE('',*,*,#16168,.T.) ;
#21806 = ORIENTED_EDGE('',*,*,#16169,.F.) ;
#21807 = ORIENTED_EDGE('',*,*,#16170,.T.) ;
#21808 = ORIENTED_EDGE('',*,*,#16171,.T.) ;
#21809 = ORIENTED_EDGE('',*,*,#16172,.T.) ;
#21810 = ORIENTED_EDGE('',*,*,#16173,.T.) ;
#21811 = ORIENTED_EDGE('',*,*,#16174,.T.) ;
#21812 = ORIENTED_EDGE('',*,*,#16170,.F.) ;
#21813 = ORIENTED_EDGE('',*,*,#16175,.F.) ;
#21814 = ORIENTED_EDGE('',*,*,#16172,.F.) ;
#21815 = ORIENTED_EDGE('',*,*,#16176,.T.) ;
#21816 = ORIENTED_EDGE('',*,*,#16173,.F.) ;
#21817 = ORIENTED_EDGE('',*,*,#16175,.T.) ;
#21818 = ORIENTED_EDGE('',*,*,#16169,.T.) ;
#21819 = ORIENTED_EDGE('',*,*,#16168,.F.) ;
#21820 = ORIENTED_EDGE('',*,*,#16174,.F.) ;
#21821 = ORIENTED_EDGE('',*,*,#16171,.F.) ;
#21822 = ORIENTED_EDGE('',*,*,#16176,.F.) ;
#21823 = ORIENTED_EDGE('',*,*,#16177,.F.) ;
#21824 = ORIENTED_EDGE('',*,*,#16178,.F.) ;
#21825 = ORIENTED_EDGE('',*,*,#16179,.F.) ;
#21826 = ORIENTED_EDGE('',*,*,#16180,.F.) ;
#21827 = ORIENTED_EDGE('',*,*,#16178,.T.) ;
#21828 = ORIENTED_EDGE('',*,*,#16181,.F.) ;
#21829 = ORIENTED_EDGE('',*,*,#16182,.F.) ;
#21830 = ORIENTED_EDGE('',*,*,#16183,.F.) ;
#21831 = ORIENTED_EDGE('',*,*,#16177,.T.) ;
#21832 = ORIENTED_EDGE('',*,*,#16184,.F.) ;
#21833 = ORIENTED_EDGE('',*,*,#16181,.T.) ;
#21834 = ORIENTED_EDGE('',*,*,#16180,.T.) ;
#21835 = ORIENTED_EDGE('',*,*,#16185,.F.) ;
#21836 = ORIENTED_EDGE('',*,*,#16182,.T.) ;
#21837 = ORIENTED_EDGE('',*,*,#16184,.T.) ;
#21838 = ORIENTED_EDGE('',*,*,#16179,.T.) ;
#21839 = ORIENTED_EDGE('',*,*,#16183,.T.) ;
#21840 = ORIENTED_EDGE('',*,*,#16185,.T.) ;
#21841 = ORIENTED_EDGE('',*,*,#16186,.T.) ;
#21842 = ORIENTED_EDGE('',*,*,#16187,.F.) ;
#21843 = ORIENTED_EDGE('',*,*,#16188,.T.) ;
#21844 = ORIENTED_EDGE('',*,*,#16189,.T.) ;
#21845 = ORIENTED_EDGE('',*,*,#16190,.T.) ;
#21846 = ORIENTED_EDGE('',*,*,#16191,.T.) ;
#21847 = ORIENTED_EDGE('',*,*,#16192,.T.) ;
#21848 = ORIENTED_EDGE('',*,*,#16188,.F.) ;
#21849 = ORIENTED_EDGE('',*,*,#16193,.F.) ;
#21850 = ORIENTED_EDGE('',*,*,#16190,.F.) ;
#21851 = ORIENTED_EDGE('',*,*,#16194,.T.) ;
#21852 = ORIENTED_EDGE('',*,*,#16191,.F.) ;
#21853 = ORIENTED_EDGE('',*,*,#16193,.T.) ;
#21854 = ORIENTED_EDGE('',*,*,#16187,.T.) ;
#21855 = ORIENTED_EDGE('',*,*,#16186,.F.) ;
#21856 = ORIENTED_EDGE('',*,*,#16192,.F.) ;
#21857 = ORIENTED_EDGE('',*,*,#16189,.F.) ;
#21858 = ORIENTED_EDGE('',*,*,#16194,.F.) ;
#21859 = ORIENTED_EDGE('',*,*,#16195,.F.) ;
#21860 = ORIENTED_EDGE('',*,*,#16196,.F.) ;
#21861 = ORIENTED_EDGE('',*,*,#16197,.F.) ;
#21862 = ORIENTED_EDGE('',*,*,#16198,.F.) ;
#21863 = ORIENTED_EDGE('',*,*,#16198,.T.) ;
#21864 = ORIENTED_EDGE('',*,*,#16199,.T.) ;
#21865 = ORIENTED_EDGE('',*,*,#16196,.T.) ;
#21866 = ORIENTED_EDGE('',*,*,#16200,.T.) ;
#21867 = ORIENTED_EDGE('',*,*,#16197,.T.) ;
#21868 = ORIENTED_EDGE('',*,*,#16200,.F.) ;
#21869 = ORIENTED_EDGE('',*,*,#16195,.T.) ;
#21870 = ORIENTED_EDGE('',*,*,#16199,.F.) ;
#21871 = ORIENTED_EDGE('',*,*,#16201,.T.) ;
#21872 = ORIENTED_EDGE('',*,*,#16202,.F.) ;
#21873 = ORIENTED_EDGE('',*,*,#16203,.T.) ;
#21874 = ORIENTED_EDGE('',*,*,#16204,.F.) ;
#21875 = ORIENTED_EDGE('',*,*,#16205,.T.) ;
#21876 = ORIENTED_EDGE('',*,*,#16204,.T.) ;
#21877 = ORIENTED_EDGE('',*,*,#16206,.T.) ;
#21878 = ORIENTED_EDGE('',*,*,#16202,.T.) ;
#21879 = ORIENTED_EDGE('',*,*,#16205,.F.) ;
#21880 = ORIENTED_EDGE('',*,*,#16203,.F.) ;
#21881 = ORIENTED_EDGE('',*,*,#16206,.F.) ;
#21882 = ORIENTED_EDGE('',*,*,#16201,.F.) ;
#21883 = ORIENTED_EDGE('',*,*,#16207,.F.) ;
#21884 = ORIENTED_EDGE('',*,*,#16208,.F.) ;
#21885 = ORIENTED_EDGE('',*,*,#16209,.F.) ;
#21886 = ORIENTED_EDGE('',*,*,#16210,.F.) ;
#21887 = ORIENTED_EDGE('',*,*,#16209,.T.) ;
#21888 = ORIENTED_EDGE('',*,*,#16211,.T.) ;
#21889 = ORIENTED_EDGE('',*,*,#16207,.T.) ;
#21890 = ORIENTED_EDGE('',*,*,#16212,.T.) ;
#21891 = ORIENTED_EDGE('',*,*,#16210,.T.) ;
#21892 = ORIENTED_EDGE('',*,*,#16211,.F.) ;
#21893 = ORIENTED_EDGE('',*,*,#16208,.T.) ;
#21894 = ORIENTED_EDGE('',*,*,#16212,.F.) ;
#21895 = ORIENTED_EDGE('',*,*,#16213,.T.) ;
#21896 = ORIENTED_EDGE('',*,*,#16214,.F.) ;
#21897 = ORIENTED_EDGE('',*,*,#16215,.T.) ;
#21898 = ORIENTED_EDGE('',*,*,#16216,.F.) ;
#21899 = ORIENTED_EDGE('',*,*,#16217,.T.) ;
#21900 = ORIENTED_EDGE('',*,*,#16214,.T.) ;
#21901 = ORIENTED_EDGE('',*,*,#16218,.T.) ;
#21902 = ORIENTED_EDGE('',*,*,#16216,.T.) ;
#21903 = ORIENTED_EDGE('',*,*,#16215,.F.) ;
#21904 = ORIENTED_EDGE('',*,*,#16217,.F.) ;
#21905 = ORIENTED_EDGE('',*,*,#16213,.F.) ;
#21906 = ORIENTED_EDGE('',*,*,#16218,.F.) ;
#21907 = ORIENTED_EDGE('',*,*,#16219,.F.) ;
#21908 = ORIENTED_EDGE('',*,*,#16220,.F.) ;
#21909 = ORIENTED_EDGE('',*,*,#16221,.F.) ;
#21910 = ORIENTED_EDGE('',*,*,#16222,.F.) ;
#21911 = ORIENTED_EDGE('',*,*,#16220,.T.) ;
#21912 = ORIENTED_EDGE('',*,*,#16223,.T.) ;
#21913 = ORIENTED_EDGE('',*,*,#16221,.T.) ;
#21914 = ORIENTED_EDGE('',*,*,#16223,.F.) ;
#21915 = ORIENTED_EDGE('',*,*,#16219,.T.) ;
#21916 = ORIENTED_EDGE('',*,*,#16224,.F.) ;
#21917 = ORIENTED_EDGE('',*,*,#16222,.T.) ;
#21918 = ORIENTED_EDGE('',*,*,#16224,.T.) ;
#21919 = ORIENTED_EDGE('',*,*,#16225,.T.) ;
#21920 = ORIENTED_EDGE('',*,*,#16226,.T.) ;
#21921 = ORIENTED_EDGE('',*,*,#16227,.T.) ;
#21922 = ORIENTED_EDGE('',*,*,#16228,.F.) ;
#21923 = ORIENTED_EDGE('',*,*,#16229,.T.) ;
#21924 = ORIENTED_EDGE('',*,*,#16230,.T.) ;
#21925 = ORIENTED_EDGE('',*,*,#16231,.T.) ;
#21926 = ORIENTED_EDGE('',*,*,#16226,.F.) ;
#21927 = ORIENTED_EDGE('',*,*,#16232,.T.) ;
#21928 = ORIENTED_EDGE('',*,*,#16228,.T.) ;
#21929 = ORIENTED_EDGE('',*,*,#16233,.T.) ;
#21930 = ORIENTED_EDGE('',*,*,#16234,.F.) ;
#21931 = ORIENTED_EDGE('',*,*,#16235,.T.) ;
#21932 = ORIENTED_EDGE('',*,*,#16234,.T.) ;
#21933 = ORIENTED_EDGE('',*,*,#16236,.T.) ;
#21934 = ORIENTED_EDGE('',*,*,#16230,.F.) ;
#21935 = ORIENTED_EDGE('',*,*,#16236,.F.) ;
#21936 = ORIENTED_EDGE('',*,*,#16233,.F.) ;
#21937 = ORIENTED_EDGE('',*,*,#16227,.F.) ;
#21938 = ORIENTED_EDGE('',*,*,#16231,.F.) ;
#21939 = ORIENTED_EDGE('',*,*,#16235,.F.) ;
#21940 = ORIENTED_EDGE('',*,*,#16229,.F.) ;
#21941 = ORIENTED_EDGE('',*,*,#16225,.F.) ;
#21942 = ORIENTED_EDGE('',*,*,#16232,.F.) ;
#21943 = ORIENTED_EDGE('',*,*,#16237,.F.) ;
#21944 = ORIENTED_EDGE('',*,*,#16238,.F.) ;
#21945 = ORIENTED_EDGE('',*,*,#16239,.F.) ;
#21946 = ORIENTED_EDGE('',*,*,#16240,.F.) ;
#21947 = ORIENTED_EDGE('',*,*,#16241,.F.) ;
#21948 = ORIENTED_EDGE('',*,*,#16242,.F.) ;
#21949 = ORIENTED_EDGE('',*,*,#16243,.F.) ;
#21950 = ORIENTED_EDGE('',*,*,#16244,.F.) ;
#21951 = ORIENTED_EDGE('',*,*,#16237,.T.) ;
#21952 = ORIENTED_EDGE('',*,*,#16245,.T.) ;
#21953 = ORIENTED_EDGE('',*,*,#16241,.T.) ;
#21954 = ORIENTED_EDGE('',*,*,#16246,.F.) ;
#21955 = ORIENTED_EDGE('',*,*,#16240,.T.) ;
#21956 = ORIENTED_EDGE('',*,*,#16247,.T.) ;
#21957 = ORIENTED_EDGE('',*,*,#16242,.T.) ;
#21958 = ORIENTED_EDGE('',*,*,#16245,.F.) ;
#21959 = ORIENTED_EDGE('',*,*,#16238,.T.) ;
#21960 = ORIENTED_EDGE('',*,*,#16246,.T.) ;
#21961 = ORIENTED_EDGE('',*,*,#16244,.T.) ;
#21962 = ORIENTED_EDGE('',*,*,#16248,.F.) ;
#21963 = ORIENTED_EDGE('',*,*,#16239,.T.) ;
#21964 = ORIENTED_EDGE('',*,*,#16248,.T.) ;
#21965 = ORIENTED_EDGE('',*,*,#16243,.T.) ;
#21966 = ORIENTED_EDGE('',*,*,#16247,.F.) ;
#21967 = ORIENTED_EDGE('',*,*,#16249,.F.) ;
#21968 = ORIENTED_EDGE('',*,*,#16250,.F.) ;
#21969 = ORIENTED_EDGE('',*,*,#16251,.F.) ;
#21970 = ORIENTED_EDGE('',*,*,#16252,.F.) ;
#21971 = ORIENTED_EDGE('',*,*,#16253,.F.) ;
#21972 = ORIENTED_EDGE('',*,*,#16254,.T.) ;
#21973 = ORIENTED_EDGE('',*,*,#16255,.F.) ;
#21974 = ORIENTED_EDGE('',*,*,#16250,.T.) ;
#21975 = ORIENTED_EDGE('',*,*,#16256,.F.) ;
#21976 = ORIENTED_EDGE('',*,*,#16257,.F.) ;
#21977 = ORIENTED_EDGE('',*,*,#16258,.F.) ;
#21978 = ORIENTED_EDGE('',*,*,#16254,.F.) ;
#21979 = ORIENTED_EDGE('',*,*,#16251,.T.) ;
#21980 = ORIENTED_EDGE('',*,*,#16255,.T.) ;
#21981 = ORIENTED_EDGE('',*,*,#16258,.T.) ;
#21982 = ORIENTED_EDGE('',*,*,#16259,.T.) ;
#21983 = ORIENTED_EDGE('',*,*,#16260,.T.) ;
#21984 = ORIENTED_EDGE('',*,*,#16261,.T.) ;
#21985 = ORIENTED_EDGE('',*,*,#16262,.T.) ;
#21986 = ORIENTED_EDGE('',*,*,#16263,.T.) ;
#21987 = ORIENTED_EDGE('',*,*,#16264,.F.) ;
#21988 = ORIENTED_EDGE('',*,*,#16265,.T.) ;
#21989 = ORIENTED_EDGE('',*,*,#16266,.F.) ;
#21990 = ORIENTED_EDGE('',*,*,#16267,.T.) ;
#21991 = ORIENTED_EDGE('',*,*,#16257,.T.) ;
#21992 = ORIENTED_EDGE('',*,*,#16268,.F.) ;
#21993 = ORIENTED_EDGE('',*,*,#16269,.T.) ;
#21994 = ORIENTED_EDGE('',*,*,#16259,.F.) ;
#21995 = ORIENTED_EDGE('',*,*,#16252,.T.) ;
#21996 = ORIENTED_EDGE('',*,*,#16267,.F.) ;
#21997 = ORIENTED_EDGE('',*,*,#16270,.F.) ;
#21998 = ORIENTED_EDGE('',*,*,#16271,.F.) ;
#21999 = ORIENTED_EDGE('',*,*,#16249,.T.) ;
#22000 = ORIENTED_EDGE('',*,*,#16271,.T.) ;
#22001 = ORIENTED_EDGE('',*,*,#16272,.F.) ;
#22002 = ORIENTED_EDGE('',*,*,#16273,.T.) ;
#22003 = ORIENTED_EDGE('',*,*,#16274,.F.) ;
#22004 = ORIENTED_EDGE('',*,*,#16275,.T.) ;
#22005 = ORIENTED_EDGE('',*,*,#16276,.T.) ;
#22006 = ORIENTED_EDGE('',*,*,#16277,.T.) ;
#22007 = ORIENTED_EDGE('',*,*,#16278,.T.) ;
#22008 = ORIENTED_EDGE('',*,*,#16268,.T.) ;
#22009 = ORIENTED_EDGE('',*,*,#16256,.T.) ;
#22010 = ORIENTED_EDGE('',*,*,#16253,.T.) ;
#22011 = ORIENTED_EDGE('',*,*,#16279,.F.) ;
#22012 = ORIENTED_EDGE('',*,*,#16273,.F.) ;
#22013 = ORIENTED_EDGE('',*,*,#16280,.F.) ;
#22014 = ORIENTED_EDGE('',*,*,#16265,.F.) ;
#22015 = ORIENTED_EDGE('',*,*,#16280,.T.) ;
#22016 = ORIENTED_EDGE('',*,*,#16272,.T.) ;
#22017 = ORIENTED_EDGE('',*,*,#16270,.T.) ;
#22018 = ORIENTED_EDGE('',*,*,#16266,.T.) ;
#22019 = ORIENTED_EDGE('',*,*,#16279,.T.) ;
#22020 = ORIENTED_EDGE('',*,*,#16264,.T.) ;
#22021 = ORIENTED_EDGE('',*,*,#16281,.T.) ;
#22022 = ORIENTED_EDGE('',*,*,#16274,.T.) ;
#22023 = ORIENTED_EDGE('',*,*,#16282,.T.) ;
#22024 = ORIENTED_EDGE('',*,*,#16275,.F.) ;
#22025 = ORIENTED_EDGE('',*,*,#16281,.F.) ;
#22026 = ORIENTED_EDGE('',*,*,#16263,.F.) ;
#22027 = ORIENTED_EDGE('',*,*,#16262,.F.) ;
#22028 = ORIENTED_EDGE('',*,*,#16283,.F.) ;
#22029 = ORIENTED_EDGE('',*,*,#16276,.F.) ;
#22030 = ORIENTED_EDGE('',*,*,#16282,.F.) ;
#22031 = ORIENTED_EDGE('',*,*,#16261,.F.) ;
#22032 = ORIENTED_EDGE('',*,*,#16284,.T.) ;
#22033 = ORIENTED_EDGE('',*,*,#16277,.F.) ;
#22034 = ORIENTED_EDGE('',*,*,#16283,.T.) ;
#22035 = ORIENTED_EDGE('',*,*,#16260,.F.) ;
#22036 = ORIENTED_EDGE('',*,*,#16269,.F.) ;
#22037 = ORIENTED_EDGE('',*,*,#16278,.F.) ;
#22038 = ORIENTED_EDGE('',*,*,#16284,.F.) ;
#22039 = ORIENTED_EDGE('',*,*,#16285,.T.) ;
#22040 = ORIENTED_EDGE('',*,*,#16286,.T.) ;
#22041 = ORIENTED_EDGE('',*,*,#16287,.T.) ;
#22042 = ORIENTED_EDGE('',*,*,#16288,.T.) ;
#22043 = ORIENTED_EDGE('',*,*,#16287,.F.) ;
#22044 = ORIENTED_EDGE('',*,*,#16289,.F.) ;
#22045 = ORIENTED_EDGE('',*,*,#16285,.F.) ;
#22046 = ORIENTED_EDGE('',*,*,#16290,.F.) ;
#22047 = ORIENTED_EDGE('',*,*,#16288,.F.) ;
#22048 = ORIENTED_EDGE('',*,*,#16290,.T.) ;
#22049 = ORIENTED_EDGE('',*,*,#16286,.F.) ;
#22050 = ORIENTED_EDGE('',*,*,#16289,.T.) ;
#22051 = ORIENTED_EDGE('',*,*,#16291,.F.) ;
#22052 = ORIENTED_EDGE('',*,*,#16292,.F.) ;
#22053 = ORIENTED_EDGE('',*,*,#16293,.F.) ;
#22054 = ORIENTED_EDGE('',*,*,#16294,.F.) ;
#22055 = ORIENTED_EDGE('',*,*,#16295,.F.) ;
#22056 = ORIENTED_EDGE('',*,*,#16292,.T.) ;
#22057 = ORIENTED_EDGE('',*,*,#16293,.T.) ;
#22058 = ORIENTED_EDGE('',*,*,#16291,.T.) ;
#22059 = ORIENTED_EDGE('',*,*,#16295,.T.) ;
#22060 = ORIENTED_EDGE('',*,*,#16296,.F.) ;
#22061 = ORIENTED_EDGE('',*,*,#16297,.T.) ;
#22062 = ORIENTED_EDGE('',*,*,#16298,.F.) ;
#22063 = ORIENTED_EDGE('',*,*,#16299,.T.) ;
#22064 = ORIENTED_EDGE('',*,*,#16300,.T.) ;
#22065 = ORIENTED_EDGE('',*,*,#16301,.T.) ;
#22066 = ORIENTED_EDGE('',*,*,#16302,.F.) ;
#22067 = ORIENTED_EDGE('',*,*,#16303,.T.) ;
#22068 = ORIENTED_EDGE('',*,*,#16304,.F.) ;
#22069 = ORIENTED_EDGE('',*,*,#16300,.F.) ;
#22070 = ORIENTED_EDGE('',*,*,#16305,.F.) ;
#22071 = ORIENTED_EDGE('',*,*,#16299,.F.) ;
#22072 = ORIENTED_EDGE('',*,*,#16306,.F.) ;
#22073 = ORIENTED_EDGE('',*,*,#16301,.F.) ;
#22074 = ORIENTED_EDGE('',*,*,#16305,.T.) ;
#22075 = ORIENTED_EDGE('',*,*,#16306,.T.) ;
#22076 = ORIENTED_EDGE('',*,*,#16298,.T.) ;
#22077 = ORIENTED_EDGE('',*,*,#16307,.T.) ;
#22078 = ORIENTED_EDGE('',*,*,#16302,.T.) ;
#22079 = ORIENTED_EDGE('',*,*,#16294,.T.) ;
#22080 = ORIENTED_EDGE('',*,*,#16304,.T.) ;
#22081 = ORIENTED_EDGE('',*,*,#16308,.T.) ;
#22082 = ORIENTED_EDGE('',*,*,#16296,.T.) ;
#22083 = ORIENTED_EDGE('',*,*,#16297,.F.) ;
#22084 = ORIENTED_EDGE('',*,*,#16308,.F.) ;
#22085 = ORIENTED_EDGE('',*,*,#16303,.F.) ;
#22086 = ORIENTED_EDGE('',*,*,#16307,.F.) ;
#22087 = ORIENTED_EDGE('',*,*,#16309,.T.) ;
#22088 = ORIENTED_EDGE('',*,*,#16310,.T.) ;
#22089 = ORIENTED_EDGE('',*,*,#16311,.T.) ;
#22090 = ORIENTED_EDGE('',*,*,#16312,.T.) ;
#22091 = ORIENTED_EDGE('',*,*,#16313,.T.) ;
#22092 = ORIENTED_EDGE('',*,*,#16314,.T.) ;
#22093 = ORIENTED_EDGE('',*,*,#16315,.T.) ;
#22094 = ORIENTED_EDGE('',*,*,#16316,.T.) ;
#22095 = ORIENTED_EDGE('',*,*,#16317,.T.) ;
#22096 = ORIENTED_EDGE('',*,*,#16314,.F.) ;
#22097 = ORIENTED_EDGE('',*,*,#16318,.F.) ;
#22098 = ORIENTED_EDGE('',*,*,#16312,.F.) ;
#22099 = ORIENTED_EDGE('',*,*,#16319,.T.) ;
#22100 = ORIENTED_EDGE('',*,*,#16315,.F.) ;
#22101 = ORIENTED_EDGE('',*,*,#16317,.F.) ;
#22102 = ORIENTED_EDGE('',*,*,#16311,.F.) ;
#22103 = ORIENTED_EDGE('',*,*,#16320,.T.) ;
#22104 = ORIENTED_EDGE('',*,*,#16316,.F.) ;
#22105 = ORIENTED_EDGE('',*,*,#16319,.F.) ;
#22106 = ORIENTED_EDGE('',*,*,#16310,.F.) ;
#22107 = ORIENTED_EDGE('',*,*,#16318,.T.) ;
#22108 = ORIENTED_EDGE('',*,*,#16313,.F.) ;
#22109 = ORIENTED_EDGE('',*,*,#16320,.F.) ;
#22110 = ORIENTED_EDGE('',*,*,#16309,.F.) ;
#22111 = ORIENTED_EDGE('',*,*,#16321,.F.) ;
#22112 = ORIENTED_EDGE('',*,*,#16322,.F.) ;
#22113 = ORIENTED_EDGE('',*,*,#16323,.T.) ;
#22114 = ORIENTED_EDGE('',*,*,#16324,.F.) ;
#22115 = ORIENTED_EDGE('',*,*,#16325,.F.) ;
#22116 = ORIENTED_EDGE('',*,*,#16323,.F.) ;
#22117 = ORIENTED_EDGE('',*,*,#16326,.T.) ;
#22118 = ORIENTED_EDGE('',*,*,#16327,.T.) ;
#22119 = ORIENTED_EDGE('',*,*,#16326,.F.) ;
#22120 = ORIENTED_EDGE('',*,*,#16328,.T.) ;
#22121 = ORIENTED_EDGE('',*,*,#16329,.F.) ;
#22122 = ORIENTED_EDGE('',*,*,#16328,.F.) ;
#22123 = ORIENTED_EDGE('',*,*,#16329,.T.) ;
#22124 = ORIENTED_EDGE('',*,*,#16330,.F.) ;
#22125 = ORIENTED_EDGE('',*,*,#16331,.T.) ;
#22126 = ORIENTED_EDGE('',*,*,#16327,.F.) ;
#22127 = ORIENTED_EDGE('',*,*,#16331,.F.) ;
#22128 = ORIENTED_EDGE('',*,*,#16324,.T.) ;
#22129 = ORIENTED_EDGE('',*,*,#16325,.T.) ;
#22130 = ORIENTED_EDGE('',*,*,#16321,.T.) ;
#22131 = ORIENTED_EDGE('',*,*,#16322,.T.) ;
#22132 = ORIENTED_EDGE('',*,*,#16330,.T.) ;
#22133 = ORIENTED_EDGE('',*,*,#16332,.F.) ;
#22134 = ORIENTED_EDGE('',*,*,#16333,.F.) ;
#22135 = ORIENTED_EDGE('',*,*,#16334,.T.) ;
#22136 = ORIENTED_EDGE('',*,*,#16335,.F.) ;
#22137 = ORIENTED_EDGE('',*,*,#16336,.F.) ;
#22138 = ORIENTED_EDGE('',*,*,#16334,.F.) ;
#22139 = ORIENTED_EDGE('',*,*,#16337,.T.) ;
#22140 = ORIENTED_EDGE('',*,*,#16338,.T.) ;
#22141 = ORIENTED_EDGE('',*,*,#16337,.F.) ;
#22142 = ORIENTED_EDGE('',*,*,#16339,.T.) ;
#22143 = ORIENTED_EDGE('',*,*,#16340,.F.) ;
#22144 = ORIENTED_EDGE('',*,*,#16339,.F.) ;
#22145 = ORIENTED_EDGE('',*,*,#16340,.T.) ;
#22146 = ORIENTED_EDGE('',*,*,#16341,.F.) ;
#22147 = ORIENTED_EDGE('',*,*,#16342,.T.) ;
#22148 = ORIENTED_EDGE('',*,*,#16338,.F.) ;
#22149 = ORIENTED_EDGE('',*,*,#16342,.F.) ;
#22150 = ORIENTED_EDGE('',*,*,#16335,.T.) ;
#22151 = ORIENTED_EDGE('',*,*,#16336,.T.) ;
#22152 = ORIENTED_EDGE('',*,*,#16332,.T.) ;
#22153 = ORIENTED_EDGE('',*,*,#16333,.T.) ;
#22154 = ORIENTED_EDGE('',*,*,#16341,.T.) ;
#22155 = ORIENTED_EDGE('',*,*,#16343,.F.) ;
#22156 = ORIENTED_EDGE('',*,*,#16344,.T.) ;
#22157 = ORIENTED_EDGE('',*,*,#16345,.F.) ;
#22158 = ORIENTED_EDGE('',*,*,#16344,.F.) ;
#22159 = ORIENTED_EDGE('',*,*,#16346,.F.) ;
#22160 = ORIENTED_EDGE('',*,*,#16347,.T.) ;
#22161 = ORIENTED_EDGE('',*,*,#16348,.F.) ;
#22162 = ORIENTED_EDGE('',*,*,#16347,.F.) ;
#22163 = ORIENTED_EDGE('',*,*,#16349,.F.) ;
#22164 = ORIENTED_EDGE('',*,*,#16350,.T.) ;
#22165 = ORIENTED_EDGE('',*,*,#16351,.F.) ;
#22166 = ORIENTED_EDGE('',*,*,#16350,.F.) ;
#22167 = ORIENTED_EDGE('',*,*,#16352,.F.) ;
#22168 = ORIENTED_EDGE('',*,*,#16353,.T.) ;
#22169 = ORIENTED_EDGE('',*,*,#16354,.F.) ;
#22170 = ORIENTED_EDGE('',*,*,#16353,.F.) ;
#22171 = ORIENTED_EDGE('',*,*,#16355,.F.) ;
#22172 = ORIENTED_EDGE('',*,*,#16356,.T.) ;
#22173 = ORIENTED_EDGE('',*,*,#16357,.F.) ;
#22174 = ORIENTED_EDGE('',*,*,#16358,.F.) ;
#22175 = ORIENTED_EDGE('',*,*,#16359,.F.) ;
#22176 = ORIENTED_EDGE('',*,*,#16356,.F.) ;
#22177 = ORIENTED_EDGE('',*,*,#16358,.T.) ;
#22178 = ORIENTED_EDGE('',*,*,#16360,.T.) ;
#22179 = ORIENTED_EDGE('',*,*,#16361,.T.) ;
#22180 = ORIENTED_EDGE('',*,*,#16362,.T.) ;
#22181 = ORIENTED_EDGE('',*,*,#16363,.T.) ;
#22182 = ORIENTED_EDGE('',*,*,#16364,.T.) ;
#22183 = ORIENTED_EDGE('',*,*,#16365,.T.) ;
#22184 = ORIENTED_EDGE('',*,*,#16366,.T.) ;
#22185 = ORIENTED_EDGE('',*,*,#16367,.T.) ;
#22186 = ORIENTED_EDGE('',*,*,#16368,.T.) ;
#22187 = ORIENTED_EDGE('',*,*,#16369,.T.) ;
#22188 = ORIENTED_EDGE('',*,*,#16370,.T.) ;
#22189 = ORIENTED_EDGE('',*,*,#16371,.T.) ;
#22190 = ORIENTED_EDGE('',*,*,#16372,.T.) ;
#22191 = ORIENTED_EDGE('',*,*,#16373,.T.) ;
#22192 = ORIENTED_EDGE('',*,*,#16374,.T.) ;
#22193 = ORIENTED_EDGE('',*,*,#16375,.T.) ;
#22194 = ORIENTED_EDGE('',*,*,#16376,.T.) ;
#22195 = ORIENTED_EDGE('',*,*,#16377,.F.) ;
#22196 = ORIENTED_EDGE('',*,*,#16378,.F.) ;
#22197 = ORIENTED_EDGE('',*,*,#16379,.F.) ;
#22198 = ORIENTED_EDGE('',*,*,#16375,.F.) ;
#22199 = ORIENTED_EDGE('',*,*,#16380,.F.) ;
#22200 = ORIENTED_EDGE('',*,*,#16378,.T.) ;
#22201 = ORIENTED_EDGE('',*,*,#16355,.T.) ;
#22202 = ORIENTED_EDGE('',*,*,#16376,.F.) ;
#22203 = ORIENTED_EDGE('',*,*,#16379,.T.) ;
#22204 = ORIENTED_EDGE('',*,*,#16377,.T.) ;
#22205 = ORIENTED_EDGE('',*,*,#16380,.T.) ;
#22206 = ORIENTED_EDGE('',*,*,#16374,.F.) ;
#22207 = ORIENTED_EDGE('',*,*,#16381,.T.) ;
#22208 = ORIENTED_EDGE('',*,*,#16382,.F.) ;
#22209 = ORIENTED_EDGE('',*,*,#16383,.T.) ;
#22210 = ORIENTED_EDGE('',*,*,#16384,.F.) ;
#22211 = ORIENTED_EDGE('',*,*,#16385,.T.) ;
#22212 = ORIENTED_EDGE('',*,*,#16386,.F.) ;
#22213 = ORIENTED_EDGE('',*,*,#16387,.F.) ;
#22214 = ORIENTED_EDGE('',*,*,#16388,.F.) ;
#22215 = ORIENTED_EDGE('',*,*,#16389,.F.) ;
#22216 = ORIENTED_EDGE('',*,*,#16390,.F.) ;
#22217 = ORIENTED_EDGE('',*,*,#16391,.F.) ;
#22218 = ORIENTED_EDGE('',*,*,#16360,.F.) ;
#22219 = ORIENTED_EDGE('',*,*,#16357,.T.) ;
#22220 = ORIENTED_EDGE('',*,*,#16359,.T.) ;
#22221 = ORIENTED_EDGE('',*,*,#16392,.T.) ;
#22222 = ORIENTED_EDGE('',*,*,#16393,.F.) ;
#22223 = ORIENTED_EDGE('',*,*,#16394,.F.) ;
#22224 = ORIENTED_EDGE('',*,*,#16395,.F.) ;
#22225 = ORIENTED_EDGE('',*,*,#16369,.F.) ;
#22226 = ORIENTED_EDGE('',*,*,#16396,.F.) ;
#22227 = ORIENTED_EDGE('',*,*,#16394,.T.) ;
#22228 = ORIENTED_EDGE('',*,*,#16395,.T.) ;
#22229 = ORIENTED_EDGE('',*,*,#16393,.T.) ;
#22230 = ORIENTED_EDGE('',*,*,#16396,.T.) ;
#22231 = ORIENTED_EDGE('',*,*,#16368,.F.) ;
#22232 = ORIENTED_EDGE('',*,*,#16397,.T.) ;
#22233 = ORIENTED_EDGE('',*,*,#16398,.F.) ;
#22234 = ORIENTED_EDGE('',*,*,#16399,.T.) ;
#22235 = ORIENTED_EDGE('',*,*,#16400,.F.) ;
#22236 = ORIENTED_EDGE('',*,*,#16401,.T.) ;
#22237 = ORIENTED_EDGE('',*,*,#16402,.F.) ;
#22238 = ORIENTED_EDGE('',*,*,#16403,.F.) ;
#22239 = ORIENTED_EDGE('',*,*,#16404,.F.) ;
#22240 = ORIENTED_EDGE('',*,*,#16405,.F.) ;
#22241 = ORIENTED_EDGE('',*,*,#16406,.F.) ;
#22242 = ORIENTED_EDGE('',*,*,#16407,.F.) ;
#22243 = ORIENTED_EDGE('',*,*,#16372,.F.) ;
#22244 = ORIENTED_EDGE('',*,*,#16408,.T.) ;
#22245 = ORIENTED_EDGE('',*,*,#16409,.T.) ;
#22246 = ORIENTED_EDGE('',*,*,#16410,.T.) ;
#22247 = ORIENTED_EDGE('',*,*,#16370,.F.) ;
#22248 = ORIENTED_EDGE('',*,*,#16411,.T.) ;
#22249 = ORIENTED_EDGE('',*,*,#16409,.F.) ;
#22250 = ORIENTED_EDGE('',*,*,#16412,.F.) ;
#22251 = ORIENTED_EDGE('',*,*,#16408,.F.) ;
#22252 = ORIENTED_EDGE('',*,*,#16371,.F.) ;
#22253 = ORIENTED_EDGE('',*,*,#16410,.F.) ;
#22254 = ORIENTED_EDGE('',*,*,#16412,.T.) ;
#22255 = ORIENTED_EDGE('',*,*,#16413,.T.) ;
#22256 = ORIENTED_EDGE('',*,*,#16414,.T.) ;
#22257 = ORIENTED_EDGE('',*,*,#16415,.F.) ;
#22258 = ORIENTED_EDGE('',*,*,#16414,.F.) ;
#22259 = ORIENTED_EDGE('',*,*,#16413,.F.) ;
#22260 = ORIENTED_EDGE('',*,*,#16416,.F.) ;
#22261 = ORIENTED_EDGE('',*,*,#16417,.T.) ;
#22262 = ORIENTED_EDGE('',*,*,#16411,.F.) ;
#22263 = ORIENTED_EDGE('',*,*,#16417,.F.) ;
#22264 = ORIENTED_EDGE('',*,*,#16416,.T.) ;
#22265 = ORIENTED_EDGE('',*,*,#16415,.T.) ;
#22266 = ORIENTED_EDGE('',*,*,#16418,.F.) ;
#22267 = ORIENTED_EDGE('',*,*,#16419,.F.) ;
#22268 = ORIENTED_EDGE('',*,*,#16420,.F.) ;
#22269 = ORIENTED_EDGE('',*,*,#16421,.F.) ;
#22270 = ORIENTED_EDGE('',*,*,#16422,.F.) ;
#22271 = ORIENTED_EDGE('',*,*,#16423,.F.) ;
#22272 = ORIENTED_EDGE('',*,*,#16424,.F.) ;
#22273 = ORIENTED_EDGE('',*,*,#16425,.F.) ;
#22274 = ORIENTED_EDGE('',*,*,#16423,.T.) ;
#22275 = ORIENTED_EDGE('',*,*,#16426,.F.) ;
#22276 = ORIENTED_EDGE('',*,*,#16427,.F.) ;
#22277 = ORIENTED_EDGE('',*,*,#16428,.F.) ;
#22278 = ORIENTED_EDGE('',*,*,#16429,.T.) ;
#22279 = ORIENTED_EDGE('',*,*,#16430,.F.) ;
#22280 = ORIENTED_EDGE('',*,*,#16422,.T.) ;
#22281 = ORIENTED_EDGE('',*,*,#16431,.T.) ;
#22282 = ORIENTED_EDGE('',*,*,#16432,.T.) ;
#22283 = ORIENTED_EDGE('',*,*,#16426,.T.) ;
#22284 = ORIENTED_EDGE('',*,*,#16424,.T.) ;
#22285 = ORIENTED_EDGE('',*,*,#16430,.T.) ;
#22286 = ORIENTED_EDGE('',*,*,#16433,.T.) ;
#22287 = ORIENTED_EDGE('',*,*,#16434,.T.) ;
#22288 = ORIENTED_EDGE('',*,*,#16419,.T.) ;
#22289 = ORIENTED_EDGE('',*,*,#16435,.F.) ;
#22290 = ORIENTED_EDGE('',*,*,#16436,.F.) ;
#22291 = ORIENTED_EDGE('',*,*,#16437,.F.) ;
#22292 = ORIENTED_EDGE('',*,*,#16438,.T.) ;
#22293 = ORIENTED_EDGE('',*,*,#16439,.F.) ;
#22294 = ORIENTED_EDGE('',*,*,#16418,.T.) ;
#22295 = ORIENTED_EDGE('',*,*,#16440,.T.) ;
#22296 = ORIENTED_EDGE('',*,*,#16441,.T.) ;
#22297 = ORIENTED_EDGE('',*,*,#16435,.T.) ;
#22298 = ORIENTED_EDGE('',*,*,#16420,.T.) ;
#22299 = ORIENTED_EDGE('',*,*,#16439,.T.) ;
#22300 = ORIENTED_EDGE('',*,*,#16442,.T.) ;
#22301 = ORIENTED_EDGE('',*,*,#16443,.T.) ;
#22302 = ORIENTED_EDGE('',*,*,#16427,.T.) ;
#22303 = ORIENTED_EDGE('',*,*,#16432,.F.) ;
#22304 = ORIENTED_EDGE('',*,*,#16444,.F.) ;
#22305 = ORIENTED_EDGE('',*,*,#16445,.F.) ;
#22306 = ORIENTED_EDGE('',*,*,#16446,.T.) ;
#22307 = ORIENTED_EDGE('',*,*,#16433,.F.) ;
#22308 = ORIENTED_EDGE('',*,*,#16429,.F.) ;
#22309 = ORIENTED_EDGE('',*,*,#16447,.F.) ;
#22310 = ORIENTED_EDGE('',*,*,#16425,.T.) ;
#22311 = ORIENTED_EDGE('',*,*,#16434,.F.) ;
#22312 = ORIENTED_EDGE('',*,*,#16446,.F.) ;
#22313 = ORIENTED_EDGE('',*,*,#16448,.F.) ;
#22314 = ORIENTED_EDGE('',*,*,#16444,.T.) ;
#22315 = ORIENTED_EDGE('',*,*,#16431,.F.) ;
#22316 = ORIENTED_EDGE('',*,*,#16436,.T.) ;
#22317 = ORIENTED_EDGE('',*,*,#16441,.F.) ;
#22318 = ORIENTED_EDGE('',*,*,#16449,.F.) ;
#22319 = ORIENTED_EDGE('',*,*,#16450,.F.) ;
#22320 = ORIENTED_EDGE('',*,*,#16451,.T.) ;
#22321 = ORIENTED_EDGE('',*,*,#16442,.F.) ;
#22322 = ORIENTED_EDGE('',*,*,#16438,.F.) ;
#22323 = ORIENTED_EDGE('',*,*,#16452,.F.) ;
#22324 = ORIENTED_EDGE('',*,*,#16421,.T.) ;
#22325 = ORIENTED_EDGE('',*,*,#16443,.F.) ;
#22326 = ORIENTED_EDGE('',*,*,#16451,.F.) ;
#22327 = ORIENTED_EDGE('',*,*,#16453,.F.) ;
#22328 = ORIENTED_EDGE('',*,*,#16449,.T.) ;
#22329 = ORIENTED_EDGE('',*,*,#16440,.F.) ;
#22330 = ORIENTED_EDGE('',*,*,#16454,.F.) ;
#22331 = ORIENTED_EDGE('',*,*,#16455,.F.) ;
#22332 = ORIENTED_EDGE('',*,*,#16456,.F.) ;
#22333 = ORIENTED_EDGE('',*,*,#16457,.T.) ;
#22334 = ORIENTED_EDGE('',*,*,#16364,.F.) ;
#22335 = ORIENTED_EDGE('',*,*,#16458,.F.) ;
#22336 = ORIENTED_EDGE('',*,*,#16455,.T.) ;
#22337 = ORIENTED_EDGE('',*,*,#16459,.F.) ;
#22338 = ORIENTED_EDGE('',*,*,#16365,.F.) ;
#22339 = ORIENTED_EDGE('',*,*,#16457,.F.) ;
#22340 = ORIENTED_EDGE('',*,*,#16460,.F.) ;
#22341 = ORIENTED_EDGE('',*,*,#16461,.T.) ;
#22342 = ORIENTED_EDGE('',*,*,#16362,.F.) ;
#22343 = ORIENTED_EDGE('',*,*,#16366,.F.) ;
#22344 = ORIENTED_EDGE('',*,*,#16459,.T.) ;
#22345 = ORIENTED_EDGE('',*,*,#16454,.T.) ;
#22346 = ORIENTED_EDGE('',*,*,#16458,.T.) ;
#22347 = ORIENTED_EDGE('',*,*,#16363,.F.) ;
#22348 = ORIENTED_EDGE('',*,*,#16461,.F.) ;
#22349 = ORIENTED_EDGE('',*,*,#16462,.T.) ;
#22350 = ORIENTED_EDGE('',*,*,#16463,.T.) ;
#22351 = ORIENTED_EDGE('',*,*,#16464,.F.) ;
#22352 = ORIENTED_EDGE('',*,*,#16463,.F.) ;
#22353 = ORIENTED_EDGE('',*,*,#16462,.F.) ;
#22354 = ORIENTED_EDGE('',*,*,#16460,.T.) ;
#22355 = ORIENTED_EDGE('',*,*,#16464,.T.) ;
#22356 = ORIENTED_EDGE('',*,*,#16465,.F.) ;
#22357 = ORIENTED_EDGE('',*,*,#16466,.T.) ;
#22358 = ORIENTED_EDGE('',*,*,#16467,.T.) ;
#22359 = ORIENTED_EDGE('',*,*,#16466,.F.) ;
#22360 = ORIENTED_EDGE('',*,*,#16467,.F.) ;
#22361 = ORIENTED_EDGE('',*,*,#16468,.F.) ;
#22362 = ORIENTED_EDGE('',*,*,#16469,.T.) ;
#22363 = ORIENTED_EDGE('',*,*,#16470,.F.) ;
#22364 = ORIENTED_EDGE('',*,*,#16469,.F.) ;
#22365 = ORIENTED_EDGE('',*,*,#16470,.T.) ;
#22366 = ORIENTED_EDGE('',*,*,#16465,.T.) ;
#22367 = ORIENTED_EDGE('',*,*,#16471,.F.) ;
#22368 = ORIENTED_EDGE('',*,*,#16472,.T.) ;
#22369 = ORIENTED_EDGE('',*,*,#16473,.T.) ;
#22370 = ORIENTED_EDGE('',*,*,#16472,.F.) ;
#22371 = ORIENTED_EDGE('',*,*,#16473,.F.) ;
#22372 = ORIENTED_EDGE('',*,*,#16392,.F.) ;
#22373 = ORIENTED_EDGE('',*,*,#16474,.T.) ;
#22374 = ORIENTED_EDGE('',*,*,#16475,.F.) ;
#22375 = ORIENTED_EDGE('',*,*,#16474,.F.) ;
#22376 = ORIENTED_EDGE('',*,*,#16475,.T.) ;
#22377 = ORIENTED_EDGE('',*,*,#16471,.T.) ;
#22378 = ORIENTED_EDGE('',*,*,#16476,.T.) ;
#22379 = ORIENTED_EDGE('',*,*,#16477,.F.) ;
#22380 = ORIENTED_EDGE('',*,*,#16390,.T.) ;
#22381 = ORIENTED_EDGE('',*,*,#16478,.T.) ;
#22382 = ORIENTED_EDGE('',*,*,#16345,.T.) ;
#22383 = ORIENTED_EDGE('',*,*,#16479,.T.) ;
#22384 = ORIENTED_EDGE('',*,*,#16480,.T.) ;
#22385 = ORIENTED_EDGE('',*,*,#16388,.T.) ;
#22386 = ORIENTED_EDGE('',*,*,#16481,.F.) ;
#22387 = ORIENTED_EDGE('',*,*,#16343,.T.) ;
#22388 = ORIENTED_EDGE('',*,*,#16389,.T.) ;
#22389 = ORIENTED_EDGE('',*,*,#16480,.F.) ;
#22390 = ORIENTED_EDGE('',*,*,#16482,.F.) ;
#22391 = ORIENTED_EDGE('',*,*,#16478,.F.) ;
#22392 = ORIENTED_EDGE('',*,*,#16482,.T.) ;
#22393 = ORIENTED_EDGE('',*,*,#16479,.F.) ;
#22394 = ORIENTED_EDGE('',*,*,#16483,.F.) ;
#22395 = ORIENTED_EDGE('',*,*,#16476,.F.) ;
#22396 = ORIENTED_EDGE('',*,*,#16477,.T.) ;
#22397 = ORIENTED_EDGE('',*,*,#16483,.T.) ;
#22398 = ORIENTED_EDGE('',*,*,#16481,.T.) ;
#22399 = ORIENTED_EDGE('',*,*,#16387,.T.) ;
#22400 = ORIENTED_EDGE('',*,*,#16484,.F.) ;
#22401 = ORIENTED_EDGE('',*,*,#16401,.F.) ;
#22402 = ORIENTED_EDGE('',*,*,#16485,.T.) ;
#22403 = ORIENTED_EDGE('',*,*,#16486,.T.) ;
#22404 = ORIENTED_EDGE('',*,*,#16487,.T.) ;
#22405 = ORIENTED_EDGE('',*,*,#16397,.F.) ;
#22406 = ORIENTED_EDGE('',*,*,#16367,.F.) ;
#22407 = ORIENTED_EDGE('',*,*,#16361,.F.) ;
#22408 = ORIENTED_EDGE('',*,*,#16391,.T.) ;
#22409 = ORIENTED_EDGE('',*,*,#16468,.T.) ;
#22410 = ORIENTED_EDGE('',*,*,#16488,.T.) ;
#22411 = ORIENTED_EDGE('',*,*,#16489,.T.) ;
#22412 = ORIENTED_EDGE('',*,*,#16382,.T.) ;
#22413 = ORIENTED_EDGE('',*,*,#16490,.F.) ;
#22414 = ORIENTED_EDGE('',*,*,#16348,.T.) ;
#22415 = ORIENTED_EDGE('',*,*,#16491,.T.) ;
#22416 = ORIENTED_EDGE('',*,*,#16492,.F.) ;
#22417 = ORIENTED_EDGE('',*,*,#16384,.T.) ;
#22418 = ORIENTED_EDGE('',*,*,#16493,.T.) ;
#22419 = ORIENTED_EDGE('',*,*,#16346,.T.) ;
#22420 = ORIENTED_EDGE('',*,*,#16494,.T.) ;
#22421 = ORIENTED_EDGE('',*,*,#16493,.F.) ;
#22422 = ORIENTED_EDGE('',*,*,#16383,.F.) ;
#22423 = ORIENTED_EDGE('',*,*,#16489,.F.) ;
#22424 = ORIENTED_EDGE('',*,*,#16495,.F.) ;
#22425 = ORIENTED_EDGE('',*,*,#16491,.F.) ;
#22426 = ORIENTED_EDGE('',*,*,#16494,.F.) ;
#22427 = ORIENTED_EDGE('',*,*,#16488,.F.) ;
#22428 = ORIENTED_EDGE('',*,*,#16398,.T.) ;
#22429 = ORIENTED_EDGE('',*,*,#16487,.F.) ;
#22430 = ORIENTED_EDGE('',*,*,#16496,.T.) ;
#22431 = ORIENTED_EDGE('',*,*,#16497,.T.) ;
#22432 = ORIENTED_EDGE('',*,*,#16351,.T.) ;
#22433 = ORIENTED_EDGE('',*,*,#16400,.T.) ;
#22434 = ORIENTED_EDGE('',*,*,#16498,.T.) ;
#22435 = ORIENTED_EDGE('',*,*,#16499,.T.) ;
#22436 = ORIENTED_EDGE('',*,*,#16485,.F.) ;
#22437 = ORIENTED_EDGE('',*,*,#16349,.T.) ;
#22438 = ORIENTED_EDGE('',*,*,#16500,.T.) ;
#22439 = ORIENTED_EDGE('',*,*,#16498,.F.) ;
#22440 = ORIENTED_EDGE('',*,*,#16399,.F.) ;
#22441 = ORIENTED_EDGE('',*,*,#16497,.F.) ;
#22442 = ORIENTED_EDGE('',*,*,#16486,.F.) ;
#22443 = ORIENTED_EDGE('',*,*,#16499,.F.) ;
#22444 = ORIENTED_EDGE('',*,*,#16500,.F.) ;
#22445 = ORIENTED_EDGE('',*,*,#16496,.F.) ;
#22446 = ORIENTED_EDGE('',*,*,#16406,.T.) ;
#22447 = ORIENTED_EDGE('',*,*,#16501,.T.) ;
#22448 = ORIENTED_EDGE('',*,*,#16502,.T.) ;
#22449 = ORIENTED_EDGE('',*,*,#16503,.F.) ;
#22450 = ORIENTED_EDGE('',*,*,#16354,.T.) ;
#22451 = ORIENTED_EDGE('',*,*,#16404,.T.) ;
#22452 = ORIENTED_EDGE('',*,*,#16504,.F.) ;
#22453 = ORIENTED_EDGE('',*,*,#16505,.T.) ;
#22454 = ORIENTED_EDGE('',*,*,#16506,.T.) ;
#22455 = ORIENTED_EDGE('',*,*,#16352,.T.) ;
#22456 = ORIENTED_EDGE('',*,*,#16507,.T.) ;
#22457 = ORIENTED_EDGE('',*,*,#16505,.F.) ;
#22458 = ORIENTED_EDGE('',*,*,#16508,.F.) ;
#22459 = ORIENTED_EDGE('',*,*,#16502,.F.) ;
#22460 = ORIENTED_EDGE('',*,*,#16405,.T.) ;
#22461 = ORIENTED_EDGE('',*,*,#16506,.F.) ;
#22462 = ORIENTED_EDGE('',*,*,#16507,.F.) ;
#22463 = ORIENTED_EDGE('',*,*,#16501,.F.) ;
#22464 = ORIENTED_EDGE('',*,*,#16490,.T.) ;
#22465 = ORIENTED_EDGE('',*,*,#16381,.F.) ;
#22466 = ORIENTED_EDGE('',*,*,#16373,.F.) ;
#22467 = ORIENTED_EDGE('',*,*,#16407,.T.) ;
#22468 = ORIENTED_EDGE('',*,*,#16503,.T.) ;
#22469 = ORIENTED_EDGE('',*,*,#16508,.T.) ;
#22470 = ORIENTED_EDGE('',*,*,#16504,.T.) ;
#22471 = ORIENTED_EDGE('',*,*,#16403,.T.) ;
#22472 = ORIENTED_EDGE('',*,*,#16509,.F.) ;
#22473 = ORIENTED_EDGE('',*,*,#16385,.F.) ;
#22474 = ORIENTED_EDGE('',*,*,#16492,.T.) ;
#22475 = ORIENTED_EDGE('',*,*,#16495,.T.) ;
#22476 = ORIENTED_EDGE('',*,*,#16402,.T.) ;
#22477 = ORIENTED_EDGE('',*,*,#16484,.T.) ;
#22478 = ORIENTED_EDGE('',*,*,#16386,.T.) ;
#22479 = ORIENTED_EDGE('',*,*,#16509,.T.) ;
#22480 = ORIENTED_EDGE('',*,*,#16445,.T.) ;
#22481 = ORIENTED_EDGE('',*,*,#16448,.T.) ;
#22482 = ORIENTED_EDGE('',*,*,#16447,.T.) ;
#22483 = ORIENTED_EDGE('',*,*,#16428,.T.) ;
#22484 = ORIENTED_EDGE('',*,*,#16450,.T.) ;
#22485 = ORIENTED_EDGE('',*,*,#16453,.T.) ;
#22486 = ORIENTED_EDGE('',*,*,#16452,.T.) ;
#22487 = ORIENTED_EDGE('',*,*,#16437,.T.) ;
#22488 = ORIENTED_EDGE('',*,*,#16456,.T.) ;
#22489 = ORIENTED_EDGE('',*,*,#16510,.F.) ;
#22490 = ORIENTED_EDGE('',*,*,#16511,.T.) ;
#22491 = ORIENTED_EDGE('',*,*,#16512,.F.) ;
#22492 = ORIENTED_EDGE('',*,*,#16511,.F.) ;
#22493 = ORIENTED_EDGE('',*,*,#16512,.T.) ;
#22494 = ORIENTED_EDGE('',*,*,#16513,.F.) ;
#22495 = ORIENTED_EDGE('',*,*,#16514,.T.) ;
#22496 = ORIENTED_EDGE('',*,*,#16515,.F.) ;
#22497 = ORIENTED_EDGE('',*,*,#16516,.T.) ;
#22498 = ORIENTED_EDGE('',*,*,#16517,.F.) ;
#22499 = ORIENTED_EDGE('',*,*,#16518,.T.) ;
#22500 = ORIENTED_EDGE('',*,*,#16519,.F.) ;
#22501 = ORIENTED_EDGE('',*,*,#16520,.T.) ;
#22502 = ORIENTED_EDGE('',*,*,#16514,.F.) ;
#22503 = ORIENTED_EDGE('',*,*,#16521,.F.) ;
#22504 = ORIENTED_EDGE('',*,*,#16522,.F.) ;
#22505 = ORIENTED_EDGE('',*,*,#16518,.F.) ;
#22506 = ORIENTED_EDGE('',*,*,#16523,.F.) ;
#22507 = ORIENTED_EDGE('',*,*,#16524,.F.) ;
#22508 = ORIENTED_EDGE('',*,*,#16510,.T.) ;
#22509 = ORIENTED_EDGE('',*,*,#16525,.F.) ;
#22510 = ORIENTED_EDGE('',*,*,#16521,.T.) ;
#22511 = ORIENTED_EDGE('',*,*,#16513,.T.) ;
#22512 = ORIENTED_EDGE('',*,*,#16526,.T.) ;
#22513 = ORIENTED_EDGE('',*,*,#16527,.F.) ;
#22514 = ORIENTED_EDGE('',*,*,#16523,.T.) ;
#22515 = ORIENTED_EDGE('',*,*,#16517,.T.) ;
#22516 = ORIENTED_EDGE('',*,*,#16528,.T.) ;
#22517 = ORIENTED_EDGE('',*,*,#16519,.T.) ;
#22518 = ORIENTED_EDGE('',*,*,#16522,.T.) ;
#22519 = ORIENTED_EDGE('',*,*,#16525,.T.) ;
#22520 = ORIENTED_EDGE('',*,*,#16529,.T.) ;
#22521 = ORIENTED_EDGE('',*,*,#16527,.T.) ;
#22522 = ORIENTED_EDGE('',*,*,#16530,.T.) ;
#22523 = ORIENTED_EDGE('',*,*,#16515,.T.) ;
#22524 = ORIENTED_EDGE('',*,*,#16524,.T.) ;
#22525 = ORIENTED_EDGE('',*,*,#16516,.F.) ;
#22526 = ORIENTED_EDGE('',*,*,#16530,.F.) ;
#22527 = ORIENTED_EDGE('',*,*,#16528,.F.) ;
#22528 = ORIENTED_EDGE('',*,*,#16520,.F.) ;
#22529 = ORIENTED_EDGE('',*,*,#16529,.F.) ;
#22530 = ORIENTED_EDGE('',*,*,#16526,.F.) ;
#22531 = ORIENTED_EDGE('',*,*,#16531,.F.) ;
#22532 = ORIENTED_EDGE('',*,*,#16532,.F.) ;
#22533 = ORIENTED_EDGE('',*,*,#16533,.F.) ;
#22534 = ORIENTED_EDGE('',*,*,#16534,.F.) ;
#22535 = ORIENTED_EDGE('',*,*,#16535,.F.) ;
#22536 = ORIENTED_EDGE('',*,*,#16536,.F.) ;
#22537 = ORIENTED_EDGE('',*,*,#16537,.F.) ;
#22538 = ORIENTED_EDGE('',*,*,#16538,.F.) ;
#22539 = ORIENTED_EDGE('',*,*,#16539,.F.) ;
#22540 = ORIENTED_EDGE('',*,*,#16540,.F.) ;
#22541 = ORIENTED_EDGE('',*,*,#16541,.F.) ;
#22542 = ORIENTED_EDGE('',*,*,#16542,.F.) ;
#22543 = ORIENTED_EDGE('',*,*,#16543,.F.) ;
#22544 = ORIENTED_EDGE('',*,*,#16544,.F.) ;
#22545 = ORIENTED_EDGE('',*,*,#16545,.F.) ;
#22546 = ORIENTED_EDGE('',*,*,#16546,.F.) ;
#22547 = ORIENTED_EDGE('',*,*,#16547,.F.) ;
#22548 = ORIENTED_EDGE('',*,*,#16548,.F.) ;
#22549 = ORIENTED_EDGE('',*,*,#16549,.F.) ;
#22550 = ORIENTED_EDGE('',*,*,#16550,.F.) ;
#22551 = ORIENTED_EDGE('',*,*,#16551,.F.) ;
#22552 = ORIENTED_EDGE('',*,*,#16552,.F.) ;
#22553 = ORIENTED_EDGE('',*,*,#16553,.F.) ;
#22554 = ORIENTED_EDGE('',*,*,#16554,.F.) ;
#22555 = ORIENTED_EDGE('',*,*,#16555,.F.) ;
#22556 = ORIENTED_EDGE('',*,*,#16556,.F.) ;
#22557 = ORIENTED_EDGE('',*,*,#16557,.F.) ;
#22558 = ORIENTED_EDGE('',*,*,#16558,.F.) ;
#22559 = ORIENTED_EDGE('',*,*,#16559,.F.) ;
#22560 = ORIENTED_EDGE('',*,*,#16560,.T.) ;
#22561 = ORIENTED_EDGE('',*,*,#16561,.F.) ;
#22562 = ORIENTED_EDGE('',*,*,#16546,.T.) ;
#22563 = ORIENTED_EDGE('',*,*,#16562,.F.) ;
#22564 = ORIENTED_EDGE('',*,*,#16563,.T.) ;
#22565 = ORIENTED_EDGE('',*,*,#16564,.F.) ;
#22566 = ORIENTED_EDGE('',*,*,#16542,.T.) ;
#22567 = ORIENTED_EDGE('',*,*,#16565,.F.) ;
#22568 = ORIENTED_EDGE('',*,*,#16535,.T.) ;
#22569 = ORIENTED_EDGE('',*,*,#16566,.F.) ;
#22570 = ORIENTED_EDGE('',*,*,#16567,.T.) ;
#22571 = ORIENTED_EDGE('',*,*,#16568,.F.) ;
#22572 = ORIENTED_EDGE('',*,*,#16569,.T.) ;
#22573 = ORIENTED_EDGE('',*,*,#16570,.F.) ;
#22574 = ORIENTED_EDGE('',*,*,#16537,.T.) ;
#22575 = ORIENTED_EDGE('',*,*,#16571,.F.) ;
#22576 = ORIENTED_EDGE('',*,*,#16572,.T.) ;
#22577 = ORIENTED_EDGE('',*,*,#16573,.F.) ;
#22578 = ORIENTED_EDGE('',*,*,#16551,.T.) ;
#22579 = ORIENTED_EDGE('',*,*,#16574,.F.) ;
#22580 = ORIENTED_EDGE('',*,*,#16575,.T.) ;
#22581 = ORIENTED_EDGE('',*,*,#16576,.F.) ;
#22582 = ORIENTED_EDGE('',*,*,#16556,.T.) ;
#22583 = ORIENTED_EDGE('',*,*,#16577,.F.) ;
#22584 = ORIENTED_EDGE('',*,*,#16567,.F.) ;
#22585 = ORIENTED_EDGE('',*,*,#16578,.F.) ;
#22586 = ORIENTED_EDGE('',*,*,#16579,.F.) ;
#22587 = ORIENTED_EDGE('',*,*,#16580,.F.) ;
#22588 = ORIENTED_EDGE('',*,*,#16581,.F.) ;
#22589 = ORIENTED_EDGE('',*,*,#16582,.F.) ;
#22590 = ORIENTED_EDGE('',*,*,#16583,.F.) ;
#22591 = ORIENTED_EDGE('',*,*,#16584,.F.) ;
#22592 = ORIENTED_EDGE('',*,*,#16563,.F.) ;
#22593 = ORIENTED_EDGE('',*,*,#16585,.F.) ;
#22594 = ORIENTED_EDGE('',*,*,#16586,.F.) ;
#22595 = ORIENTED_EDGE('',*,*,#16587,.F.) ;
#22596 = ORIENTED_EDGE('',*,*,#16588,.F.) ;
#22597 = ORIENTED_EDGE('',*,*,#16560,.F.) ;
#22598 = ORIENTED_EDGE('',*,*,#16589,.F.) ;
#22599 = ORIENTED_EDGE('',*,*,#16590,.F.) ;
#22600 = ORIENTED_EDGE('',*,*,#16591,.F.) ;
#22601 = ORIENTED_EDGE('',*,*,#16592,.F.) ;
#22602 = ORIENTED_EDGE('',*,*,#16572,.F.) ;
#22603 = ORIENTED_EDGE('',*,*,#16593,.F.) ;
#22604 = ORIENTED_EDGE('',*,*,#16594,.F.) ;
#22605 = ORIENTED_EDGE('',*,*,#16595,.F.) ;
#22606 = ORIENTED_EDGE('',*,*,#16596,.F.) ;
#22607 = ORIENTED_EDGE('',*,*,#16569,.F.) ;
#22608 = ORIENTED_EDGE('',*,*,#16597,.F.) ;
#22609 = ORIENTED_EDGE('',*,*,#16598,.F.) ;
#22610 = ORIENTED_EDGE('',*,*,#16599,.F.) ;
#22611 = ORIENTED_EDGE('',*,*,#16575,.F.) ;
#22612 = ORIENTED_EDGE('',*,*,#16597,.T.) ;
#22613 = ORIENTED_EDGE('',*,*,#16574,.T.) ;
#22614 = ORIENTED_EDGE('',*,*,#16555,.T.) ;
#22615 = ORIENTED_EDGE('',*,*,#16600,.F.) ;
#22616 = ORIENTED_EDGE('',*,*,#16601,.F.) ;
#22617 = ORIENTED_EDGE('',*,*,#16602,.F.) ;
#22618 = ORIENTED_EDGE('',*,*,#16603,.F.) ;
#22619 = ORIENTED_EDGE('',*,*,#16604,.F.) ;
#22620 = ORIENTED_EDGE('',*,*,#16593,.T.) ;
#22621 = ORIENTED_EDGE('',*,*,#16568,.T.) ;
#22622 = ORIENTED_EDGE('',*,*,#16536,.T.) ;
#22623 = ORIENTED_EDGE('',*,*,#16605,.F.) ;
#22624 = ORIENTED_EDGE('',*,*,#16606,.F.) ;
#22625 = ORIENTED_EDGE('',*,*,#16607,.F.) ;
#22626 = ORIENTED_EDGE('',*,*,#16608,.F.) ;
#22627 = ORIENTED_EDGE('',*,*,#16609,.F.) ;
#22628 = ORIENTED_EDGE('',*,*,#16539,.T.) ;
#22629 = ORIENTED_EDGE('',*,*,#16610,.F.) ;
#22630 = ORIENTED_EDGE('',*,*,#16611,.F.) ;
#22631 = ORIENTED_EDGE('',*,*,#16612,.F.) ;
#22632 = ORIENTED_EDGE('',*,*,#16552,.T.) ;
#22633 = ORIENTED_EDGE('',*,*,#16573,.T.) ;
#22634 = ORIENTED_EDGE('',*,*,#16592,.T.) ;
#22635 = ORIENTED_EDGE('',*,*,#16613,.T.) ;
#22636 = ORIENTED_EDGE('',*,*,#16614,.T.) ;
#22637 = ORIENTED_EDGE('',*,*,#16602,.T.) ;
#22638 = ORIENTED_EDGE('',*,*,#16615,.F.) ;
#22639 = ORIENTED_EDGE('',*,*,#16616,.T.) ;
#22640 = ORIENTED_EDGE('',*,*,#16591,.T.) ;
#22641 = ORIENTED_EDGE('',*,*,#16617,.F.) ;
#22642 = ORIENTED_EDGE('',*,*,#16618,.F.) ;
#22643 = ORIENTED_EDGE('',*,*,#16613,.F.) ;
#22644 = ORIENTED_EDGE('',*,*,#16553,.T.) ;
#22645 = ORIENTED_EDGE('',*,*,#16616,.F.) ;
#22646 = ORIENTED_EDGE('',*,*,#16619,.F.) ;
#22647 = ORIENTED_EDGE('',*,*,#16620,.F.) ;
#22648 = ORIENTED_EDGE('',*,*,#16531,.T.) ;
#22649 = ORIENTED_EDGE('',*,*,#16565,.T.) ;
#22650 = ORIENTED_EDGE('',*,*,#16577,.T.) ;
#22651 = ORIENTED_EDGE('',*,*,#16621,.F.) ;
#22652 = ORIENTED_EDGE('',*,*,#16622,.F.) ;
#22653 = ORIENTED_EDGE('',*,*,#16623,.F.) ;
#22654 = ORIENTED_EDGE('',*,*,#16624,.F.) ;
#22655 = ORIENTED_EDGE('',*,*,#16625,.F.) ;
#22656 = ORIENTED_EDGE('',*,*,#16579,.T.) ;
#22657 = ORIENTED_EDGE('',*,*,#16626,.F.) ;
#22658 = ORIENTED_EDGE('',*,*,#16627,.F.) ;
#22659 = ORIENTED_EDGE('',*,*,#16628,.F.) ;
#22660 = ORIENTED_EDGE('',*,*,#16547,.T.) ;
#22661 = ORIENTED_EDGE('',*,*,#16561,.T.) ;
#22662 = ORIENTED_EDGE('',*,*,#16588,.T.) ;
#22663 = ORIENTED_EDGE('',*,*,#16629,.F.) ;
#22664 = ORIENTED_EDGE('',*,*,#16630,.F.) ;
#22665 = ORIENTED_EDGE('',*,*,#16631,.F.) ;
#22666 = ORIENTED_EDGE('',*,*,#16632,.F.) ;
#22667 = ORIENTED_EDGE('',*,*,#16633,.F.) ;
#22668 = ORIENTED_EDGE('',*,*,#16586,.T.) ;
#22669 = ORIENTED_EDGE('',*,*,#16634,.F.) ;
#22670 = ORIENTED_EDGE('',*,*,#16635,.F.) ;
#22671 = ORIENTED_EDGE('',*,*,#16636,.F.) ;
#22672 = ORIENTED_EDGE('',*,*,#16549,.T.) ;
#22673 = ORIENTED_EDGE('',*,*,#16637,.F.) ;
#22674 = ORIENTED_EDGE('',*,*,#16638,.F.) ;
#22675 = ORIENTED_EDGE('',*,*,#16639,.F.) ;
#22676 = ORIENTED_EDGE('',*,*,#16543,.T.) ;
#22677 = ORIENTED_EDGE('',*,*,#16564,.T.) ;
#22678 = ORIENTED_EDGE('',*,*,#16584,.T.) ;
#22679 = ORIENTED_EDGE('',*,*,#16640,.F.) ;
#22680 = ORIENTED_EDGE('',*,*,#16641,.F.) ;
#22681 = ORIENTED_EDGE('',*,*,#16642,.F.) ;
#22682 = ORIENTED_EDGE('',*,*,#16643,.F.) ;
#22683 = ORIENTED_EDGE('',*,*,#16644,.F.) ;
#22684 = ORIENTED_EDGE('',*,*,#16544,.T.) ;
#22685 = ORIENTED_EDGE('',*,*,#16644,.T.) ;
#22686 = ORIENTED_EDGE('',*,*,#16645,.F.) ;
#22687 = ORIENTED_EDGE('',*,*,#16646,.T.) ;
#22688 = ORIENTED_EDGE('',*,*,#16548,.T.) ;
#22689 = ORIENTED_EDGE('',*,*,#16633,.T.) ;
#22690 = ORIENTED_EDGE('',*,*,#16647,.F.) ;
#22691 = ORIENTED_EDGE('',*,*,#16637,.T.) ;
#22692 = ORIENTED_EDGE('',*,*,#16554,.T.) ;
#22693 = ORIENTED_EDGE('',*,*,#16620,.T.) ;
#22694 = ORIENTED_EDGE('',*,*,#16648,.F.) ;
#22695 = ORIENTED_EDGE('',*,*,#16649,.T.) ;
#22696 = ORIENTED_EDGE('',*,*,#16532,.T.) ;
#22697 = ORIENTED_EDGE('',*,*,#16625,.T.) ;
#22698 = ORIENTED_EDGE('',*,*,#16650,.F.) ;
#22699 = ORIENTED_EDGE('',*,*,#16651,.T.) ;
#22700 = ORIENTED_EDGE('',*,*,#16540,.T.) ;
#22701 = ORIENTED_EDGE('',*,*,#16612,.T.) ;
#22702 = ORIENTED_EDGE('',*,*,#16652,.F.) ;
#22703 = ORIENTED_EDGE('',*,*,#16605,.T.) ;
#22704 = ORIENTED_EDGE('',*,*,#16558,.T.) ;
#22705 = ORIENTED_EDGE('',*,*,#16653,.T.) ;
#22706 = ORIENTED_EDGE('',*,*,#16654,.F.) ;
#22707 = ORIENTED_EDGE('',*,*,#16600,.T.) ;
#22708 = ORIENTED_EDGE('',*,*,#16655,.F.) ;
#22709 = ORIENTED_EDGE('',*,*,#16603,.T.) ;
#22710 = ORIENTED_EDGE('',*,*,#16614,.F.) ;
#22711 = ORIENTED_EDGE('',*,*,#16618,.T.) ;
#22712 = ORIENTED_EDGE('',*,*,#16619,.T.) ;
#22713 = ORIENTED_EDGE('',*,*,#16615,.T.) ;
#22714 = ORIENTED_EDGE('',*,*,#16601,.T.) ;
#22715 = ORIENTED_EDGE('',*,*,#16654,.T.) ;
#22716 = ORIENTED_EDGE('',*,*,#16656,.T.) ;
#22717 = ORIENTED_EDGE('',*,*,#16657,.T.) ;
#22718 = ORIENTED_EDGE('',*,*,#16658,.T.) ;
#22719 = ORIENTED_EDGE('',*,*,#16650,.T.) ;
#22720 = ORIENTED_EDGE('',*,*,#16624,.T.) ;
#22721 = ORIENTED_EDGE('',*,*,#16659,.T.) ;
#22722 = ORIENTED_EDGE('',*,*,#16606,.T.) ;
#22723 = ORIENTED_EDGE('',*,*,#16652,.T.) ;
#22724 = ORIENTED_EDGE('',*,*,#16611,.T.) ;
#22725 = ORIENTED_EDGE('',*,*,#16660,.T.) ;
#22726 = ORIENTED_EDGE('',*,*,#16661,.T.) ;
#22727 = ORIENTED_EDGE('',*,*,#16645,.T.) ;
#22728 = ORIENTED_EDGE('',*,*,#16643,.T.) ;
#22729 = ORIENTED_EDGE('',*,*,#16662,.T.) ;
#22730 = ORIENTED_EDGE('',*,*,#16638,.T.) ;
#22731 = ORIENTED_EDGE('',*,*,#16647,.T.) ;
#22732 = ORIENTED_EDGE('',*,*,#16632,.T.) ;
#22733 = ORIENTED_EDGE('',*,*,#16663,.T.) ;
#22734 = ORIENTED_EDGE('',*,*,#16664,.T.) ;
#22735 = ORIENTED_EDGE('',*,*,#16648,.T.) ;
#22736 = ORIENTED_EDGE('',*,*,#16599,.T.) ;
#22737 = ORIENTED_EDGE('',*,*,#16665,.F.) ;
#22738 = ORIENTED_EDGE('',*,*,#16666,.F.) ;
#22739 = ORIENTED_EDGE('',*,*,#16667,.F.) ;
#22740 = ORIENTED_EDGE('',*,*,#16656,.F.) ;
#22741 = ORIENTED_EDGE('',*,*,#16653,.F.) ;
#22742 = ORIENTED_EDGE('',*,*,#16557,.T.) ;
#22743 = ORIENTED_EDGE('',*,*,#16576,.T.) ;
#22744 = ORIENTED_EDGE('',*,*,#16533,.T.) ;
#22745 = ORIENTED_EDGE('',*,*,#16651,.F.) ;
#22746 = ORIENTED_EDGE('',*,*,#16658,.F.) ;
#22747 = ORIENTED_EDGE('',*,*,#16668,.F.) ;
#22748 = ORIENTED_EDGE('',*,*,#16534,.T.) ;
#22749 = ORIENTED_EDGE('',*,*,#16668,.T.) ;
#22750 = ORIENTED_EDGE('',*,*,#16657,.F.) ;
#22751 = ORIENTED_EDGE('',*,*,#16667,.T.) ;
#22752 = ORIENTED_EDGE('',*,*,#16669,.T.) ;
#22753 = ORIENTED_EDGE('',*,*,#16626,.T.) ;
#22754 = ORIENTED_EDGE('',*,*,#16578,.T.) ;
#22755 = ORIENTED_EDGE('',*,*,#16566,.T.) ;
#22756 = ORIENTED_EDGE('',*,*,#16670,.F.) ;
#22757 = ORIENTED_EDGE('',*,*,#16627,.T.) ;
#22758 = ORIENTED_EDGE('',*,*,#16669,.F.) ;
#22759 = ORIENTED_EDGE('',*,*,#16666,.T.) ;
#22760 = ORIENTED_EDGE('',*,*,#16671,.F.) ;
#22761 = ORIENTED_EDGE('',*,*,#16608,.T.) ;
#22762 = ORIENTED_EDGE('',*,*,#16672,.T.) ;
#22763 = ORIENTED_EDGE('',*,*,#16622,.T.) ;
#22764 = ORIENTED_EDGE('',*,*,#16672,.F.) ;
#22765 = ORIENTED_EDGE('',*,*,#16607,.T.) ;
#22766 = ORIENTED_EDGE('',*,*,#16659,.F.) ;
#22767 = ORIENTED_EDGE('',*,*,#16623,.T.) ;
#22768 = ORIENTED_EDGE('',*,*,#16673,.F.) ;
#22769 = ORIENTED_EDGE('',*,*,#16674,.T.) ;
#22770 = ORIENTED_EDGE('',*,*,#16582,.T.) ;
#22771 = ORIENTED_EDGE('',*,*,#16675,.T.) ;
#22772 = ORIENTED_EDGE('',*,*,#16676,.T.) ;
#22773 = ORIENTED_EDGE('',*,*,#16677,.T.) ;
#22774 = ORIENTED_EDGE('',*,*,#16594,.T.) ;
#22775 = ORIENTED_EDGE('',*,*,#16609,.T.) ;
#22776 = ORIENTED_EDGE('',*,*,#16671,.T.) ;
#22777 = ORIENTED_EDGE('',*,*,#16621,.T.) ;
#22778 = ORIENTED_EDGE('',*,*,#16580,.T.) ;
#22779 = ORIENTED_EDGE('',*,*,#16628,.T.) ;
#22780 = ORIENTED_EDGE('',*,*,#16670,.T.) ;
#22781 = ORIENTED_EDGE('',*,*,#16665,.T.) ;
#22782 = ORIENTED_EDGE('',*,*,#16598,.T.) ;
#22783 = ORIENTED_EDGE('',*,*,#16604,.T.) ;
#22784 = ORIENTED_EDGE('',*,*,#16655,.T.) ;
#22785 = ORIENTED_EDGE('',*,*,#16617,.T.) ;
#22786 = ORIENTED_EDGE('',*,*,#16590,.T.) ;
#22787 = ORIENTED_EDGE('',*,*,#16678,.T.) ;
#22788 = ORIENTED_EDGE('',*,*,#16679,.T.) ;
#22789 = ORIENTED_EDGE('',*,*,#16629,.T.) ;
#22790 = ORIENTED_EDGE('',*,*,#16587,.T.) ;
#22791 = ORIENTED_EDGE('',*,*,#16636,.T.) ;
#22792 = ORIENTED_EDGE('',*,*,#16680,.T.) ;
#22793 = ORIENTED_EDGE('',*,*,#16640,.T.) ;
#22794 = ORIENTED_EDGE('',*,*,#16583,.T.) ;
#22795 = ORIENTED_EDGE('',*,*,#16674,.F.) ;
#22796 = ORIENTED_EDGE('',*,*,#16595,.T.) ;
#22797 = ORIENTED_EDGE('',*,*,#16677,.F.) ;
#22798 = ORIENTED_EDGE('',*,*,#16681,.F.) ;
#22799 = ORIENTED_EDGE('',*,*,#16682,.F.) ;
#22800 = ORIENTED_EDGE('',*,*,#16541,.T.) ;
#22801 = ORIENTED_EDGE('',*,*,#16646,.F.) ;
#22802 = ORIENTED_EDGE('',*,*,#16661,.F.) ;
#22803 = ORIENTED_EDGE('',*,*,#16683,.F.) ;
#22804 = ORIENTED_EDGE('',*,*,#16684,.F.) ;
#22805 = ORIENTED_EDGE('',*,*,#16675,.F.) ;
#22806 = ORIENTED_EDGE('',*,*,#16581,.T.) ;
#22807 = ORIENTED_EDGE('',*,*,#16562,.T.) ;
#22808 = ORIENTED_EDGE('',*,*,#16596,.T.) ;
#22809 = ORIENTED_EDGE('',*,*,#16682,.T.) ;
#22810 = ORIENTED_EDGE('',*,*,#16685,.T.) ;
#22811 = ORIENTED_EDGE('',*,*,#16683,.T.) ;
#22812 = ORIENTED_EDGE('',*,*,#16660,.F.) ;
#22813 = ORIENTED_EDGE('',*,*,#16610,.T.) ;
#22814 = ORIENTED_EDGE('',*,*,#16538,.T.) ;
#22815 = ORIENTED_EDGE('',*,*,#16570,.T.) ;
#22816 = ORIENTED_EDGE('',*,*,#16676,.F.) ;
#22817 = ORIENTED_EDGE('',*,*,#16684,.T.) ;
#22818 = ORIENTED_EDGE('',*,*,#16685,.F.) ;
#22819 = ORIENTED_EDGE('',*,*,#16681,.T.) ;
#22820 = ORIENTED_EDGE('',*,*,#16545,.T.) ;
#22821 = ORIENTED_EDGE('',*,*,#16639,.T.) ;
#22822 = ORIENTED_EDGE('',*,*,#16662,.F.) ;
#22823 = ORIENTED_EDGE('',*,*,#16642,.T.) ;
#22824 = ORIENTED_EDGE('',*,*,#16686,.T.) ;
#22825 = ORIENTED_EDGE('',*,*,#16634,.T.) ;
#22826 = ORIENTED_EDGE('',*,*,#16585,.T.) ;
#22827 = ORIENTED_EDGE('',*,*,#16559,.T.) ;
#22828 = ORIENTED_EDGE('',*,*,#16680,.F.) ;
#22829 = ORIENTED_EDGE('',*,*,#16635,.T.) ;
#22830 = ORIENTED_EDGE('',*,*,#16686,.F.) ;
#22831 = ORIENTED_EDGE('',*,*,#16641,.T.) ;
#22832 = ORIENTED_EDGE('',*,*,#16550,.T.) ;
#22833 = ORIENTED_EDGE('',*,*,#16649,.F.) ;
#22834 = ORIENTED_EDGE('',*,*,#16664,.F.) ;
#22835 = ORIENTED_EDGE('',*,*,#16687,.F.) ;
#22836 = ORIENTED_EDGE('',*,*,#16688,.F.) ;
#22837 = ORIENTED_EDGE('',*,*,#16678,.F.) ;
#22838 = ORIENTED_EDGE('',*,*,#16589,.T.) ;
#22839 = ORIENTED_EDGE('',*,*,#16571,.T.) ;
#22840 = ORIENTED_EDGE('',*,*,#16663,.F.) ;
#22841 = ORIENTED_EDGE('',*,*,#16631,.T.) ;
#22842 = ORIENTED_EDGE('',*,*,#16689,.T.) ;
#22843 = ORIENTED_EDGE('',*,*,#16687,.T.) ;
#22844 = ORIENTED_EDGE('',*,*,#16679,.F.) ;
#22845 = ORIENTED_EDGE('',*,*,#16688,.T.) ;
#22846 = ORIENTED_EDGE('',*,*,#16689,.F.) ;
#22847 = ORIENTED_EDGE('',*,*,#16630,.T.) ;
#22848 = ORIENTED_EDGE('',*,*,#16690,.F.) ;
#22849 = ORIENTED_EDGE('',*,*,#16691,.T.) ;
#22850 = ORIENTED_EDGE('',*,*,#16692,.F.) ;
#22851 = ORIENTED_EDGE('',*,*,#16691,.F.) ;
#22852 = ORIENTED_EDGE('',*,*,#16690,.T.) ;
#22853 = ORIENTED_EDGE('',*,*,#16693,.T.) ;
#22854 = ORIENTED_EDGE('',*,*,#16673,.T.) ;
#22855 = ORIENTED_EDGE('',*,*,#16694,.F.) ;
#22856 = ORIENTED_EDGE('',*,*,#16695,.T.) ;
#22857 = ORIENTED_EDGE('',*,*,#16693,.F.) ;
#22858 = ORIENTED_EDGE('',*,*,#16695,.F.) ;
#22859 = ORIENTED_EDGE('',*,*,#16694,.T.) ;
#22860 = ORIENTED_EDGE('',*,*,#16692,.T.) ;
#22861 = ORIENTED_EDGE('',*,*,#16696,.F.) ;
#22862 = ORIENTED_EDGE('',*,*,#16697,.T.) ;
#22863 = ORIENTED_EDGE('',*,*,#16698,.F.) ;
#22864 = ORIENTED_EDGE('',*,*,#16697,.F.) ;
#22865 = ORIENTED_EDGE('',*,*,#16699,.F.) ;
#22866 = ORIENTED_EDGE('',*,*,#16700,.T.) ;
#22867 = ORIENTED_EDGE('',*,*,#16701,.F.) ;
#22868 = ORIENTED_EDGE('',*,*,#16700,.F.) ;
#22869 = ORIENTED_EDGE('',*,*,#16701,.T.) ;
#22870 = ORIENTED_EDGE('',*,*,#16696,.T.) ;
#22871 = ORIENTED_EDGE('',*,*,#16699,.T.) ;
#22872 = ORIENTED_EDGE('',*,*,#16698,.T.) ;
#22873 = ORIENTED_EDGE('',*,*,#16702,.F.) ;
#22874 = ORIENTED_EDGE('',*,*,#16703,.T.) ;
#22875 = ORIENTED_EDGE('',*,*,#16704,.F.) ;
#22876 = ORIENTED_EDGE('',*,*,#16705,.F.) ;
#22877 = ORIENTED_EDGE('',*,*,#16706,.F.) ;
#22878 = ORIENTED_EDGE('',*,*,#16705,.T.) ;
#22879 = ORIENTED_EDGE('',*,*,#16707,.T.) ;
#22880 = ORIENTED_EDGE('',*,*,#16708,.F.) ;
#22881 = ORIENTED_EDGE('',*,*,#16709,.T.) ;
#22882 = ORIENTED_EDGE('',*,*,#16710,.F.) ;
#22883 = ORIENTED_EDGE('',*,*,#16711,.F.) ;
#22884 = ORIENTED_EDGE('',*,*,#16709,.F.) ;
#22885 = ORIENTED_EDGE('',*,*,#16712,.F.) ;
#22886 = ORIENTED_EDGE('',*,*,#16713,.F.) ;
#22887 = ORIENTED_EDGE('',*,*,#16714,.F.) ;
#22888 = ORIENTED_EDGE('',*,*,#16715,.F.) ;
#22889 = ORIENTED_EDGE('',*,*,#16713,.T.) ;
#22890 = ORIENTED_EDGE('',*,*,#16716,.F.) ;
#22891 = ORIENTED_EDGE('',*,*,#16717,.T.) ;
#22892 = ORIENTED_EDGE('',*,*,#16703,.F.) ;
#22893 = ORIENTED_EDGE('',*,*,#16714,.T.) ;
#22894 = ORIENTED_EDGE('',*,*,#16702,.T.) ;
#22895 = ORIENTED_EDGE('',*,*,#16706,.T.) ;
#22896 = ORIENTED_EDGE('',*,*,#16718,.T.) ;
#22897 = ORIENTED_EDGE('',*,*,#16719,.T.) ;
#22898 = ORIENTED_EDGE('',*,*,#16720,.F.) ;
#22899 = ORIENTED_EDGE('',*,*,#16721,.T.) ;
#22900 = ORIENTED_EDGE('',*,*,#16722,.T.) ;
#22901 = ORIENTED_EDGE('',*,*,#16704,.T.) ;
#22902 = ORIENTED_EDGE('',*,*,#16723,.T.) ;
#22903 = ORIENTED_EDGE('',*,*,#16724,.F.) ;
#22904 = ORIENTED_EDGE('',*,*,#16725,.T.) ;
#22905 = ORIENTED_EDGE('',*,*,#16717,.F.) ;
#22906 = ORIENTED_EDGE('',*,*,#16726,.F.) ;
#22907 = ORIENTED_EDGE('',*,*,#16727,.F.) ;
#22908 = ORIENTED_EDGE('',*,*,#16721,.F.) ;
#22909 = ORIENTED_EDGE('',*,*,#16728,.F.) ;
#22910 = ORIENTED_EDGE('',*,*,#16723,.F.) ;
#22911 = ORIENTED_EDGE('',*,*,#16716,.T.) ;
#22912 = ORIENTED_EDGE('',*,*,#16712,.T.) ;
#22913 = ORIENTED_EDGE('',*,*,#16708,.T.) ;
#22914 = ORIENTED_EDGE('',*,*,#16729,.T.) ;
#22915 = ORIENTED_EDGE('',*,*,#16730,.F.) ;
#22916 = ORIENTED_EDGE('',*,*,#16731,.F.) ;
#22917 = ORIENTED_EDGE('',*,*,#16732,.T.) ;
#22918 = ORIENTED_EDGE('',*,*,#16726,.T.) ;
#22919 = ORIENTED_EDGE('',*,*,#16715,.T.) ;
#22920 = ORIENTED_EDGE('',*,*,#16722,.F.) ;
#22921 = ORIENTED_EDGE('',*,*,#16733,.F.) ;
#22922 = ORIENTED_EDGE('',*,*,#16734,.F.) ;
#22923 = ORIENTED_EDGE('',*,*,#16735,.T.) ;
#22924 = ORIENTED_EDGE('',*,*,#16718,.F.) ;
#22925 = ORIENTED_EDGE('',*,*,#16710,.T.) ;
#22926 = ORIENTED_EDGE('',*,*,#16711,.T.) ;
#22927 = ORIENTED_EDGE('',*,*,#16731,.T.) ;
#22928 = ORIENTED_EDGE('',*,*,#16736,.T.) ;
#22929 = ORIENTED_EDGE('',*,*,#16734,.T.) ;
#22930 = ORIENTED_EDGE('',*,*,#16737,.T.) ;
#22931 = ORIENTED_EDGE('',*,*,#16733,.T.) ;
#22932 = ORIENTED_EDGE('',*,*,#16727,.T.) ;
#22933 = ORIENTED_EDGE('',*,*,#16732,.F.) ;
#22934 = ORIENTED_EDGE('',*,*,#16737,.F.) ;
#22935 = ORIENTED_EDGE('',*,*,#16730,.T.) ;
#22936 = ORIENTED_EDGE('',*,*,#16738,.T.) ;
#22937 = ORIENTED_EDGE('',*,*,#16735,.F.) ;
#22938 = ORIENTED_EDGE('',*,*,#16736,.F.) ;
#22939 = ORIENTED_EDGE('',*,*,#16707,.F.) ;
#22940 = ORIENTED_EDGE('',*,*,#16725,.F.) ;
#22941 = ORIENTED_EDGE('',*,*,#16739,.F.) ;
#22942 = ORIENTED_EDGE('',*,*,#16719,.F.) ;
#22943 = ORIENTED_EDGE('',*,*,#16738,.F.) ;
#22944 = ORIENTED_EDGE('',*,*,#16729,.F.) ;
#22945 = ORIENTED_EDGE('',*,*,#16739,.T.) ;
#22946 = ORIENTED_EDGE('',*,*,#16724,.T.) ;
#22947 = ORIENTED_EDGE('',*,*,#16728,.T.) ;
#22948 = ORIENTED_EDGE('',*,*,#16720,.T.) ;
#22949 = ORIENTED_EDGE('',*,*,#16740,.F.) ;
#22950 = ORIENTED_EDGE('',*,*,#16741,.T.) ;
#22951 = ORIENTED_EDGE('',*,*,#16742,.F.) ;
#22952 = ORIENTED_EDGE('',*,*,#16741,.F.) ;
#22953 = ORIENTED_EDGE('',*,*,#16742,.T.) ;
#22954 = ORIENTED_EDGE('',*,*,#16740,.T.) ;
#22955 = ORIENTED_EDGE('',*,*,#16743,.F.) ;
#22956 = ORIENTED_EDGE('',*,*,#16744,.T.) ;
#22957 = ORIENTED_EDGE('',*,*,#16745,.F.) ;
#22958 = ORIENTED_EDGE('',*,*,#16744,.F.) ;
#22959 = ORIENTED_EDGE('',*,*,#16745,.T.) ;
#22960 = ORIENTED_EDGE('',*,*,#16746,.F.) ;
#22961 = ORIENTED_EDGE('',*,*,#16747,.T.) ;
#22962 = ORIENTED_EDGE('',*,*,#16748,.F.) ;
#22963 = ORIENTED_EDGE('',*,*,#16747,.F.) ;
#22964 = ORIENTED_EDGE('',*,*,#16749,.F.) ;
#22965 = ORIENTED_EDGE('',*,*,#16750,.T.) ;
#22966 = ORIENTED_EDGE('',*,*,#16751,.F.) ;
#22967 = ORIENTED_EDGE('',*,*,#16750,.F.) ;
#22968 = ORIENTED_EDGE('',*,*,#16751,.T.) ;
#22969 = ORIENTED_EDGE('',*,*,#16743,.T.) ;
#22970 = ORIENTED_EDGE('',*,*,#16746,.T.) ;
#22971 = ORIENTED_EDGE('',*,*,#16749,.T.) ;
#22972 = ORIENTED_EDGE('',*,*,#16748,.T.) ;
#22973 = ORIENTED_EDGE('',*,*,#16752,.F.) ;
#22974 = ORIENTED_EDGE('',*,*,#16753,.T.) ;
#22975 = ORIENTED_EDGE('',*,*,#16754,.F.) ;
#22976 = ORIENTED_EDGE('',*,*,#16753,.F.) ;
#22977 = ORIENTED_EDGE('',*,*,#16755,.F.) ;
#22978 = ORIENTED_EDGE('',*,*,#16756,.T.) ;
#22979 = ORIENTED_EDGE('',*,*,#16757,.F.) ;
#22980 = ORIENTED_EDGE('',*,*,#16756,.F.) ;
#22981 = ORIENTED_EDGE('',*,*,#16757,.T.) ;
#22982 = ORIENTED_EDGE('',*,*,#16752,.T.) ;
#22983 = ORIENTED_EDGE('',*,*,#16755,.T.) ;
#22984 = ORIENTED_EDGE('',*,*,#16754,.T.) ;
#22985 = ORIENTED_EDGE('',*,*,#16758,.F.) ;
#22986 = ORIENTED_EDGE('',*,*,#16759,.T.) ;
#22987 = ORIENTED_EDGE('',*,*,#16760,.F.) ;
#22988 = ORIENTED_EDGE('',*,*,#16759,.F.) ;
#22989 = ORIENTED_EDGE('',*,*,#16761,.F.) ;
#22990 = ORIENTED_EDGE('',*,*,#16762,.T.) ;
#22991 = ORIENTED_EDGE('',*,*,#16763,.F.) ;
#22992 = ORIENTED_EDGE('',*,*,#16762,.F.) ;
#22993 = ORIENTED_EDGE('',*,*,#16763,.T.) ;
#22994 = ORIENTED_EDGE('',*,*,#16758,.T.) ;
#22995 = ORIENTED_EDGE('',*,*,#16761,.T.) ;
#22996 = ORIENTED_EDGE('',*,*,#16760,.T.) ;
#22997 = ORIENTED_EDGE('',*,*,#16764,.F.) ;
#22998 = ORIENTED_EDGE('',*,*,#16765,.T.) ;
#22999 = ORIENTED_EDGE('',*,*,#16766,.F.) ;
#23000 = ORIENTED_EDGE('',*,*,#16765,.F.) ;
#23001 = ORIENTED_EDGE('',*,*,#16766,.T.) ;
#23002 = ORIENTED_EDGE('',*,*,#16764,.T.) ;
#23003 = ORIENTED_EDGE('',*,*,#16767,.T.) ;
#23004 = ORIENTED_EDGE('',*,*,#16768,.F.) ;
#23005 = ORIENTED_EDGE('',*,*,#16769,.T.) ;
#23006 = ORIENTED_EDGE('',*,*,#16770,.F.) ;
#23007 = ORIENTED_EDGE('',*,*,#16769,.F.) ;
#23008 = ORIENTED_EDGE('',*,*,#16771,.T.) ;
#23009 = ORIENTED_EDGE('',*,*,#16767,.F.) ;
#23010 = ORIENTED_EDGE('',*,*,#16771,.F.) ;
#23011 = ORIENTED_EDGE('',*,*,#16772,.F.) ;
#23012 = ORIENTED_EDGE('',*,*,#16773,.T.) ;
#23013 = ORIENTED_EDGE('',*,*,#16774,.T.) ;
#23014 = ORIENTED_EDGE('',*,*,#16775,.T.) ;
#23015 = ORIENTED_EDGE('',*,*,#16776,.T.) ;
#23016 = ORIENTED_EDGE('',*,*,#16777,.T.) ;
#23017 = ORIENTED_EDGE('',*,*,#16778,.T.) ;
#23018 = ORIENTED_EDGE('',*,*,#16779,.T.) ;
#23019 = ORIENTED_EDGE('',*,*,#16780,.T.) ;
#23020 = ORIENTED_EDGE('',*,*,#16781,.T.) ;
#23021 = ORIENTED_EDGE('',*,*,#16770,.T.) ;
#23022 = ORIENTED_EDGE('',*,*,#16781,.F.) ;
#23023 = ORIENTED_EDGE('',*,*,#16782,.T.) ;
#23024 = ORIENTED_EDGE('',*,*,#16783,.T.) ;
#23025 = ORIENTED_EDGE('',*,*,#16784,.T.) ;
#23026 = ORIENTED_EDGE('',*,*,#16777,.F.) ;
#23027 = ORIENTED_EDGE('',*,*,#16785,.T.) ;
#23028 = ORIENTED_EDGE('',*,*,#16786,.T.) ;
#23029 = ORIENTED_EDGE('',*,*,#16787,.T.) ;
#23030 = ORIENTED_EDGE('',*,*,#16773,.F.) ;
#23031 = ORIENTED_EDGE('',*,*,#16788,.T.) ;
#23032 = ORIENTED_EDGE('',*,*,#16789,.T.) ;
#23033 = ORIENTED_EDGE('',*,*,#16790,.T.) ;
#23034 = ORIENTED_EDGE('',*,*,#16791,.T.) ;
#23035 = ORIENTED_EDGE('',*,*,#16792,.T.) ;
#23036 = ORIENTED_EDGE('',*,*,#16793,.T.) ;
#23037 = ORIENTED_EDGE('',*,*,#16794,.T.) ;
#23038 = ORIENTED_EDGE('',*,*,#16795,.T.) ;
#23039 = ORIENTED_EDGE('',*,*,#16796,.T.) ;
#23040 = ORIENTED_EDGE('',*,*,#16797,.T.) ;
#23041 = ORIENTED_EDGE('',*,*,#16798,.T.) ;
#23042 = ORIENTED_EDGE('',*,*,#16799,.T.) ;
#23043 = ORIENTED_EDGE('',*,*,#16800,.T.) ;
#23044 = ORIENTED_EDGE('',*,*,#16801,.T.) ;
#23045 = ORIENTED_EDGE('',*,*,#16802,.T.) ;
#23046 = ORIENTED_EDGE('',*,*,#16803,.T.) ;
#23047 = ORIENTED_EDGE('',*,*,#16804,.T.) ;
#23048 = ORIENTED_EDGE('',*,*,#16805,.T.) ;
#23049 = ORIENTED_EDGE('',*,*,#16806,.T.) ;
#23050 = ORIENTED_EDGE('',*,*,#16807,.T.) ;
#23051 = ORIENTED_EDGE('',*,*,#16808,.T.) ;
#23052 = ORIENTED_EDGE('',*,*,#16809,.T.) ;
#23053 = ORIENTED_EDGE('',*,*,#16810,.T.) ;
#23054 = ORIENTED_EDGE('',*,*,#16811,.T.) ;
#23055 = ORIENTED_EDGE('',*,*,#16806,.F.) ;
#23056 = ORIENTED_EDGE('',*,*,#16812,.T.) ;
#23057 = ORIENTED_EDGE('',*,*,#16813,.T.) ;
#23058 = ORIENTED_EDGE('',*,*,#16814,.T.) ;
#23059 = ORIENTED_EDGE('',*,*,#16805,.F.) ;
#23060 = ORIENTED_EDGE('',*,*,#16815,.F.) ;
#23061 = ORIENTED_EDGE('',*,*,#16816,.F.) ;
#23062 = ORIENTED_EDGE('',*,*,#16812,.F.) ;
#23063 = ORIENTED_EDGE('',*,*,#16807,.F.) ;
#23064 = ORIENTED_EDGE('',*,*,#16814,.F.) ;
#23065 = ORIENTED_EDGE('',*,*,#16817,.T.) ;
#23066 = ORIENTED_EDGE('',*,*,#16818,.F.) ;
#23067 = ORIENTED_EDGE('',*,*,#16809,.F.) ;
#23068 = ORIENTED_EDGE('',*,*,#16819,.F.) ;
#23069 = ORIENTED_EDGE('',*,*,#16820,.F.) ;
#23070 = ORIENTED_EDGE('',*,*,#16821,.F.) ;
#23071 = ORIENTED_EDGE('',*,*,#16804,.F.) ;
#23072 = ORIENTED_EDGE('',*,*,#16818,.T.) ;
#23073 = ORIENTED_EDGE('',*,*,#16822,.T.) ;
#23074 = ORIENTED_EDGE('',*,*,#16815,.T.) ;
#23075 = ORIENTED_EDGE('',*,*,#16808,.F.) ;
#23076 = ORIENTED_EDGE('',*,*,#16823,.T.) ;
#23077 = ORIENTED_EDGE('',*,*,#16824,.T.) ;
#23078 = ORIENTED_EDGE('',*,*,#16819,.T.) ;
#23079 = ORIENTED_EDGE('',*,*,#16810,.F.) ;
#23080 = ORIENTED_EDGE('',*,*,#16821,.T.) ;
#23081 = ORIENTED_EDGE('',*,*,#16825,.T.) ;
#23082 = ORIENTED_EDGE('',*,*,#16826,.T.) ;
#23083 = ORIENTED_EDGE('',*,*,#16816,.T.) ;
#23084 = ORIENTED_EDGE('',*,*,#16822,.F.) ;
#23085 = ORIENTED_EDGE('',*,*,#16817,.F.) ;
#23086 = ORIENTED_EDGE('',*,*,#16813,.F.) ;
#23087 = ORIENTED_EDGE('',*,*,#16811,.F.) ;
#23088 = ORIENTED_EDGE('',*,*,#16826,.F.) ;
#23089 = ORIENTED_EDGE('',*,*,#16827,.T.) ;
#23090 = ORIENTED_EDGE('',*,*,#16823,.F.) ;
#23091 = ORIENTED_EDGE('',*,*,#16820,.T.) ;
#23092 = ORIENTED_EDGE('',*,*,#16824,.F.) ;
#23093 = ORIENTED_EDGE('',*,*,#16827,.F.) ;
#23094 = ORIENTED_EDGE('',*,*,#16825,.F.) ;
#23095 = ORIENTED_EDGE('',*,*,#16802,.F.) ;
#23096 = ORIENTED_EDGE('',*,*,#16828,.T.) ;
#23097 = ORIENTED_EDGE('',*,*,#16829,.T.) ;
#23098 = ORIENTED_EDGE('',*,*,#16830,.T.) ;
#23099 = ORIENTED_EDGE('',*,*,#16801,.F.) ;
#23100 = ORIENTED_EDGE('',*,*,#16831,.F.) ;
#23101 = ORIENTED_EDGE('',*,*,#16832,.F.) ;
#23102 = ORIENTED_EDGE('',*,*,#16828,.F.) ;
#23103 = ORIENTED_EDGE('',*,*,#16803,.F.) ;
#23104 = ORIENTED_EDGE('',*,*,#16830,.F.) ;
#23105 = ORIENTED_EDGE('',*,*,#16833,.T.) ;
#23106 = ORIENTED_EDGE('',*,*,#16834,.F.) ;
#23107 = ORIENTED_EDGE('',*,*,#16787,.F.) ;
#23108 = ORIENTED_EDGE('',*,*,#16835,.F.) ;
#23109 = ORIENTED_EDGE('',*,*,#16836,.F.) ;
#23110 = ORIENTED_EDGE('',*,*,#16837,.F.) ;
#23111 = ORIENTED_EDGE('',*,*,#16774,.F.) ;
#23112 = ORIENTED_EDGE('',*,*,#16800,.F.) ;
#23113 = ORIENTED_EDGE('',*,*,#16834,.T.) ;
#23114 = ORIENTED_EDGE('',*,*,#16838,.T.) ;
#23115 = ORIENTED_EDGE('',*,*,#16831,.T.) ;
#23116 = ORIENTED_EDGE('',*,*,#16786,.F.) ;
#23117 = ORIENTED_EDGE('',*,*,#16839,.T.) ;
#23118 = ORIENTED_EDGE('',*,*,#16840,.T.) ;
#23119 = ORIENTED_EDGE('',*,*,#16835,.T.) ;
#23120 = ORIENTED_EDGE('',*,*,#16775,.F.) ;
#23121 = ORIENTED_EDGE('',*,*,#16837,.T.) ;
#23122 = ORIENTED_EDGE('',*,*,#16841,.T.) ;
#23123 = ORIENTED_EDGE('',*,*,#16842,.T.) ;
#23124 = ORIENTED_EDGE('',*,*,#16776,.F.) ;
#23125 = ORIENTED_EDGE('',*,*,#16842,.F.) ;
#23126 = ORIENTED_EDGE('',*,*,#16843,.T.) ;
#23127 = ORIENTED_EDGE('',*,*,#16839,.F.) ;
#23128 = ORIENTED_EDGE('',*,*,#16785,.F.) ;
#23129 = ORIENTED_EDGE('',*,*,#16836,.T.) ;
#23130 = ORIENTED_EDGE('',*,*,#16840,.F.) ;
#23131 = ORIENTED_EDGE('',*,*,#16843,.F.) ;
#23132 = ORIENTED_EDGE('',*,*,#16841,.F.) ;
#23133 = ORIENTED_EDGE('',*,*,#16832,.T.) ;
#23134 = ORIENTED_EDGE('',*,*,#16838,.F.) ;
#23135 = ORIENTED_EDGE('',*,*,#16833,.F.) ;
#23136 = ORIENTED_EDGE('',*,*,#16829,.F.) ;
#23137 = ORIENTED_EDGE('',*,*,#16794,.F.) ;
#23138 = ORIENTED_EDGE('',*,*,#16844,.T.) ;
#23139 = ORIENTED_EDGE('',*,*,#16845,.T.) ;
#23140 = ORIENTED_EDGE('',*,*,#16846,.T.) ;
#23141 = ORIENTED_EDGE('',*,*,#16793,.F.) ;
#23142 = ORIENTED_EDGE('',*,*,#16847,.F.) ;
#23143 = ORIENTED_EDGE('',*,*,#16848,.F.) ;
#23144 = ORIENTED_EDGE('',*,*,#16844,.F.) ;
#23145 = ORIENTED_EDGE('',*,*,#16795,.F.) ;
#23146 = ORIENTED_EDGE('',*,*,#16846,.F.) ;
#23147 = ORIENTED_EDGE('',*,*,#16849,.T.) ;
#23148 = ORIENTED_EDGE('',*,*,#16850,.F.) ;
#23149 = ORIENTED_EDGE('',*,*,#16797,.F.) ;
#23150 = ORIENTED_EDGE('',*,*,#16851,.F.) ;
#23151 = ORIENTED_EDGE('',*,*,#16852,.F.) ;
#23152 = ORIENTED_EDGE('',*,*,#16853,.F.) ;
#23153 = ORIENTED_EDGE('',*,*,#16792,.F.) ;
#23154 = ORIENTED_EDGE('',*,*,#16850,.T.) ;
#23155 = ORIENTED_EDGE('',*,*,#16854,.T.) ;
#23156 = ORIENTED_EDGE('',*,*,#16847,.T.) ;
#23157 = ORIENTED_EDGE('',*,*,#16796,.F.) ;
#23158 = ORIENTED_EDGE('',*,*,#16855,.T.) ;
#23159 = ORIENTED_EDGE('',*,*,#16856,.T.) ;
#23160 = ORIENTED_EDGE('',*,*,#16851,.T.) ;
#23161 = ORIENTED_EDGE('',*,*,#16798,.F.) ;
#23162 = ORIENTED_EDGE('',*,*,#16853,.T.) ;
#23163 = ORIENTED_EDGE('',*,*,#16857,.T.) ;
#23164 = ORIENTED_EDGE('',*,*,#16858,.T.) ;
#23165 = ORIENTED_EDGE('',*,*,#16848,.T.) ;
#23166 = ORIENTED_EDGE('',*,*,#16854,.F.) ;
#23167 = ORIENTED_EDGE('',*,*,#16849,.F.) ;
#23168 = ORIENTED_EDGE('',*,*,#16845,.F.) ;
#23169 = ORIENTED_EDGE('',*,*,#16799,.F.) ;
#23170 = ORIENTED_EDGE('',*,*,#16858,.F.) ;
#23171 = ORIENTED_EDGE('',*,*,#16859,.T.) ;
#23172 = ORIENTED_EDGE('',*,*,#16855,.F.) ;
#23173 = ORIENTED_EDGE('',*,*,#16852,.T.) ;
#23174 = ORIENTED_EDGE('',*,*,#16856,.F.) ;
#23175 = ORIENTED_EDGE('',*,*,#16859,.F.) ;
#23176 = ORIENTED_EDGE('',*,*,#16857,.F.) ;
#23177 = ORIENTED_EDGE('',*,*,#16790,.F.) ;
#23178 = ORIENTED_EDGE('',*,*,#16860,.T.) ;
#23179 = ORIENTED_EDGE('',*,*,#16861,.T.) ;
#23180 = ORIENTED_EDGE('',*,*,#16862,.T.) ;
#23181 = ORIENTED_EDGE('',*,*,#16789,.F.) ;
#23182 = ORIENTED_EDGE('',*,*,#16863,.F.) ;
#23183 = ORIENTED_EDGE('',*,*,#16864,.F.) ;
#23184 = ORIENTED_EDGE('',*,*,#16860,.F.) ;
#23185 = ORIENTED_EDGE('',*,*,#16791,.F.) ;
#23186 = ORIENTED_EDGE('',*,*,#16862,.F.) ;
#23187 = ORIENTED_EDGE('',*,*,#16865,.T.) ;
#23188 = ORIENTED_EDGE('',*,*,#16866,.F.) ;
#23189 = ORIENTED_EDGE('',*,*,#16784,.F.) ;
#23190 = ORIENTED_EDGE('',*,*,#16867,.F.) ;
#23191 = ORIENTED_EDGE('',*,*,#16868,.F.) ;
#23192 = ORIENTED_EDGE('',*,*,#16869,.F.) ;
#23193 = ORIENTED_EDGE('',*,*,#16778,.F.) ;
#23194 = ORIENTED_EDGE('',*,*,#16788,.F.) ;
#23195 = ORIENTED_EDGE('',*,*,#16866,.T.) ;
#23196 = ORIENTED_EDGE('',*,*,#16870,.T.) ;
#23197 = ORIENTED_EDGE('',*,*,#16863,.T.) ;
#23198 = ORIENTED_EDGE('',*,*,#16783,.F.) ;
#23199 = ORIENTED_EDGE('',*,*,#16871,.T.) ;
#23200 = ORIENTED_EDGE('',*,*,#16872,.T.) ;
#23201 = ORIENTED_EDGE('',*,*,#16867,.T.) ;
#23202 = ORIENTED_EDGE('',*,*,#16779,.F.) ;
#23203 = ORIENTED_EDGE('',*,*,#16869,.T.) ;
#23204 = ORIENTED_EDGE('',*,*,#16873,.T.) ;
#23205 = ORIENTED_EDGE('',*,*,#16874,.T.) ;
#23206 = ORIENTED_EDGE('',*,*,#16780,.F.) ;
#23207 = ORIENTED_EDGE('',*,*,#16874,.F.) ;
#23208 = ORIENTED_EDGE('',*,*,#16875,.T.) ;
#23209 = ORIENTED_EDGE('',*,*,#16871,.F.) ;
#23210 = ORIENTED_EDGE('',*,*,#16782,.F.) ;
#23211 = ORIENTED_EDGE('',*,*,#16868,.T.) ;
#23212 = ORIENTED_EDGE('',*,*,#16872,.F.) ;
#23213 = ORIENTED_EDGE('',*,*,#16875,.F.) ;
#23214 = ORIENTED_EDGE('',*,*,#16873,.F.) ;
#23215 = ORIENTED_EDGE('',*,*,#16864,.T.) ;
#23216 = ORIENTED_EDGE('',*,*,#16870,.F.) ;
#23217 = ORIENTED_EDGE('',*,*,#16865,.F.) ;
#23218 = ORIENTED_EDGE('',*,*,#16861,.F.) ;
#23219 = ORIENTED_EDGE('',*,*,#16768,.T.) ;
#23220 = ORIENTED_EDGE('',*,*,#16876,.T.) ;
#23221 = ORIENTED_EDGE('',*,*,#16877,.F.) ;
#23222 = ORIENTED_EDGE('',*,*,#16876,.F.) ;
#23223 = ORIENTED_EDGE('',*,*,#16877,.T.) ;
#23224 = ORIENTED_EDGE('',*,*,#16772,.T.) ;
#23225 = ORIENTED_EDGE('',*,*,#16878,.F.) ;
#23226 = ORIENTED_EDGE('',*,*,#16879,.T.) ;
#23227 = ORIENTED_EDGE('',*,*,#16880,.F.) ;
#23228 = ORIENTED_EDGE('',*,*,#16879,.F.) ;
#23229 = ORIENTED_EDGE('',*,*,#16881,.F.) ;
#23230 = ORIENTED_EDGE('',*,*,#16882,.T.) ;
#23231 = ORIENTED_EDGE('',*,*,#16883,.F.) ;
#23232 = ORIENTED_EDGE('',*,*,#16882,.F.) ;
#23233 = ORIENTED_EDGE('',*,*,#16883,.T.) ;
#23234 = ORIENTED_EDGE('',*,*,#16878,.T.) ;
#23235 = ORIENTED_EDGE('',*,*,#16881,.T.) ;
#23236 = ORIENTED_EDGE('',*,*,#16880,.T.) ;
#23237 = ORIENTED_EDGE('',*,*,#16884,.F.) ;
#23238 = ORIENTED_EDGE('',*,*,#16885,.T.) ;
#23239 = ORIENTED_EDGE('',*,*,#16886,.F.) ;
#23240 = ORIENTED_EDGE('',*,*,#16885,.F.) ;
#23241 = ORIENTED_EDGE('',*,*,#16887,.F.) ;
#23242 = ORIENTED_EDGE('',*,*,#16888,.T.) ;
#23243 = ORIENTED_EDGE('',*,*,#16889,.T.) ;
#23244 = ORIENTED_EDGE('',*,*,#16890,.T.) ;
#23245 = ORIENTED_EDGE('',*,*,#16884,.T.) ;
#23246 = ORIENTED_EDGE('',*,*,#16891,.T.) ;
#23247 = ORIENTED_EDGE('',*,*,#16889,.F.) ;
#23248 = ORIENTED_EDGE('',*,*,#16892,.F.) ;
#23249 = ORIENTED_EDGE('',*,*,#16893,.F.) ;
#23250 = ORIENTED_EDGE('',*,*,#16894,.T.) ;
#23251 = ORIENTED_EDGE('',*,*,#16895,.F.) ;
#23252 = ORIENTED_EDGE('',*,*,#16896,.F.) ;
#23253 = ORIENTED_EDGE('',*,*,#16890,.F.) ;
#23254 = ORIENTED_EDGE('',*,*,#16891,.F.) ;
#23255 = ORIENTED_EDGE('',*,*,#16897,.F.) ;
#23256 = ORIENTED_EDGE('',*,*,#16898,.T.) ;
#23257 = ORIENTED_EDGE('',*,*,#16899,.F.) ;
#23258 = ORIENTED_EDGE('',*,*,#16894,.F.) ;
#23259 = ORIENTED_EDGE('',*,*,#16900,.F.) ;
#23260 = ORIENTED_EDGE('',*,*,#16900,.T.) ;
#23261 = ORIENTED_EDGE('',*,*,#16897,.T.) ;
#23262 = ORIENTED_EDGE('',*,*,#16893,.T.) ;
#23263 = ORIENTED_EDGE('',*,*,#16901,.T.) ;
#23264 = ORIENTED_EDGE('',*,*,#16886,.T.) ;
#23265 = ORIENTED_EDGE('',*,*,#16902,.T.) ;
#23266 = ORIENTED_EDGE('',*,*,#16903,.F.) ;
#23267 = ORIENTED_EDGE('',*,*,#16898,.F.) ;
#23268 = ORIENTED_EDGE('',*,*,#16901,.F.) ;
#23269 = ORIENTED_EDGE('',*,*,#16892,.T.) ;
#23270 = ORIENTED_EDGE('',*,*,#16888,.F.) ;
#23271 = ORIENTED_EDGE('',*,*,#16887,.T.) ;
#23272 = ORIENTED_EDGE('',*,*,#16896,.T.) ;
#23273 = ORIENTED_EDGE('',*,*,#16904,.F.) ;
#23274 = ORIENTED_EDGE('',*,*,#16902,.F.) ;
#23275 = ORIENTED_EDGE('',*,*,#16905,.F.) ;
#23276 = ORIENTED_EDGE('',*,*,#16906,.T.) ;
#23277 = ORIENTED_EDGE('',*,*,#16907,.F.) ;
#23278 = ORIENTED_EDGE('',*,*,#16906,.F.) ;
#23279 = ORIENTED_EDGE('',*,*,#16908,.T.) ;
#23280 = ORIENTED_EDGE('',*,*,#16909,.T.) ;
#23281 = ORIENTED_EDGE('',*,*,#16910,.T.) ;
#23282 = ORIENTED_EDGE('',*,*,#16911,.T.) ;
#23283 = ORIENTED_EDGE('',*,*,#16912,.T.) ;
#23284 = ORIENTED_EDGE('',*,*,#16913,.F.) ;
#23285 = ORIENTED_EDGE('',*,*,#16914,.F.) ;
#23286 = ORIENTED_EDGE('',*,*,#16911,.F.) ;
#23287 = ORIENTED_EDGE('',*,*,#16915,.T.) ;
#23288 = ORIENTED_EDGE('',*,*,#16916,.F.) ;
#23289 = ORIENTED_EDGE('',*,*,#16912,.F.) ;
#23290 = ORIENTED_EDGE('',*,*,#16910,.F.) ;
#23291 = ORIENTED_EDGE('',*,*,#16905,.T.) ;
#23292 = ORIENTED_EDGE('',*,*,#16917,.T.) ;
#23293 = ORIENTED_EDGE('',*,*,#16918,.F.) ;
#23294 = ORIENTED_EDGE('',*,*,#16915,.F.) ;
#23295 = ORIENTED_EDGE('',*,*,#16909,.F.) ;
#23296 = ORIENTED_EDGE('',*,*,#16914,.T.) ;
#23297 = ORIENTED_EDGE('',*,*,#16919,.F.) ;
#23298 = ORIENTED_EDGE('',*,*,#16917,.F.) ;
#23299 = ORIENTED_EDGE('',*,*,#16908,.F.) ;
#23300 = ORIENTED_EDGE('',*,*,#16907,.T.) ;
#23301 = ORIENTED_EDGE('',*,*,#16920,.F.) ;
#23302 = ORIENTED_EDGE('',*,*,#16921,.T.) ;
#23303 = ORIENTED_EDGE('',*,*,#16922,.F.) ;
#23304 = ORIENTED_EDGE('',*,*,#16921,.F.) ;
#23305 = ORIENTED_EDGE('',*,*,#16923,.F.) ;
#23306 = ORIENTED_EDGE('',*,*,#16924,.T.) ;
#23307 = ORIENTED_EDGE('',*,*,#16925,.F.) ;
#23308 = ORIENTED_EDGE('',*,*,#16924,.F.) ;
#23309 = ORIENTED_EDGE('',*,*,#16926,.F.) ;
#23310 = ORIENTED_EDGE('',*,*,#16927,.T.) ;
#23311 = ORIENTED_EDGE('',*,*,#16928,.F.) ;
#23312 = ORIENTED_EDGE('',*,*,#16927,.F.) ;
#23313 = ORIENTED_EDGE('',*,*,#16929,.F.) ;
#23314 = ORIENTED_EDGE('',*,*,#16930,.T.) ;
#23315 = ORIENTED_EDGE('',*,*,#16931,.F.) ;
#23316 = ORIENTED_EDGE('',*,*,#16930,.F.) ;
#23317 = ORIENTED_EDGE('',*,*,#16932,.F.) ;
#23318 = ORIENTED_EDGE('',*,*,#16933,.T.) ;
#23319 = ORIENTED_EDGE('',*,*,#16934,.F.) ;
#23320 = ORIENTED_EDGE('',*,*,#16935,.F.) ;
#23321 = ORIENTED_EDGE('',*,*,#16936,.F.) ;
#23322 = ORIENTED_EDGE('',*,*,#16937,.F.) ;
#23323 = ORIENTED_EDGE('',*,*,#16938,.F.) ;
#23324 = ORIENTED_EDGE('',*,*,#16933,.F.) ;
#23325 = ORIENTED_EDGE('',*,*,#16934,.T.) ;
#23326 = ORIENTED_EDGE('',*,*,#16938,.T.) ;
#23327 = ORIENTED_EDGE('',*,*,#16939,.T.) ;
#23328 = ORIENTED_EDGE('',*,*,#16940,.T.) ;
#23329 = ORIENTED_EDGE('',*,*,#16941,.T.) ;
#23330 = ORIENTED_EDGE('',*,*,#16942,.T.) ;
#23331 = ORIENTED_EDGE('',*,*,#16943,.T.) ;
#23332 = ORIENTED_EDGE('',*,*,#16944,.T.) ;
#23333 = ORIENTED_EDGE('',*,*,#16945,.T.) ;
#23334 = ORIENTED_EDGE('',*,*,#16946,.T.) ;
#23335 = ORIENTED_EDGE('',*,*,#16947,.T.) ;
#23336 = ORIENTED_EDGE('',*,*,#16948,.T.) ;
#23337 = ORIENTED_EDGE('',*,*,#16949,.T.) ;
#23338 = ORIENTED_EDGE('',*,*,#16950,.T.) ;
#23339 = ORIENTED_EDGE('',*,*,#16951,.T.) ;
#23340 = ORIENTED_EDGE('',*,*,#16952,.T.) ;
#23341 = ORIENTED_EDGE('',*,*,#16953,.T.) ;
#23342 = ORIENTED_EDGE('',*,*,#16954,.T.) ;
#23343 = ORIENTED_EDGE('',*,*,#16955,.T.) ;
#23344 = ORIENTED_EDGE('',*,*,#16903,.T.) ;
#23345 = ORIENTED_EDGE('',*,*,#16904,.T.) ;
#23346 = ORIENTED_EDGE('',*,*,#16895,.T.) ;
#23347 = ORIENTED_EDGE('',*,*,#16899,.T.) ;
#23348 = ORIENTED_EDGE('',*,*,#16913,.T.) ;
#23349 = ORIENTED_EDGE('',*,*,#16916,.T.) ;
#23350 = ORIENTED_EDGE('',*,*,#16918,.T.) ;
#23351 = ORIENTED_EDGE('',*,*,#16919,.T.) ;
#23352 = ORIENTED_EDGE('',*,*,#16937,.T.) ;
#23353 = ORIENTED_EDGE('',*,*,#16956,.F.) ;
#23354 = ORIENTED_EDGE('',*,*,#16957,.T.) ;
#23355 = ORIENTED_EDGE('',*,*,#16939,.F.) ;
#23356 = ORIENTED_EDGE('',*,*,#16958,.T.) ;
#23357 = ORIENTED_EDGE('',*,*,#16959,.T.) ;
#23358 = ORIENTED_EDGE('',*,*,#16960,.T.) ;
#23359 = ORIENTED_EDGE('',*,*,#16961,.T.) ;
#23360 = ORIENTED_EDGE('',*,*,#16962,.T.) ;
#23361 = ORIENTED_EDGE('',*,*,#16963,.T.) ;
#23362 = ORIENTED_EDGE('',*,*,#16922,.T.) ;
#23363 = ORIENTED_EDGE('',*,*,#16928,.T.) ;
#23364 = ORIENTED_EDGE('',*,*,#16964,.T.) ;
#23365 = ORIENTED_EDGE('',*,*,#16945,.F.) ;
#23366 = ORIENTED_EDGE('',*,*,#16965,.F.) ;
#23367 = ORIENTED_EDGE('',*,*,#16959,.F.) ;
#23368 = ORIENTED_EDGE('',*,*,#16965,.T.) ;
#23369 = ORIENTED_EDGE('',*,*,#16944,.F.) ;
#23370 = ORIENTED_EDGE('',*,*,#16966,.F.) ;
#23371 = ORIENTED_EDGE('',*,*,#16960,.F.) ;
#23372 = ORIENTED_EDGE('',*,*,#16967,.T.) ;
#23373 = ORIENTED_EDGE('',*,*,#16963,.F.) ;
#23374 = ORIENTED_EDGE('',*,*,#16968,.T.) ;
#23375 = ORIENTED_EDGE('',*,*,#16949,.F.) ;
#23376 = ORIENTED_EDGE('',*,*,#16969,.T.) ;
#23377 = ORIENTED_EDGE('',*,*,#16950,.F.) ;
#23378 = ORIENTED_EDGE('',*,*,#16968,.F.) ;
#23379 = ORIENTED_EDGE('',*,*,#16962,.F.) ;
#23380 = ORIENTED_EDGE('',*,*,#16936,.T.) ;
#23381 = ORIENTED_EDGE('',*,*,#16970,.T.) ;
#23382 = ORIENTED_EDGE('',*,*,#16971,.T.) ;
#23383 = ORIENTED_EDGE('',*,*,#16972,.T.) ;
#23384 = ORIENTED_EDGE('',*,*,#16973,.T.) ;
#23385 = ORIENTED_EDGE('',*,*,#16956,.T.) ;
#23386 = ORIENTED_EDGE('',*,*,#16925,.T.) ;
#23387 = ORIENTED_EDGE('',*,*,#16931,.T.) ;
#23388 = ORIENTED_EDGE('',*,*,#16935,.T.) ;
#23389 = ORIENTED_EDGE('',*,*,#16955,.F.) ;
#23390 = ORIENTED_EDGE('',*,*,#16974,.F.) ;
#23391 = ORIENTED_EDGE('',*,*,#16970,.F.) ;
#23392 = ORIENTED_EDGE('',*,*,#16975,.T.) ;
#23393 = ORIENTED_EDGE('',*,*,#16940,.F.) ;
#23394 = ORIENTED_EDGE('',*,*,#16957,.F.) ;
#23395 = ORIENTED_EDGE('',*,*,#16973,.F.) ;
#23396 = ORIENTED_EDGE('',*,*,#16974,.T.) ;
#23397 = ORIENTED_EDGE('',*,*,#16954,.F.) ;
#23398 = ORIENTED_EDGE('',*,*,#16976,.F.) ;
#23399 = ORIENTED_EDGE('',*,*,#16971,.F.) ;
#23400 = ORIENTED_EDGE('',*,*,#16977,.F.) ;
#23401 = ORIENTED_EDGE('',*,*,#16978,.F.) ;
#23402 = ORIENTED_EDGE('',*,*,#16979,.F.) ;
#23403 = ORIENTED_EDGE('',*,*,#16946,.F.) ;
#23404 = ORIENTED_EDGE('',*,*,#16964,.F.) ;
#23405 = ORIENTED_EDGE('',*,*,#16958,.F.) ;
#23406 = ORIENTED_EDGE('',*,*,#16967,.F.) ;
#23407 = ORIENTED_EDGE('',*,*,#16948,.F.) ;
#23408 = ORIENTED_EDGE('',*,*,#16980,.T.) ;
#23409 = ORIENTED_EDGE('',*,*,#16981,.T.) ;
#23410 = ORIENTED_EDGE('',*,*,#16982,.T.) ;
#23411 = ORIENTED_EDGE('',*,*,#16983,.T.) ;
#23412 = ORIENTED_EDGE('',*,*,#16920,.T.) ;
#23413 = ORIENTED_EDGE('',*,*,#16923,.T.) ;
#23414 = ORIENTED_EDGE('',*,*,#16926,.T.) ;
#23415 = ORIENTED_EDGE('',*,*,#16929,.T.) ;
#23416 = ORIENTED_EDGE('',*,*,#16932,.T.) ;
#23417 = ORIENTED_EDGE('',*,*,#16978,.T.) ;
#23418 = ORIENTED_EDGE('',*,*,#16984,.T.) ;
#23419 = ORIENTED_EDGE('',*,*,#16979,.T.) ;
#23420 = ORIENTED_EDGE('',*,*,#16984,.F.) ;
#23421 = ORIENTED_EDGE('',*,*,#16977,.T.) ;
#23422 = ORIENTED_EDGE('',*,*,#16947,.F.) ;
#23423 = ORIENTED_EDGE('',*,*,#16985,.T.) ;
#23424 = ORIENTED_EDGE('',*,*,#16981,.F.) ;
#23425 = ORIENTED_EDGE('',*,*,#16986,.F.) ;
#23426 = ORIENTED_EDGE('',*,*,#16951,.F.) ;
#23427 = ORIENTED_EDGE('',*,*,#16969,.F.) ;
#23428 = ORIENTED_EDGE('',*,*,#16961,.F.) ;
#23429 = ORIENTED_EDGE('',*,*,#16966,.T.) ;
#23430 = ORIENTED_EDGE('',*,*,#16943,.F.) ;
#23431 = ORIENTED_EDGE('',*,*,#16987,.T.) ;
#23432 = ORIENTED_EDGE('',*,*,#16982,.F.) ;
#23433 = ORIENTED_EDGE('',*,*,#16985,.F.) ;
#23434 = ORIENTED_EDGE('',*,*,#16942,.F.) ;
#23435 = ORIENTED_EDGE('',*,*,#16988,.T.) ;
#23436 = ORIENTED_EDGE('',*,*,#16983,.F.) ;
#23437 = ORIENTED_EDGE('',*,*,#16987,.F.) ;
#23438 = ORIENTED_EDGE('',*,*,#16941,.F.) ;
#23439 = ORIENTED_EDGE('',*,*,#16975,.F.) ;
#23440 = ORIENTED_EDGE('',*,*,#16972,.F.) ;
#23441 = ORIENTED_EDGE('',*,*,#16976,.T.) ;
#23442 = ORIENTED_EDGE('',*,*,#16953,.F.) ;
#23443 = ORIENTED_EDGE('',*,*,#16986,.T.) ;
#23444 = ORIENTED_EDGE('',*,*,#16980,.F.) ;
#23445 = ORIENTED_EDGE('',*,*,#16988,.F.) ;
#23446 = ORIENTED_EDGE('',*,*,#16952,.F.) ;
#23447 = ORIENTED_EDGE('',*,*,#16989,.F.) ;
#23448 = ORIENTED_EDGE('',*,*,#16990,.F.) ;
#23449 = ORIENTED_EDGE('',*,*,#16991,.F.) ;
#23450 = ORIENTED_EDGE('',*,*,#16992,.F.) ;
#23451 = ORIENTED_EDGE('',*,*,#16991,.T.) ;
#23452 = ORIENTED_EDGE('',*,*,#16993,.F.) ;
#23453 = ORIENTED_EDGE('',*,*,#16994,.F.) ;
#23454 = ORIENTED_EDGE('',*,*,#16995,.F.) ;
#23455 = ORIENTED_EDGE('',*,*,#16996,.T.) ;
#23456 = ORIENTED_EDGE('',*,*,#16997,.T.) ;
#23457 = ORIENTED_EDGE('',*,*,#16998,.T.) ;
#23458 = ORIENTED_EDGE('',*,*,#16992,.T.) ;
#23459 = ORIENTED_EDGE('',*,*,#16995,.T.) ;
#23460 = ORIENTED_EDGE('',*,*,#16999,.T.) ;
#23461 = ORIENTED_EDGE('',*,*,#17000,.F.) ;
#23462 = ORIENTED_EDGE('',*,*,#17001,.F.) ;
#23463 = ORIENTED_EDGE('',*,*,#16996,.F.) ;
#23464 = ORIENTED_EDGE('',*,*,#17002,.T.) ;
#23465 = ORIENTED_EDGE('',*,*,#17003,.F.) ;
#23466 = ORIENTED_EDGE('',*,*,#17004,.T.) ;
#23467 = ORIENTED_EDGE('',*,*,#17003,.T.) ;
#23468 = ORIENTED_EDGE('',*,*,#17005,.T.) ;
#23469 = ORIENTED_EDGE('',*,*,#16993,.T.) ;
#23470 = ORIENTED_EDGE('',*,*,#16990,.T.) ;
#23471 = ORIENTED_EDGE('',*,*,#17006,.T.) ;
#23472 = ORIENTED_EDGE('',*,*,#17001,.T.) ;
#23473 = ORIENTED_EDGE('',*,*,#17007,.F.) ;
#23474 = ORIENTED_EDGE('',*,*,#17008,.F.) ;
#23475 = ORIENTED_EDGE('',*,*,#16997,.F.) ;
#23476 = ORIENTED_EDGE('',*,*,#17005,.F.) ;
#23477 = ORIENTED_EDGE('',*,*,#17002,.F.) ;
#23478 = ORIENTED_EDGE('',*,*,#16999,.F.) ;
#23479 = ORIENTED_EDGE('',*,*,#16994,.T.) ;
#23480 = ORIENTED_EDGE('',*,*,#17009,.F.) ;
#23481 = ORIENTED_EDGE('',*,*,#17010,.T.) ;
#23482 = ORIENTED_EDGE('',*,*,#17011,.F.) ;
#23483 = ORIENTED_EDGE('',*,*,#17010,.F.) ;
#23484 = ORIENTED_EDGE('',*,*,#17012,.F.) ;
#23485 = ORIENTED_EDGE('',*,*,#17013,.F.) ;
#23486 = ORIENTED_EDGE('',*,*,#17014,.F.) ;
#23487 = ORIENTED_EDGE('',*,*,#17015,.F.) ;
#23488 = ORIENTED_EDGE('',*,*,#17016,.T.) ;
#23489 = ORIENTED_EDGE('',*,*,#17017,.F.) ;
#23490 = ORIENTED_EDGE('',*,*,#17018,.F.) ;
#23491 = ORIENTED_EDGE('',*,*,#17019,.F.) ;
#23492 = ORIENTED_EDGE('',*,*,#17014,.T.) ;
#23493 = ORIENTED_EDGE('',*,*,#17020,.F.) ;
#23494 = ORIENTED_EDGE('',*,*,#17016,.F.) ;
#23495 = ORIENTED_EDGE('',*,*,#17021,.F.) ;
#23496 = ORIENTED_EDGE('',*,*,#17012,.T.) ;
#23497 = ORIENTED_EDGE('',*,*,#17022,.F.) ;
#23498 = ORIENTED_EDGE('',*,*,#17023,.T.) ;
#23499 = ORIENTED_EDGE('',*,*,#17024,.F.) ;
#23500 = ORIENTED_EDGE('',*,*,#17018,.T.) ;
#23501 = ORIENTED_EDGE('',*,*,#17025,.F.) ;
#23502 = ORIENTED_EDGE('',*,*,#17026,.F.) ;
#23503 = ORIENTED_EDGE('',*,*,#17006,.F.) ;
#23504 = ORIENTED_EDGE('',*,*,#16989,.T.) ;
#23505 = ORIENTED_EDGE('',*,*,#16998,.F.) ;
#23506 = ORIENTED_EDGE('',*,*,#17008,.T.) ;
#23507 = ORIENTED_EDGE('',*,*,#17027,.F.) ;
#23508 = ORIENTED_EDGE('',*,*,#17028,.F.) ;
#23509 = ORIENTED_EDGE('',*,*,#17029,.T.) ;
#23510 = ORIENTED_EDGE('',*,*,#17030,.F.) ;
#23511 = ORIENTED_EDGE('',*,*,#17029,.F.) ;
#23512 = ORIENTED_EDGE('',*,*,#17031,.T.) ;
#23513 = ORIENTED_EDGE('',*,*,#17032,.F.) ;
#23514 = ORIENTED_EDGE('',*,*,#17033,.F.) ;
#23515 = ORIENTED_EDGE('',*,*,#17034,.F.) ;
#23516 = ORIENTED_EDGE('',*,*,#17035,.T.) ;
#23517 = ORIENTED_EDGE('',*,*,#17036,.F.) ;
#23518 = ORIENTED_EDGE('',*,*,#17031,.F.) ;
#23519 = ORIENTED_EDGE('',*,*,#17037,.F.) ;
#23520 = ORIENTED_EDGE('',*,*,#17038,.F.) ;
#23521 = ORIENTED_EDGE('',*,*,#17039,.F.) ;
#23522 = ORIENTED_EDGE('',*,*,#17035,.F.) ;
#23523 = ORIENTED_EDGE('',*,*,#17040,.F.) ;
#23524 = ORIENTED_EDGE('',*,*,#17038,.T.) ;
#23525 = ORIENTED_EDGE('',*,*,#17041,.F.) ;
#23526 = ORIENTED_EDGE('',*,*,#17042,.T.) ;
#23527 = ORIENTED_EDGE('',*,*,#17043,.F.) ;
#23528 = ORIENTED_EDGE('',*,*,#17033,.T.) ;
#23529 = ORIENTED_EDGE('',*,*,#17044,.F.) ;
#23530 = ORIENTED_EDGE('',*,*,#17045,.F.) ;
#23531 = ORIENTED_EDGE('',*,*,#17046,.F.) ;
#23532 = ORIENTED_EDGE('',*,*,#17047,.F.) ;
#23533 = ORIENTED_EDGE('',*,*,#17048,.T.) ;
#23534 = ORIENTED_EDGE('',*,*,#17049,.F.) ;
#23535 = ORIENTED_EDGE('',*,*,#17048,.F.) ;
#23536 = ORIENTED_EDGE('',*,*,#17000,.T.) ;
#23537 = ORIENTED_EDGE('',*,*,#17050,.T.) ;
#23538 = ORIENTED_EDGE('',*,*,#17041,.T.) ;
#23539 = ORIENTED_EDGE('',*,*,#17040,.T.) ;
#23540 = ORIENTED_EDGE('',*,*,#17037,.T.) ;
#23541 = ORIENTED_EDGE('',*,*,#17034,.T.) ;
#23542 = ORIENTED_EDGE('',*,*,#17046,.T.) ;
#23543 = ORIENTED_EDGE('',*,*,#17051,.T.) ;
#23544 = ORIENTED_EDGE('',*,*,#17022,.T.) ;
#23545 = ORIENTED_EDGE('',*,*,#17015,.T.) ;
#23546 = ORIENTED_EDGE('',*,*,#17021,.T.) ;
#23547 = ORIENTED_EDGE('',*,*,#17019,.T.) ;
#23548 = ORIENTED_EDGE('',*,*,#17027,.T.) ;
#23549 = ORIENTED_EDGE('',*,*,#17007,.T.) ;
#23550 = ORIENTED_EDGE('',*,*,#17011,.T.) ;
#23551 = ORIENTED_EDGE('',*,*,#17030,.T.) ;
#23552 = ORIENTED_EDGE('',*,*,#17049,.T.) ;
#23553 = ORIENTED_EDGE('',*,*,#17025,.T.) ;
#23554 = ORIENTED_EDGE('',*,*,#17017,.T.) ;
#23555 = ORIENTED_EDGE('',*,*,#17020,.T.) ;
#23556 = ORIENTED_EDGE('',*,*,#17013,.T.) ;
#23557 = ORIENTED_EDGE('',*,*,#17024,.T.) ;
#23558 = ORIENTED_EDGE('',*,*,#17052,.T.) ;
#23559 = ORIENTED_EDGE('',*,*,#17044,.T.) ;
#23560 = ORIENTED_EDGE('',*,*,#17032,.T.) ;
#23561 = ORIENTED_EDGE('',*,*,#17036,.T.) ;
#23562 = ORIENTED_EDGE('',*,*,#17039,.T.) ;
#23563 = ORIENTED_EDGE('',*,*,#17043,.T.) ;
#23564 = ORIENTED_EDGE('',*,*,#17053,.T.) ;
#23565 = ORIENTED_EDGE('',*,*,#17009,.T.) ;
#23566 = ORIENTED_EDGE('',*,*,#17028,.T.) ;
#23567 = ORIENTED_EDGE('',*,*,#17047,.T.) ;
#23568 = ORIENTED_EDGE('',*,*,#17045,.T.) ;
#23569 = ORIENTED_EDGE('',*,*,#17052,.F.) ;
#23570 = ORIENTED_EDGE('',*,*,#17023,.F.) ;
#23571 = ORIENTED_EDGE('',*,*,#17051,.F.) ;
#23572 = ORIENTED_EDGE('',*,*,#17026,.T.) ;
#23573 = ORIENTED_EDGE('',*,*,#17053,.F.) ;
#23574 = ORIENTED_EDGE('',*,*,#17042,.F.) ;
#23575 = ORIENTED_EDGE('',*,*,#17050,.F.) ;
#23576 = ORIENTED_EDGE('',*,*,#17004,.F.) ;
#23577 = ORIENTED_EDGE('',*,*,#17054,.F.) ;
#23578 = ORIENTED_EDGE('',*,*,#17055,.F.) ;
#23579 = ORIENTED_EDGE('',*,*,#17056,.F.) ;
#23580 = ORIENTED_EDGE('',*,*,#17057,.F.) ;
#23581 = ORIENTED_EDGE('',*,*,#17058,.F.) ;
#23582 = ORIENTED_EDGE('',*,*,#17057,.T.) ;
#23583 = ORIENTED_EDGE('',*,*,#17059,.F.) ;
#23584 = ORIENTED_EDGE('',*,*,#17060,.F.) ;
#23585 = ORIENTED_EDGE('',*,*,#17061,.F.) ;
#23586 = ORIENTED_EDGE('',*,*,#17059,.T.) ;
#23587 = ORIENTED_EDGE('',*,*,#17056,.T.) ;
#23588 = ORIENTED_EDGE('',*,*,#17062,.F.) ;
#23589 = ORIENTED_EDGE('',*,*,#17063,.F.) ;
#23590 = ORIENTED_EDGE('',*,*,#17064,.F.) ;
#23591 = ORIENTED_EDGE('',*,*,#17062,.T.) ;
#23592 = ORIENTED_EDGE('',*,*,#17055,.T.) ;
#23593 = ORIENTED_EDGE('',*,*,#17063,.T.) ;
#23594 = ORIENTED_EDGE('',*,*,#17054,.T.) ;
#23595 = ORIENTED_EDGE('',*,*,#17058,.T.) ;
#23596 = ORIENTED_EDGE('',*,*,#17065,.F.) ;
#23597 = ORIENTED_EDGE('',*,*,#17066,.T.) ;
#23598 = ORIENTED_EDGE('',*,*,#17067,.T.) ;
#23599 = ORIENTED_EDGE('',*,*,#17068,.T.) ;
#23600 = ORIENTED_EDGE('',*,*,#17069,.F.) ;
#23601 = ORIENTED_EDGE('',*,*,#17070,.T.) ;
#23602 = ORIENTED_EDGE('',*,*,#17071,.T.) ;
#23603 = ORIENTED_EDGE('',*,*,#17072,.T.) ;
#23604 = ORIENTED_EDGE('',*,*,#17073,.F.) ;
#23605 = ORIENTED_EDGE('',*,*,#17074,.T.) ;
#23606 = ORIENTED_EDGE('',*,*,#17075,.T.) ;
#23607 = ORIENTED_EDGE('',*,*,#17076,.T.) ;
#23608 = ORIENTED_EDGE('',*,*,#17077,.F.) ;
#23609 = ORIENTED_EDGE('',*,*,#17078,.T.) ;
#23610 = ORIENTED_EDGE('',*,*,#17079,.T.) ;
#23611 = ORIENTED_EDGE('',*,*,#17080,.T.) ;
#23612 = ORIENTED_EDGE('',*,*,#17081,.F.) ;
#23613 = ORIENTED_EDGE('',*,*,#17082,.T.) ;
#23614 = ORIENTED_EDGE('',*,*,#17083,.T.) ;
#23615 = ORIENTED_EDGE('',*,*,#17084,.T.) ;
#23616 = ORIENTED_EDGE('',*,*,#17085,.F.) ;
#23617 = ORIENTED_EDGE('',*,*,#17086,.T.) ;
#23618 = ORIENTED_EDGE('',*,*,#17087,.T.) ;
#23619 = ORIENTED_EDGE('',*,*,#17088,.T.) ;
#23620 = ORIENTED_EDGE('',*,*,#17089,.F.) ;
#23621 = ORIENTED_EDGE('',*,*,#17090,.T.) ;
#23622 = ORIENTED_EDGE('',*,*,#17091,.T.) ;
#23623 = ORIENTED_EDGE('',*,*,#17092,.T.) ;
#23624 = ORIENTED_EDGE('',*,*,#17093,.F.) ;
#23625 = ORIENTED_EDGE('',*,*,#17094,.T.) ;
#23626 = ORIENTED_EDGE('',*,*,#17095,.T.) ;
#23627 = ORIENTED_EDGE('',*,*,#17096,.T.) ;
#23628 = ORIENTED_EDGE('',*,*,#17097,.F.) ;
#23629 = ORIENTED_EDGE('',*,*,#17098,.T.) ;
#23630 = ORIENTED_EDGE('',*,*,#17099,.F.) ;
#23631 = ORIENTED_EDGE('',*,*,#17100,.F.) ;
#23632 = ORIENTED_EDGE('',*,*,#17101,.F.) ;
#23633 = ORIENTED_EDGE('',*,*,#17102,.F.) ;
#23634 = ORIENTED_EDGE('',*,*,#17103,.T.) ;
#23635 = ORIENTED_EDGE('',*,*,#17104,.T.) ;
#23636 = ORIENTED_EDGE('',*,*,#17105,.F.) ;
#23637 = ORIENTED_EDGE('',*,*,#17106,.F.) ;
#23638 = ORIENTED_EDGE('',*,*,#17105,.T.) ;
#23639 = ORIENTED_EDGE('',*,*,#17107,.T.) ;
#23640 = ORIENTED_EDGE('',*,*,#17066,.F.) ;
#23641 = ORIENTED_EDGE('',*,*,#17067,.F.) ;
#23642 = ORIENTED_EDGE('',*,*,#17107,.F.) ;
#23643 = ORIENTED_EDGE('',*,*,#17104,.F.) ;
#23644 = ORIENTED_EDGE('',*,*,#17108,.F.) ;
#23645 = ORIENTED_EDGE('',*,*,#17109,.F.) ;
#23646 = ORIENTED_EDGE('',*,*,#17068,.F.) ;
#23647 = ORIENTED_EDGE('',*,*,#17108,.T.) ;
#23648 = ORIENTED_EDGE('',*,*,#17103,.F.) ;
#23649 = ORIENTED_EDGE('',*,*,#17064,.T.) ;
#23650 = ORIENTED_EDGE('',*,*,#17101,.T.) ;
#23651 = ORIENTED_EDGE('',*,*,#17110,.T.) ;
#23652 = ORIENTED_EDGE('',*,*,#17111,.T.) ;
#23653 = ORIENTED_EDGE('',*,*,#17112,.T.) ;
#23654 = ORIENTED_EDGE('',*,*,#17097,.T.) ;
#23655 = ORIENTED_EDGE('',*,*,#17113,.T.) ;
#23656 = ORIENTED_EDGE('',*,*,#17114,.T.) ;
#23657 = ORIENTED_EDGE('',*,*,#17115,.T.) ;
#23658 = ORIENTED_EDGE('',*,*,#17093,.T.) ;
#23659 = ORIENTED_EDGE('',*,*,#17116,.T.) ;
#23660 = ORIENTED_EDGE('',*,*,#17117,.T.) ;
#23661 = ORIENTED_EDGE('',*,*,#17118,.T.) ;
#23662 = ORIENTED_EDGE('',*,*,#17089,.T.) ;
#23663 = ORIENTED_EDGE('',*,*,#17119,.T.) ;
#23664 = ORIENTED_EDGE('',*,*,#17120,.T.) ;
#23665 = ORIENTED_EDGE('',*,*,#17121,.T.) ;
#23666 = ORIENTED_EDGE('',*,*,#17085,.T.) ;
#23667 = ORIENTED_EDGE('',*,*,#17122,.T.) ;
#23668 = ORIENTED_EDGE('',*,*,#17123,.T.) ;
#23669 = ORIENTED_EDGE('',*,*,#17124,.T.) ;
#23670 = ORIENTED_EDGE('',*,*,#17081,.T.) ;
#23671 = ORIENTED_EDGE('',*,*,#17125,.T.) ;
#23672 = ORIENTED_EDGE('',*,*,#17126,.T.) ;
#23673 = ORIENTED_EDGE('',*,*,#17127,.T.) ;
#23674 = ORIENTED_EDGE('',*,*,#17077,.T.) ;
#23675 = ORIENTED_EDGE('',*,*,#17128,.T.) ;
#23676 = ORIENTED_EDGE('',*,*,#17129,.T.) ;
#23677 = ORIENTED_EDGE('',*,*,#17130,.T.) ;
#23678 = ORIENTED_EDGE('',*,*,#17073,.T.) ;
#23679 = ORIENTED_EDGE('',*,*,#17131,.T.) ;
#23680 = ORIENTED_EDGE('',*,*,#17132,.T.) ;
#23681 = ORIENTED_EDGE('',*,*,#17133,.T.) ;
#23682 = ORIENTED_EDGE('',*,*,#17069,.T.) ;
#23683 = ORIENTED_EDGE('',*,*,#17109,.T.) ;
#23684 = ORIENTED_EDGE('',*,*,#17102,.T.) ;
#23685 = ORIENTED_EDGE('',*,*,#17106,.T.) ;
#23686 = ORIENTED_EDGE('',*,*,#17065,.T.) ;
#23687 = ORIENTED_EDGE('',*,*,#17060,.T.) ;
#23688 = ORIENTED_EDGE('',*,*,#17061,.T.) ;
#23689 = ORIENTED_EDGE('',*,*,#17071,.F.) ;
#23690 = ORIENTED_EDGE('',*,*,#17134,.F.) ;
#23691 = ORIENTED_EDGE('',*,*,#17135,.F.) ;
#23692 = ORIENTED_EDGE('',*,*,#17136,.F.) ;
#23693 = ORIENTED_EDGE('',*,*,#17072,.F.) ;
#23694 = ORIENTED_EDGE('',*,*,#17136,.T.) ;
#23695 = ORIENTED_EDGE('',*,*,#17137,.F.) ;
#23696 = ORIENTED_EDGE('',*,*,#17131,.F.) ;
#23697 = ORIENTED_EDGE('',*,*,#17132,.F.) ;
#23698 = ORIENTED_EDGE('',*,*,#17137,.T.) ;
#23699 = ORIENTED_EDGE('',*,*,#17135,.T.) ;
#23700 = ORIENTED_EDGE('',*,*,#17138,.F.) ;
#23701 = ORIENTED_EDGE('',*,*,#17070,.F.) ;
#23702 = ORIENTED_EDGE('',*,*,#17133,.F.) ;
#23703 = ORIENTED_EDGE('',*,*,#17138,.T.) ;
#23704 = ORIENTED_EDGE('',*,*,#17134,.T.) ;
#23705 = ORIENTED_EDGE('',*,*,#17129,.F.) ;
#23706 = ORIENTED_EDGE('',*,*,#17139,.T.) ;
#23707 = ORIENTED_EDGE('',*,*,#17140,.T.) ;
#23708 = ORIENTED_EDGE('',*,*,#17141,.F.) ;
#23709 = ORIENTED_EDGE('',*,*,#17130,.F.) ;
#23710 = ORIENTED_EDGE('',*,*,#17141,.T.) ;
#23711 = ORIENTED_EDGE('',*,*,#17142,.T.) ;
#23712 = ORIENTED_EDGE('',*,*,#17074,.F.) ;
#23713 = ORIENTED_EDGE('',*,*,#17075,.F.) ;
#23714 = ORIENTED_EDGE('',*,*,#17142,.F.) ;
#23715 = ORIENTED_EDGE('',*,*,#17140,.F.) ;
#23716 = ORIENTED_EDGE('',*,*,#17143,.F.) ;
#23717 = ORIENTED_EDGE('',*,*,#17128,.F.) ;
#23718 = ORIENTED_EDGE('',*,*,#17076,.F.) ;
#23719 = ORIENTED_EDGE('',*,*,#17143,.T.) ;
#23720 = ORIENTED_EDGE('',*,*,#17139,.F.) ;
#23721 = ORIENTED_EDGE('',*,*,#17079,.F.) ;
#23722 = ORIENTED_EDGE('',*,*,#17144,.F.) ;
#23723 = ORIENTED_EDGE('',*,*,#17145,.F.) ;
#23724 = ORIENTED_EDGE('',*,*,#17146,.F.) ;
#23725 = ORIENTED_EDGE('',*,*,#17080,.F.) ;
#23726 = ORIENTED_EDGE('',*,*,#17146,.T.) ;
#23727 = ORIENTED_EDGE('',*,*,#17147,.F.) ;
#23728 = ORIENTED_EDGE('',*,*,#17125,.F.) ;
#23729 = ORIENTED_EDGE('',*,*,#17126,.F.) ;
#23730 = ORIENTED_EDGE('',*,*,#17147,.T.) ;
#23731 = ORIENTED_EDGE('',*,*,#17145,.T.) ;
#23732 = ORIENTED_EDGE('',*,*,#17148,.F.) ;
#23733 = ORIENTED_EDGE('',*,*,#17078,.F.) ;
#23734 = ORIENTED_EDGE('',*,*,#17127,.F.) ;
#23735 = ORIENTED_EDGE('',*,*,#17148,.T.) ;
#23736 = ORIENTED_EDGE('',*,*,#17144,.T.) ;
#23737 = ORIENTED_EDGE('',*,*,#17123,.F.) ;
#23738 = ORIENTED_EDGE('',*,*,#17149,.T.) ;
#23739 = ORIENTED_EDGE('',*,*,#17150,.T.) ;
#23740 = ORIENTED_EDGE('',*,*,#17151,.F.) ;
#23741 = ORIENTED_EDGE('',*,*,#17124,.F.) ;
#23742 = ORIENTED_EDGE('',*,*,#17151,.T.) ;
#23743 = ORIENTED_EDGE('',*,*,#17152,.T.) ;
#23744 = ORIENTED_EDGE('',*,*,#17082,.F.) ;
#23745 = ORIENTED_EDGE('',*,*,#17083,.F.) ;
#23746 = ORIENTED_EDGE('',*,*,#17152,.F.) ;
#23747 = ORIENTED_EDGE('',*,*,#17150,.F.) ;
#23748 = ORIENTED_EDGE('',*,*,#17153,.F.) ;
#23749 = ORIENTED_EDGE('',*,*,#17122,.F.) ;
#23750 = ORIENTED_EDGE('',*,*,#17084,.F.) ;
#23751 = ORIENTED_EDGE('',*,*,#17153,.T.) ;
#23752 = ORIENTED_EDGE('',*,*,#17149,.F.) ;
#23753 = ORIENTED_EDGE('',*,*,#17087,.F.) ;
#23754 = ORIENTED_EDGE('',*,*,#17154,.F.) ;
#23755 = ORIENTED_EDGE('',*,*,#17155,.F.) ;
#23756 = ORIENTED_EDGE('',*,*,#17156,.F.) ;
#23757 = ORIENTED_EDGE('',*,*,#17088,.F.) ;
#23758 = ORIENTED_EDGE('',*,*,#17156,.T.) ;
#23759 = ORIENTED_EDGE('',*,*,#17157,.F.) ;
#23760 = ORIENTED_EDGE('',*,*,#17119,.F.) ;
#23761 = ORIENTED_EDGE('',*,*,#17120,.F.) ;
#23762 = ORIENTED_EDGE('',*,*,#17157,.T.) ;
#23763 = ORIENTED_EDGE('',*,*,#17155,.T.) ;
#23764 = ORIENTED_EDGE('',*,*,#17158,.F.) ;
#23765 = ORIENTED_EDGE('',*,*,#17086,.F.) ;
#23766 = ORIENTED_EDGE('',*,*,#17121,.F.) ;
#23767 = ORIENTED_EDGE('',*,*,#17158,.T.) ;
#23768 = ORIENTED_EDGE('',*,*,#17154,.T.) ;
#23769 = ORIENTED_EDGE('',*,*,#17117,.F.) ;
#23770 = ORIENTED_EDGE('',*,*,#17159,.T.) ;
#23771 = ORIENTED_EDGE('',*,*,#17160,.T.) ;
#23772 = ORIENTED_EDGE('',*,*,#17161,.F.) ;
#23773 = ORIENTED_EDGE('',*,*,#17118,.F.) ;
#23774 = ORIENTED_EDGE('',*,*,#17161,.T.) ;
#23775 = ORIENTED_EDGE('',*,*,#17162,.T.) ;
#23776 = ORIENTED_EDGE('',*,*,#17090,.F.) ;
#23777 = ORIENTED_EDGE('',*,*,#17091,.F.) ;
#23778 = ORIENTED_EDGE('',*,*,#17162,.F.) ;
#23779 = ORIENTED_EDGE('',*,*,#17160,.F.) ;
#23780 = ORIENTED_EDGE('',*,*,#17163,.F.) ;
#23781 = ORIENTED_EDGE('',*,*,#17116,.F.) ;
#23782 = ORIENTED_EDGE('',*,*,#17092,.F.) ;
#23783 = ORIENTED_EDGE('',*,*,#17163,.T.) ;
#23784 = ORIENTED_EDGE('',*,*,#17159,.F.) ;
#23785 = ORIENTED_EDGE('',*,*,#17095,.F.) ;
#23786 = ORIENTED_EDGE('',*,*,#17164,.F.) ;
#23787 = ORIENTED_EDGE('',*,*,#17165,.F.) ;
#23788 = ORIENTED_EDGE('',*,*,#17166,.F.) ;
#23789 = ORIENTED_EDGE('',*,*,#17096,.F.) ;
#23790 = ORIENTED_EDGE('',*,*,#17166,.T.) ;
#23791 = ORIENTED_EDGE('',*,*,#17167,.F.) ;
#23792 = ORIENTED_EDGE('',*,*,#17113,.F.) ;
#23793 = ORIENTED_EDGE('',*,*,#17114,.F.) ;
#23794 = ORIENTED_EDGE('',*,*,#17167,.T.) ;
#23795 = ORIENTED_EDGE('',*,*,#17165,.T.) ;
#23796 = ORIENTED_EDGE('',*,*,#17168,.F.) ;
#23797 = ORIENTED_EDGE('',*,*,#17094,.F.) ;
#23798 = ORIENTED_EDGE('',*,*,#17115,.F.) ;
#23799 = ORIENTED_EDGE('',*,*,#17168,.T.) ;
#23800 = ORIENTED_EDGE('',*,*,#17164,.T.) ;
#23801 = ORIENTED_EDGE('',*,*,#17169,.T.) ;
#23802 = ORIENTED_EDGE('',*,*,#17099,.T.) ;
#23803 = ORIENTED_EDGE('',*,*,#17170,.T.) ;
#23804 = ORIENTED_EDGE('',*,*,#17171,.T.) ;
#23805 = ORIENTED_EDGE('',*,*,#17172,.T.) ;
#23806 = ORIENTED_EDGE('',*,*,#17170,.F.) ;
#23807 = ORIENTED_EDGE('',*,*,#17098,.F.) ;
#23808 = ORIENTED_EDGE('',*,*,#17112,.F.) ;
#23809 = ORIENTED_EDGE('',*,*,#17173,.T.) ;
#23810 = ORIENTED_EDGE('',*,*,#17171,.F.) ;
#23811 = ORIENTED_EDGE('',*,*,#17172,.F.) ;
#23812 = ORIENTED_EDGE('',*,*,#17111,.F.) ;
#23813 = ORIENTED_EDGE('',*,*,#17100,.T.) ;
#23814 = ORIENTED_EDGE('',*,*,#17169,.F.) ;
#23815 = ORIENTED_EDGE('',*,*,#17173,.F.) ;
#23816 = ORIENTED_EDGE('',*,*,#17110,.F.) ;
#23817 = ORIENTED_EDGE('',*,*,#17174,.F.) ;
#23818 = ORIENTED_EDGE('',*,*,#17175,.T.) ;
#23819 = ORIENTED_EDGE('',*,*,#17176,.F.) ;
#23820 = ORIENTED_EDGE('',*,*,#17175,.F.) ;
#23821 = ORIENTED_EDGE('',*,*,#17177,.F.) ;
#23822 = ORIENTED_EDGE('',*,*,#17178,.T.) ;
#23823 = ORIENTED_EDGE('',*,*,#17179,.F.) ;
#23824 = ORIENTED_EDGE('',*,*,#17178,.F.) ;
#23825 = ORIENTED_EDGE('',*,*,#17180,.F.) ;
#23826 = ORIENTED_EDGE('',*,*,#17181,.T.) ;
#23827 = ORIENTED_EDGE('',*,*,#17182,.F.) ;
#23828 = ORIENTED_EDGE('',*,*,#17181,.F.) ;
#23829 = ORIENTED_EDGE('',*,*,#17183,.F.) ;
#23830 = ORIENTED_EDGE('',*,*,#17184,.T.) ;
#23831 = ORIENTED_EDGE('',*,*,#17185,.F.) ;
#23832 = ORIENTED_EDGE('',*,*,#17184,.F.) ;
#23833 = ORIENTED_EDGE('',*,*,#17186,.F.) ;
#23834 = ORIENTED_EDGE('',*,*,#17187,.F.) ;
#23835 = ORIENTED_EDGE('',*,*,#17188,.F.) ;
#23836 = ORIENTED_EDGE('',*,*,#17189,.F.) ;
#23837 = ORIENTED_EDGE('',*,*,#17190,.F.) ;
#23838 = ORIENTED_EDGE('',*,*,#17191,.F.) ;
#23839 = ORIENTED_EDGE('',*,*,#17192,.T.) ;
#23840 = ORIENTED_EDGE('',*,*,#17193,.T.) ;
#23841 = ORIENTED_EDGE('',*,*,#17194,.T.) ;
#23842 = ORIENTED_EDGE('',*,*,#17195,.T.) ;
#23843 = ORIENTED_EDGE('',*,*,#17174,.T.) ;
#23844 = ORIENTED_EDGE('',*,*,#17177,.T.) ;
#23845 = ORIENTED_EDGE('',*,*,#17180,.T.) ;
#23846 = ORIENTED_EDGE('',*,*,#17183,.T.) ;
#23847 = ORIENTED_EDGE('',*,*,#17187,.T.) ;
#23848 = ORIENTED_EDGE('',*,*,#17196,.T.) ;
#23849 = ORIENTED_EDGE('',*,*,#17188,.T.) ;
#23850 = ORIENTED_EDGE('',*,*,#17196,.F.) ;
#23851 = ORIENTED_EDGE('',*,*,#17186,.T.) ;
#23852 = ORIENTED_EDGE('',*,*,#17197,.T.) ;
#23853 = ORIENTED_EDGE('',*,*,#17198,.T.) ;
#23854 = ORIENTED_EDGE('',*,*,#17199,.F.) ;
#23855 = ORIENTED_EDGE('',*,*,#17200,.T.) ;
#23856 = ORIENTED_EDGE('',*,*,#17201,.F.) ;
#23857 = ORIENTED_EDGE('',*,*,#17191,.T.) ;
#23858 = ORIENTED_EDGE('',*,*,#17202,.F.) ;
#23859 = ORIENTED_EDGE('',*,*,#17200,.F.) ;
#23860 = ORIENTED_EDGE('',*,*,#17203,.T.) ;
#23861 = ORIENTED_EDGE('',*,*,#17204,.T.) ;
#23862 = ORIENTED_EDGE('',*,*,#17205,.T.) ;
#23863 = ORIENTED_EDGE('',*,*,#17206,.T.) ;
#23864 = ORIENTED_EDGE('',*,*,#17176,.T.) ;
#23865 = ORIENTED_EDGE('',*,*,#17179,.T.) ;
#23866 = ORIENTED_EDGE('',*,*,#17182,.T.) ;
#23867 = ORIENTED_EDGE('',*,*,#17185,.T.) ;
#23868 = ORIENTED_EDGE('',*,*,#17190,.T.) ;
#23869 = ORIENTED_EDGE('',*,*,#17201,.T.) ;
#23870 = ORIENTED_EDGE('',*,*,#17202,.T.) ;
#23871 = ORIENTED_EDGE('',*,*,#17207,.T.) ;
#23872 = ORIENTED_EDGE('',*,*,#17193,.F.) ;
#23873 = ORIENTED_EDGE('',*,*,#17208,.F.) ;
#23874 = ORIENTED_EDGE('',*,*,#17206,.F.) ;
#23875 = ORIENTED_EDGE('',*,*,#17209,.T.) ;
#23876 = ORIENTED_EDGE('',*,*,#17194,.F.) ;
#23877 = ORIENTED_EDGE('',*,*,#17207,.F.) ;
#23878 = ORIENTED_EDGE('',*,*,#17205,.F.) ;
#23879 = ORIENTED_EDGE('',*,*,#17210,.T.) ;
#23880 = ORIENTED_EDGE('',*,*,#17195,.F.) ;
#23881 = ORIENTED_EDGE('',*,*,#17209,.F.) ;
#23882 = ORIENTED_EDGE('',*,*,#17204,.F.) ;
#23883 = ORIENTED_EDGE('',*,*,#17208,.T.) ;
#23884 = ORIENTED_EDGE('',*,*,#17192,.F.) ;
#23885 = ORIENTED_EDGE('',*,*,#17210,.F.) ;
#23886 = ORIENTED_EDGE('',*,*,#17203,.F.) ;
#23887 = ORIENTED_EDGE('',*,*,#17189,.T.) ;
#23888 = ORIENTED_EDGE('',*,*,#17198,.F.) ;
#23889 = ORIENTED_EDGE('',*,*,#17211,.T.) ;
#23890 = ORIENTED_EDGE('',*,*,#17212,.F.) ;
#23891 = ORIENTED_EDGE('',*,*,#17211,.F.) ;
#23892 = ORIENTED_EDGE('',*,*,#17197,.F.) ;
#23893 = ORIENTED_EDGE('',*,*,#17199,.T.) ;
#23894 = ORIENTED_EDGE('',*,*,#17212,.T.) ;
#23895 = ORIENTED_EDGE('',*,*,#17213,.F.) ;
#23896 = ORIENTED_EDGE('',*,*,#17214,.T.) ;
#23897 = ORIENTED_EDGE('',*,*,#17215,.T.) ;
#23898 = ORIENTED_EDGE('',*,*,#17214,.F.) ;
#23899 = ORIENTED_EDGE('',*,*,#17215,.F.) ;
#23900 = ORIENTED_EDGE('',*,*,#17216,.T.) ;
#23901 = ORIENTED_EDGE('',*,*,#17217,.F.) ;
#23902 = ORIENTED_EDGE('',*,*,#17216,.F.) ;
#23903 = ORIENTED_EDGE('',*,*,#17218,.F.) ;
#23904 = ORIENTED_EDGE('',*,*,#17219,.T.) ;
#23905 = ORIENTED_EDGE('',*,*,#17220,.F.) ;
#23906 = ORIENTED_EDGE('',*,*,#17219,.F.) ;
#23907 = ORIENTED_EDGE('',*,*,#17220,.T.) ;
#23908 = ORIENTED_EDGE('',*,*,#17213,.T.) ;
#23909 = ORIENTED_EDGE('',*,*,#17218,.T.) ;
#23910 = ORIENTED_EDGE('',*,*,#17217,.T.) ;
#23911 = ORIENTED_EDGE('',*,*,#17221,.T.) ;
#23912 = ORIENTED_EDGE('',*,*,#17222,.T.) ;
#23913 = ORIENTED_EDGE('',*,*,#17223,.T.) ;
#23914 = ORIENTED_EDGE('',*,*,#17224,.T.) ;
#23915 = ORIENTED_EDGE('',*,*,#17221,.F.) ;
#23916 = ORIENTED_EDGE('',*,*,#17225,.T.) ;
#23917 = ORIENTED_EDGE('',*,*,#17223,.F.) ;
#23918 = ORIENTED_EDGE('',*,*,#17225,.F.) ;
#23919 = ORIENTED_EDGE('',*,*,#17224,.F.) ;
#23920 = ORIENTED_EDGE('',*,*,#17226,.T.) ;
#23921 = ORIENTED_EDGE('',*,*,#17222,.F.) ;
#23922 = ORIENTED_EDGE('',*,*,#17226,.F.) ;
#23923 = ORIENTED_EDGE('',*,*,#17227,.F.) ;
#23924 = ORIENTED_EDGE('',*,*,#17228,.T.) ;
#23925 = ORIENTED_EDGE('',*,*,#17229,.F.) ;
#23926 = ORIENTED_EDGE('',*,*,#17228,.F.) ;
#23927 = ORIENTED_EDGE('',*,*,#17230,.F.) ;
#23928 = ORIENTED_EDGE('',*,*,#17231,.T.) ;
#23929 = ORIENTED_EDGE('',*,*,#17232,.F.) ;
#23930 = ORIENTED_EDGE('',*,*,#17231,.F.) ;
#23931 = ORIENTED_EDGE('',*,*,#17233,.F.) ;
#23932 = ORIENTED_EDGE('',*,*,#17234,.T.) ;
#23933 = ORIENTED_EDGE('',*,*,#17235,.F.) ;
#23934 = ORIENTED_EDGE('',*,*,#17234,.F.) ;
#23935 = ORIENTED_EDGE('',*,*,#17236,.F.) ;
#23936 = ORIENTED_EDGE('',*,*,#17237,.T.) ;
#23937 = ORIENTED_EDGE('',*,*,#17238,.F.) ;
#23938 = ORIENTED_EDGE('',*,*,#17237,.F.) ;
#23939 = ORIENTED_EDGE('',*,*,#17239,.F.) ;
#23940 = ORIENTED_EDGE('',*,*,#17240,.T.) ;
#23941 = ORIENTED_EDGE('',*,*,#17241,.F.) ;
#23942 = ORIENTED_EDGE('',*,*,#17240,.F.) ;
#23943 = ORIENTED_EDGE('',*,*,#17242,.F.) ;
#23944 = ORIENTED_EDGE('',*,*,#17243,.T.) ;
#23945 = ORIENTED_EDGE('',*,*,#17244,.F.) ;
#23946 = ORIENTED_EDGE('',*,*,#17243,.F.) ;
#23947 = ORIENTED_EDGE('',*,*,#17245,.F.) ;
#23948 = ORIENTED_EDGE('',*,*,#17246,.T.) ;
#23949 = ORIENTED_EDGE('',*,*,#17247,.F.) ;
#23950 = ORIENTED_EDGE('',*,*,#17246,.F.) ;
#23951 = ORIENTED_EDGE('',*,*,#17248,.F.) ;
#23952 = ORIENTED_EDGE('',*,*,#17249,.T.) ;
#23953 = ORIENTED_EDGE('',*,*,#17250,.F.) ;
#23954 = ORIENTED_EDGE('',*,*,#17249,.F.) ;
#23955 = ORIENTED_EDGE('',*,*,#17251,.F.) ;
#23956 = ORIENTED_EDGE('',*,*,#17252,.F.) ;
#23957 = ORIENTED_EDGE('',*,*,#17253,.F.) ;
#23958 = ORIENTED_EDGE('',*,*,#17254,.F.) ;
#23959 = ORIENTED_EDGE('',*,*,#17253,.T.) ;
#23960 = ORIENTED_EDGE('',*,*,#17255,.T.) ;
#23961 = ORIENTED_EDGE('',*,*,#17250,.T.) ;
#23962 = ORIENTED_EDGE('',*,*,#17247,.T.) ;
#23963 = ORIENTED_EDGE('',*,*,#17244,.T.) ;
#23964 = ORIENTED_EDGE('',*,*,#17241,.T.) ;
#23965 = ORIENTED_EDGE('',*,*,#17238,.T.) ;
#23966 = ORIENTED_EDGE('',*,*,#17235,.T.) ;
#23967 = ORIENTED_EDGE('',*,*,#17232,.T.) ;
#23968 = ORIENTED_EDGE('',*,*,#17229,.T.) ;
#23969 = ORIENTED_EDGE('',*,*,#17251,.T.) ;
#23970 = ORIENTED_EDGE('',*,*,#17256,.T.) ;
#23971 = ORIENTED_EDGE('',*,*,#17248,.T.) ;
#23972 = ORIENTED_EDGE('',*,*,#17245,.T.) ;
#23973 = ORIENTED_EDGE('',*,*,#17242,.T.) ;
#23974 = ORIENTED_EDGE('',*,*,#17239,.T.) ;
#23975 = ORIENTED_EDGE('',*,*,#17236,.T.) ;
#23976 = ORIENTED_EDGE('',*,*,#17233,.T.) ;
#23977 = ORIENTED_EDGE('',*,*,#17230,.T.) ;
#23978 = ORIENTED_EDGE('',*,*,#17227,.T.) ;
#23979 = ORIENTED_EDGE('',*,*,#17254,.T.) ;
#23980 = ORIENTED_EDGE('',*,*,#17255,.F.) ;
#23981 = ORIENTED_EDGE('',*,*,#17252,.T.) ;
#23982 = ORIENTED_EDGE('',*,*,#17256,.F.) ;
#23983 = ORIENTED_EDGE('',*,*,#17257,.F.) ;
#23984 = ORIENTED_EDGE('',*,*,#17258,.F.) ;
#23985 = ORIENTED_EDGE('',*,*,#17259,.T.) ;
#23986 = ORIENTED_EDGE('',*,*,#17260,.F.) ;
#23987 = ORIENTED_EDGE('',*,*,#17259,.F.) ;
#23988 = ORIENTED_EDGE('',*,*,#17260,.T.) ;
#23989 = ORIENTED_EDGE('',*,*,#17258,.T.) ;
#23990 = ORIENTED_EDGE('',*,*,#17261,.F.) ;
#23991 = ORIENTED_EDGE('',*,*,#17262,.F.) ;
#23992 = ORIENTED_EDGE('',*,*,#17263,.T.) ;
#23993 = ORIENTED_EDGE('',*,*,#17257,.T.) ;
#23994 = ORIENTED_EDGE('',*,*,#17264,.T.) ;
#23995 = ORIENTED_EDGE('',*,*,#17265,.T.) ;
#23996 = ORIENTED_EDGE('',*,*,#17266,.F.) ;
#23997 = ORIENTED_EDGE('',*,*,#17267,.T.) ;
#23998 = ORIENTED_EDGE('',*,*,#17268,.T.) ;
#23999 = ORIENTED_EDGE('',*,*,#17269,.T.) ;
#24000 = ORIENTED_EDGE('',*,*,#17268,.F.) ;
#24001 = ORIENTED_EDGE('',*,*,#17267,.F.) ;
#24002 = ORIENTED_EDGE('',*,*,#17270,.F.) ;
#24003 = ORIENTED_EDGE('',*,*,#17269,.F.) ;
#24004 = ORIENTED_EDGE('',*,*,#17271,.F.) ;
#24005 = ORIENTED_EDGE('',*,*,#17272,.T.) ;
#24006 = ORIENTED_EDGE('',*,*,#17270,.T.) ;
#24007 = ORIENTED_EDGE('',*,*,#17272,.F.) ;
#24008 = ORIENTED_EDGE('',*,*,#17273,.F.) ;
#24009 = ORIENTED_EDGE('',*,*,#17274,.T.) ;
#24010 = ORIENTED_EDGE('',*,*,#17275,.F.) ;
#24011 = ORIENTED_EDGE('',*,*,#17274,.F.) ;
#24012 = ORIENTED_EDGE('',*,*,#17276,.T.) ;
#24013 = ORIENTED_EDGE('',*,*,#17277,.T.) ;
#24014 = ORIENTED_EDGE('',*,*,#17278,.T.) ;
#24015 = ORIENTED_EDGE('',*,*,#17279,.T.) ;
#24016 = ORIENTED_EDGE('',*,*,#17280,.F.) ;
#24017 = ORIENTED_EDGE('',*,*,#17281,.F.) ;
#24018 = ORIENTED_EDGE('',*,*,#17282,.F.) ;
#24019 = ORIENTED_EDGE('',*,*,#17283,.F.) ;
#24020 = ORIENTED_EDGE('',*,*,#17284,.T.) ;
#24021 = ORIENTED_EDGE('',*,*,#17285,.T.) ;
#24022 = ORIENTED_EDGE('',*,*,#17286,.T.) ;
#24023 = ORIENTED_EDGE('',*,*,#17287,.T.) ;
#24024 = ORIENTED_EDGE('',*,*,#17288,.F.) ;
#24025 = ORIENTED_EDGE('',*,*,#17265,.F.) ;
#24026 = ORIENTED_EDGE('',*,*,#17289,.F.) ;
#24027 = ORIENTED_EDGE('',*,*,#17290,.F.) ;
#24028 = ORIENTED_EDGE('',*,*,#17291,.T.) ;
#24029 = ORIENTED_EDGE('',*,*,#17277,.F.) ;
#24030 = ORIENTED_EDGE('',*,*,#17292,.F.) ;
#24031 = ORIENTED_EDGE('',*,*,#17287,.F.) ;
#24032 = ORIENTED_EDGE('',*,*,#17273,.T.) ;
#24033 = ORIENTED_EDGE('',*,*,#17293,.T.) ;
#24034 = ORIENTED_EDGE('',*,*,#17278,.F.) ;
#24035 = ORIENTED_EDGE('',*,*,#17291,.F.) ;
#24036 = ORIENTED_EDGE('',*,*,#17286,.F.) ;
#24037 = ORIENTED_EDGE('',*,*,#17294,.T.) ;
#24038 = ORIENTED_EDGE('',*,*,#17279,.F.) ;
#24039 = ORIENTED_EDGE('',*,*,#17293,.F.) ;
#24040 = ORIENTED_EDGE('',*,*,#17285,.F.) ;
#24041 = ORIENTED_EDGE('',*,*,#17275,.T.) ;
#24042 = ORIENTED_EDGE('',*,*,#17292,.T.) ;
#24043 = ORIENTED_EDGE('',*,*,#17276,.F.) ;
#24044 = ORIENTED_EDGE('',*,*,#17294,.F.) ;
#24045 = ORIENTED_EDGE('',*,*,#17284,.F.) ;
#24046 = ORIENTED_EDGE('',*,*,#17289,.T.) ;
#24047 = ORIENTED_EDGE('',*,*,#17264,.F.) ;
#24048 = ORIENTED_EDGE('',*,*,#17263,.F.) ;
#24049 = ORIENTED_EDGE('',*,*,#17295,.F.) ;
#24050 = ORIENTED_EDGE('',*,*,#17296,.T.) ;
#24051 = ORIENTED_EDGE('',*,*,#17288,.T.) ;
#24052 = ORIENTED_EDGE('',*,*,#17297,.F.) ;
#24053 = ORIENTED_EDGE('',*,*,#17298,.F.) ;
#24054 = ORIENTED_EDGE('',*,*,#17261,.T.) ;
#24055 = ORIENTED_EDGE('',*,*,#17266,.T.) ;
#24056 = ORIENTED_EDGE('',*,*,#17298,.T.) ;
#24057 = ORIENTED_EDGE('',*,*,#17299,.T.) ;
#24058 = ORIENTED_EDGE('',*,*,#17295,.T.) ;
#24059 = ORIENTED_EDGE('',*,*,#17262,.T.) ;
#24060 = ORIENTED_EDGE('',*,*,#17290,.T.) ;
#24061 = ORIENTED_EDGE('',*,*,#17296,.F.) ;
#24062 = ORIENTED_EDGE('',*,*,#17299,.F.) ;
#24063 = ORIENTED_EDGE('',*,*,#17297,.T.) ;
#24064 = ORIENTED_EDGE('',*,*,#17282,.T.) ;
#24065 = ORIENTED_EDGE('',*,*,#17300,.T.) ;
#24066 = ORIENTED_EDGE('',*,*,#17301,.F.) ;
#24067 = ORIENTED_EDGE('',*,*,#17302,.F.) ;
#24068 = ORIENTED_EDGE('',*,*,#17281,.T.) ;
#24069 = ORIENTED_EDGE('',*,*,#17303,.T.) ;
#24070 = ORIENTED_EDGE('',*,*,#17304,.F.) ;
#24071 = ORIENTED_EDGE('',*,*,#17300,.F.) ;
#24072 = ORIENTED_EDGE('',*,*,#17280,.T.) ;
#24073 = ORIENTED_EDGE('',*,*,#17305,.T.) ;
#24074 = ORIENTED_EDGE('',*,*,#17306,.F.) ;
#24075 = ORIENTED_EDGE('',*,*,#17303,.F.) ;
#24076 = ORIENTED_EDGE('',*,*,#17283,.T.) ;
#24077 = ORIENTED_EDGE('',*,*,#17302,.T.) ;
#24078 = ORIENTED_EDGE('',*,*,#17307,.F.) ;
#24079 = ORIENTED_EDGE('',*,*,#17305,.F.) ;
#24080 = ORIENTED_EDGE('',*,*,#17307,.T.) ;
#24081 = ORIENTED_EDGE('',*,*,#17301,.T.) ;
#24082 = ORIENTED_EDGE('',*,*,#17304,.T.) ;
#24083 = ORIENTED_EDGE('',*,*,#17306,.T.) ;
#24084 = ORIENTED_EDGE('',*,*,#17271,.T.) ;
#24085 = ORIENTED_EDGE('',*,*,#17308,.F.) ;
#24086 = ORIENTED_EDGE('',*,*,#17309,.T.) ;
#24087 = ORIENTED_EDGE('',*,*,#17310,.F.) ;
#24088 = ORIENTED_EDGE('',*,*,#17309,.F.) ;
#24089 = ORIENTED_EDGE('',*,*,#17310,.T.) ;
#24090 = ORIENTED_EDGE('',*,*,#17308,.T.) ;
#24091 = ORIENTED_EDGE('',*,*,#17311,.F.) ;
#24092 = ORIENTED_EDGE('',*,*,#17311,.T.) ;
#24093 = ORIENTED_EDGE('',*,*,#17312,.T.) ;
#24094 = ORIENTED_EDGE('',*,*,#17313,.T.) ;
#24095 = ORIENTED_EDGE('',*,*,#17312,.F.) ;
#24096 = ORIENTED_EDGE('',*,*,#17314,.T.) ;
#24097 = ORIENTED_EDGE('',*,*,#17315,.F.) ;
#24098 = ORIENTED_EDGE('',*,*,#17314,.F.) ;
#24099 = ORIENTED_EDGE('',*,*,#17315,.T.) ;
#24100 = ORIENTED_EDGE('',*,*,#17316,.F.) ;
#24101 = ORIENTED_EDGE('',*,*,#17317,.T.) ;
#24102 = ORIENTED_EDGE('',*,*,#17313,.F.) ;
#24103 = ORIENTED_EDGE('',*,*,#17317,.F.) ;
#24104 = ORIENTED_EDGE('',*,*,#17316,.T.) ;
#24105 = ORIENTED_EDGE('',*,*,#17318,.T.) ;
#24106 = ORIENTED_EDGE('',*,*,#17318,.F.) ;
#24107 = ORIENTED_EDGE('',*,*,#17319,.T.) ;
#24108 = ORIENTED_EDGE('',*,*,#17319,.F.) ;
#24109 = ORIENTED_EDGE('',*,*,#17320,.T.) ;
#24110 = ORIENTED_EDGE('',*,*,#17320,.F.) ;
#24111 = ORIENTED_EDGE('',*,*,#17321,.F.) ;
#24112 = ORIENTED_EDGE('',*,*,#17322,.T.) ;
#24113 = ORIENTED_EDGE('',*,*,#17323,.T.) ;
#24114 = ORIENTED_EDGE('',*,*,#17321,.T.) ;
#24115 = ORIENTED_EDGE('',*,*,#17323,.F.) ;
#24116 = ORIENTED_EDGE('',*,*,#17322,.F.) ;
#24117 = ORIENTED_EDGE('',*,*,#17324,.T.) ;
#24118 = ORIENTED_EDGE('',*,*,#17325,.T.) ;
#24119 = ORIENTED_EDGE('',*,*,#17326,.T.) ;
#24120 = ORIENTED_EDGE('',*,*,#17327,.T.) ;
#24121 = ORIENTED_EDGE('',*,*,#17328,.T.) ;
#24122 = ORIENTED_EDGE('',*,*,#17329,.T.) ;
#24123 = ORIENTED_EDGE('',*,*,#17330,.T.) ;
#24124 = ORIENTED_EDGE('',*,*,#17331,.F.) ;
#24125 = ORIENTED_EDGE('',*,*,#17332,.T.) ;
#24126 = ORIENTED_EDGE('',*,*,#17333,.T.) ;
#24127 = ORIENTED_EDGE('',*,*,#17334,.T.) ;
#24128 = ORIENTED_EDGE('',*,*,#17335,.F.) ;
#24129 = ORIENTED_EDGE('',*,*,#17336,.T.) ;
#24130 = ORIENTED_EDGE('',*,*,#17337,.T.) ;
#24131 = ORIENTED_EDGE('',*,*,#17331,.T.) ;
#24132 = ORIENTED_EDGE('',*,*,#17338,.T.) ;
#24133 = ORIENTED_EDGE('',*,*,#17336,.F.) ;
#24134 = ORIENTED_EDGE('',*,*,#17339,.T.) ;
#24135 = ORIENTED_EDGE('',*,*,#17340,.T.) ;
#24136 = ORIENTED_EDGE('',*,*,#17341,.F.) ;
#24137 = ORIENTED_EDGE('',*,*,#17340,.F.) ;
#24138 = ORIENTED_EDGE('',*,*,#17342,.F.) ;
#24139 = ORIENTED_EDGE('',*,*,#17343,.T.) ;
#24140 = ORIENTED_EDGE('',*,*,#17344,.F.) ;
#24141 = ORIENTED_EDGE('',*,*,#17345,.F.) ;
#24142 = ORIENTED_EDGE('',*,*,#17346,.F.) ;
#24143 = ORIENTED_EDGE('',*,*,#17343,.F.) ;
#24144 = ORIENTED_EDGE('',*,*,#17342,.T.) ;
#24145 = ORIENTED_EDGE('',*,*,#17341,.T.) ;
#24146 = ORIENTED_EDGE('',*,*,#17344,.T.) ;
#24147 = ORIENTED_EDGE('',*,*,#17346,.T.) ;
#24148 = ORIENTED_EDGE('',*,*,#17347,.F.) ;
#24149 = ORIENTED_EDGE('',*,*,#17348,.T.) ;
#24150 = ORIENTED_EDGE('',*,*,#17349,.F.) ;
#24151 = ORIENTED_EDGE('',*,*,#17324,.F.) ;
#24152 = ORIENTED_EDGE('',*,*,#17350,.F.) ;
#24153 = ORIENTED_EDGE('',*,*,#17348,.F.) ;
#24154 = ORIENTED_EDGE('',*,*,#17351,.F.) ;
#24155 = ORIENTED_EDGE('',*,*,#17349,.T.) ;
#24156 = ORIENTED_EDGE('',*,*,#17352,.T.) ;
#24157 = ORIENTED_EDGE('',*,*,#17326,.F.) ;
#24158 = ORIENTED_EDGE('',*,*,#17353,.F.) ;
#24159 = ORIENTED_EDGE('',*,*,#17327,.F.) ;
#24160 = ORIENTED_EDGE('',*,*,#17352,.F.) ;
#24161 = ORIENTED_EDGE('',*,*,#17350,.T.) ;
#24162 = ORIENTED_EDGE('',*,*,#17325,.F.) ;
#24163 = ORIENTED_EDGE('',*,*,#17353,.T.) ;
#24164 = ORIENTED_EDGE('',*,*,#17329,.F.) ;
#24165 = ORIENTED_EDGE('',*,*,#17354,.T.) ;
#24166 = ORIENTED_EDGE('',*,*,#17355,.F.) ;
#24167 = ORIENTED_EDGE('',*,*,#17356,.F.) ;
#24168 = ORIENTED_EDGE('',*,*,#17354,.F.) ;
#24169 = ORIENTED_EDGE('',*,*,#17328,.F.) ;
#24170 = ORIENTED_EDGE('',*,*,#17356,.T.) ;
#24171 = ORIENTED_EDGE('',*,*,#17357,.F.) ;
#24172 = ORIENTED_EDGE('',*,*,#17358,.T.) ;
#24173 = ORIENTED_EDGE('',*,*,#17332,.F.) ;
#24174 = ORIENTED_EDGE('',*,*,#17359,.F.) ;
#24175 = ORIENTED_EDGE('',*,*,#17360,.F.) ;
#24176 = ORIENTED_EDGE('',*,*,#17333,.F.) ;
#24177 = ORIENTED_EDGE('',*,*,#17358,.F.) ;
#24178 = ORIENTED_EDGE('',*,*,#17338,.F.) ;
#24179 = ORIENTED_EDGE('',*,*,#17330,.F.) ;
#24180 = ORIENTED_EDGE('',*,*,#17337,.F.) ;
#24181 = ORIENTED_EDGE('',*,*,#17360,.T.) ;
#24182 = ORIENTED_EDGE('',*,*,#17361,.T.) ;
#24183 = ORIENTED_EDGE('',*,*,#17362,.F.) ;
#24184 = ORIENTED_EDGE('',*,*,#17361,.F.) ;
#24185 = ORIENTED_EDGE('',*,*,#17359,.T.) ;
#24186 = ORIENTED_EDGE('',*,*,#17334,.F.) ;
#24187 = ORIENTED_EDGE('',*,*,#17362,.T.) ;
#24188 = ORIENTED_EDGE('',*,*,#17335,.T.) ;
#24189 = ORIENTED_EDGE('',*,*,#17357,.T.) ;
#24190 = ORIENTED_EDGE('',*,*,#17355,.T.) ;
#24191 = ORIENTED_EDGE('',*,*,#17351,.T.) ;
#24192 = ORIENTED_EDGE('',*,*,#17347,.T.) ;
#24193 = ORIENTED_EDGE('',*,*,#17345,.T.) ;
#24194 = ORIENTED_EDGE('',*,*,#17339,.F.) ;
#24195 = ORIENTED_EDGE('',*,*,#17363,.F.) ;
#24196 = ORIENTED_EDGE('',*,*,#17364,.F.) ;
#24197 = ORIENTED_EDGE('',*,*,#17365,.T.) ;
#24198 = ORIENTED_EDGE('',*,*,#17366,.F.) ;
#24199 = ORIENTED_EDGE('',*,*,#17364,.T.) ;
#24200 = ORIENTED_EDGE('',*,*,#17367,.T.) ;
#24201 = ORIENTED_EDGE('',*,*,#17363,.T.) ;
#24202 = ORIENTED_EDGE('',*,*,#17367,.F.) ;
#24203 = ORIENTED_EDGE('',*,*,#17366,.T.) ;
#24204 = ORIENTED_EDGE('',*,*,#17368,.F.) ;
#24205 = ORIENTED_EDGE('',*,*,#17368,.T.) ;
#24206 = ORIENTED_EDGE('',*,*,#17365,.F.) ;
#24207 = ORIENTED_EDGE('',*,*,#17369,.T.) ;
#24208 = ORIENTED_EDGE('',*,*,#17369,.F.) ;
#24209 = ORIENTED_EDGE('',*,*,#17370,.T.) ;
#24210 = ORIENTED_EDGE('',*,*,#17371,.F.) ;
#24211 = ORIENTED_EDGE('',*,*,#17372,.F.) ;
#24212 = ORIENTED_EDGE('',*,*,#17373,.T.) ;
#24213 = ORIENTED_EDGE('',*,*,#17370,.F.) ;
#24214 = ORIENTED_EDGE('',*,*,#17374,.F.) ;
#24215 = ORIENTED_EDGE('',*,*,#17375,.F.) ;
#24216 = ORIENTED_EDGE('',*,*,#17372,.T.) ;
#24217 = ORIENTED_EDGE('',*,*,#17376,.T.) ;
#24218 = ORIENTED_EDGE('',*,*,#17377,.T.) ;
#24219 = ORIENTED_EDGE('',*,*,#17374,.T.) ;
#24220 = ORIENTED_EDGE('',*,*,#17378,.T.) ;
#24221 = ORIENTED_EDGE('',*,*,#17376,.F.) ;
#24222 = ORIENTED_EDGE('',*,*,#17371,.T.) ;
#24223 = ORIENTED_EDGE('',*,*,#17373,.F.) ;
#24224 = ORIENTED_EDGE('',*,*,#17375,.T.) ;
#24225 = ORIENTED_EDGE('',*,*,#17377,.F.) ;
#24226 = ORIENTED_EDGE('',*,*,#17378,.F.) ;
#24227 = ORIENTED_EDGE('',*,*,#17379,.F.) ;
#24228 = ORIENTED_EDGE('',*,*,#17380,.T.) ;
#24229 = ORIENTED_EDGE('',*,*,#17381,.F.) ;
#24230 = ORIENTED_EDGE('',*,*,#17382,.F.) ;
#24231 = ORIENTED_EDGE('',*,*,#17382,.T.) ;
#24232 = ORIENTED_EDGE('',*,*,#17383,.T.) ;
#24233 = ORIENTED_EDGE('',*,*,#17384,.F.) ;
#24234 = ORIENTED_EDGE('',*,*,#17385,.T.) ;
#24235 = ORIENTED_EDGE('',*,*,#17386,.T.) ;
#24236 = ORIENTED_EDGE('',*,*,#17381,.T.) ;
#24237 = ORIENTED_EDGE('',*,*,#17387,.T.) ;
#24238 = ORIENTED_EDGE('',*,*,#17379,.T.) ;
#24239 = ORIENTED_EDGE('',*,*,#17386,.F.) ;
#24240 = ORIENTED_EDGE('',*,*,#17388,.T.) ;
#24241 = ORIENTED_EDGE('',*,*,#17383,.F.) ;
#24242 = ORIENTED_EDGE('',*,*,#17387,.F.) ;
#24243 = ORIENTED_EDGE('',*,*,#17380,.F.) ;
#24244 = ORIENTED_EDGE('',*,*,#17385,.F.) ;
#24245 = ORIENTED_EDGE('',*,*,#17384,.T.) ;
#24246 = ORIENTED_EDGE('',*,*,#17388,.F.) ;
#24247 = ORIENTED_EDGE('',*,*,#17389,.T.) ;
#24248 = ORIENTED_EDGE('',*,*,#17389,.F.) ;
#24249 = ORIENTED_EDGE('',*,*,#17390,.F.) ;
#24250 = ORIENTED_EDGE('',*,*,#17391,.F.) ;
#24251 = ORIENTED_EDGE('',*,*,#17392,.T.) ;
#24252 = ORIENTED_EDGE('',*,*,#17393,.F.) ;
#24253 = ORIENTED_EDGE('',*,*,#17392,.F.) ;
#24254 = ORIENTED_EDGE('',*,*,#17394,.F.) ;
#24255 = ORIENTED_EDGE('',*,*,#17395,.F.) ;
#24256 = ORIENTED_EDGE('',*,*,#17396,.F.) ;
#24257 = ORIENTED_EDGE('',*,*,#17393,.T.) ;
#24258 = ORIENTED_EDGE('',*,*,#17397,.F.) ;
#24259 = ORIENTED_EDGE('',*,*,#17396,.T.) ;
#24260 = ORIENTED_EDGE('',*,*,#17398,.F.) ;
#24261 = ORIENTED_EDGE('',*,*,#17399,.F.) ;
#24262 = ORIENTED_EDGE('',*,*,#17399,.T.) ;
#24263 = ORIENTED_EDGE('',*,*,#17400,.T.) ;
#24264 = ORIENTED_EDGE('',*,*,#17401,.T.) ;
#24265 = ORIENTED_EDGE('',*,*,#17397,.T.) ;
#24266 = ORIENTED_EDGE('',*,*,#17401,.F.) ;
#24267 = ORIENTED_EDGE('',*,*,#17402,.T.) ;
#24268 = ORIENTED_EDGE('',*,*,#17403,.F.) ;
#24269 = ORIENTED_EDGE('',*,*,#17402,.F.) ;
#24270 = ORIENTED_EDGE('',*,*,#17400,.F.) ;
#24271 = ORIENTED_EDGE('',*,*,#17398,.T.) ;
#24272 = ORIENTED_EDGE('',*,*,#17395,.T.) ;
#24273 = ORIENTED_EDGE('',*,*,#17394,.T.) ;
#24274 = ORIENTED_EDGE('',*,*,#17391,.T.) ;
#24275 = ORIENTED_EDGE('',*,*,#17390,.T.) ;
#24276 = ORIENTED_EDGE('',*,*,#17403,.T.) ;
#24277 = ORIENTED_EDGE('',*,*,#17404,.F.) ;
#24278 = ORIENTED_EDGE('',*,*,#17405,.T.) ;
#24279 = ORIENTED_EDGE('',*,*,#17406,.F.) ;
#24280 = ORIENTED_EDGE('',*,*,#17405,.F.) ;
#24281 = ORIENTED_EDGE('',*,*,#17406,.T.) ;
#24282 = ORIENTED_EDGE('',*,*,#17404,.T.) ;
#24283 = ORIENTED_EDGE('',*,*,#17407,.F.) ;
#24284 = ORIENTED_EDGE('',*,*,#17408,.T.) ;
#24285 = ORIENTED_EDGE('',*,*,#17409,.F.) ;
#24286 = ORIENTED_EDGE('',*,*,#17408,.F.) ;
#24287 = ORIENTED_EDGE('',*,*,#17409,.T.) ;
#24288 = ORIENTED_EDGE('',*,*,#17407,.T.) ;
#24289 = ORIENTED_EDGE('',*,*,#17410,.F.) ;
#24290 = ORIENTED_EDGE('',*,*,#17411,.T.) ;
#24291 = ORIENTED_EDGE('',*,*,#17412,.F.) ;
#24292 = ORIENTED_EDGE('',*,*,#17411,.F.) ;
#24293 = ORIENTED_EDGE('',*,*,#17412,.T.) ;
#24294 = ORIENTED_EDGE('',*,*,#17410,.T.) ;
#24295 = ORIENTED_EDGE('',*,*,#17413,.F.) ;
#24296 = ORIENTED_EDGE('',*,*,#17414,.T.) ;
#24297 = ORIENTED_EDGE('',*,*,#17415,.F.) ;
#24298 = ORIENTED_EDGE('',*,*,#17414,.F.) ;
#24299 = ORIENTED_EDGE('',*,*,#17416,.F.) ;
#24300 = ORIENTED_EDGE('',*,*,#17417,.F.) ;
#24301 = ORIENTED_EDGE('',*,*,#17418,.F.) ;
#24302 = ORIENTED_EDGE('',*,*,#17419,.T.) ;
#24303 = ORIENTED_EDGE('',*,*,#17420,.F.) ;
#24304 = ORIENTED_EDGE('',*,*,#17419,.F.) ;
#24305 = ORIENTED_EDGE('',*,*,#17415,.T.) ;
#24306 = ORIENTED_EDGE('',*,*,#17418,.T.) ;
#24307 = ORIENTED_EDGE('',*,*,#17413,.T.) ;
#24308 = ORIENTED_EDGE('',*,*,#17420,.T.) ;
#24309 = ORIENTED_EDGE('',*,*,#17421,.F.) ;
#24310 = ORIENTED_EDGE('',*,*,#17422,.T.) ;
#24311 = ORIENTED_EDGE('',*,*,#17417,.T.) ;
#24312 = ORIENTED_EDGE('',*,*,#17416,.T.) ;
#24313 = ORIENTED_EDGE('',*,*,#17422,.F.) ;
#24314 = ORIENTED_EDGE('',*,*,#17421,.T.) ;
#24315 = ORIENTED_EDGE('',*,*,#17423,.F.) ;
#24316 = ORIENTED_EDGE('',*,*,#17424,.T.) ;
#24317 = ORIENTED_EDGE('',*,*,#17425,.F.) ;
#24318 = ORIENTED_EDGE('',*,*,#17424,.F.) ;
#24319 = ORIENTED_EDGE('',*,*,#17426,.F.) ;
#24320 = ORIENTED_EDGE('',*,*,#17427,.T.) ;
#24321 = ORIENTED_EDGE('',*,*,#17428,.F.) ;
#24322 = ORIENTED_EDGE('',*,*,#17427,.F.) ;
#24323 = ORIENTED_EDGE('',*,*,#17428,.T.) ;
#24324 = ORIENTED_EDGE('',*,*,#17423,.T.) ;
#24325 = ORIENTED_EDGE('',*,*,#17426,.T.) ;
#24326 = ORIENTED_EDGE('',*,*,#17425,.T.) ;
#24327 = ORIENTED_EDGE('',*,*,#17429,.F.) ;
#24328 = ORIENTED_EDGE('',*,*,#17430,.F.) ;
#24329 = ORIENTED_EDGE('',*,*,#17431,.F.) ;
#24330 = ORIENTED_EDGE('',*,*,#17432,.F.) ;
#24331 = ORIENTED_EDGE('',*,*,#17433,.F.) ;
#24332 = ORIENTED_EDGE('',*,*,#17434,.T.) ;
#24333 = ORIENTED_EDGE('',*,*,#17435,.F.) ;
#24334 = ORIENTED_EDGE('',*,*,#17434,.F.) ;
#24335 = ORIENTED_EDGE('',*,*,#17436,.F.) ;
#24336 = ORIENTED_EDGE('',*,*,#17437,.T.) ;
#24337 = ORIENTED_EDGE('',*,*,#17438,.F.) ;
#24338 = ORIENTED_EDGE('',*,*,#17437,.F.) ;
#24339 = ORIENTED_EDGE('',*,*,#17438,.T.) ;
#24340 = ORIENTED_EDGE('',*,*,#17439,.F.) ;
#24341 = ORIENTED_EDGE('',*,*,#17433,.T.) ;
#24342 = ORIENTED_EDGE('',*,*,#17440,.F.) ;
#24343 = ORIENTED_EDGE('',*,*,#17441,.F.) ;
#24344 = ORIENTED_EDGE('',*,*,#17442,.F.) ;
#24345 = ORIENTED_EDGE('',*,*,#17443,.F.) ;
#24346 = ORIENTED_EDGE('',*,*,#17444,.F.) ;
#24347 = ORIENTED_EDGE('',*,*,#17436,.T.) ;
#24348 = ORIENTED_EDGE('',*,*,#17435,.T.) ;
#24349 = ORIENTED_EDGE('',*,*,#17429,.T.) ;
#24350 = ORIENTED_EDGE('',*,*,#17439,.T.) ;
#24351 = ORIENTED_EDGE('',*,*,#17445,.T.) ;
#24352 = ORIENTED_EDGE('',*,*,#17443,.T.) ;
#24353 = ORIENTED_EDGE('',*,*,#17446,.T.) ;
#24354 = ORIENTED_EDGE('',*,*,#17447,.T.) ;
#24355 = ORIENTED_EDGE('',*,*,#17441,.T.) ;
#24356 = ORIENTED_EDGE('',*,*,#17448,.T.) ;
#24357 = ORIENTED_EDGE('',*,*,#17449,.T.) ;
#24358 = ORIENTED_EDGE('',*,*,#17450,.T.) ;
#24359 = ORIENTED_EDGE('',*,*,#17451,.T.) ;
#24360 = ORIENTED_EDGE('',*,*,#17452,.T.) ;
#24361 = ORIENTED_EDGE('',*,*,#17453,.T.) ;
#24362 = ORIENTED_EDGE('',*,*,#17454,.T.) ;
#24363 = ORIENTED_EDGE('',*,*,#17455,.T.) ;
#24364 = ORIENTED_EDGE('',*,*,#17456,.T.) ;
#24365 = ORIENTED_EDGE('',*,*,#17456,.F.) ;
#24366 = ORIENTED_EDGE('',*,*,#17457,.T.) ;
#24367 = ORIENTED_EDGE('',*,*,#17458,.T.) ;
#24368 = ORIENTED_EDGE('',*,*,#17459,.T.) ;
#24369 = ORIENTED_EDGE('',*,*,#17460,.T.) ;
#24370 = ORIENTED_EDGE('',*,*,#17461,.T.) ;
#24371 = ORIENTED_EDGE('',*,*,#17462,.T.) ;
#24372 = ORIENTED_EDGE('',*,*,#17463,.T.) ;
#24373 = ORIENTED_EDGE('',*,*,#17464,.T.) ;
#24374 = ORIENTED_EDGE('',*,*,#17465,.T.) ;
#24375 = ORIENTED_EDGE('',*,*,#17466,.T.) ;
#24376 = ORIENTED_EDGE('',*,*,#17467,.T.) ;
#24377 = ORIENTED_EDGE('',*,*,#17468,.T.) ;
#24378 = ORIENTED_EDGE('',*,*,#17469,.T.) ;
#24379 = ORIENTED_EDGE('',*,*,#17470,.F.) ;
#24380 = ORIENTED_EDGE('',*,*,#17470,.T.) ;
#24381 = ORIENTED_EDGE('',*,*,#17471,.T.) ;
#24382 = ORIENTED_EDGE('',*,*,#17472,.T.) ;
#24383 = ORIENTED_EDGE('',*,*,#17473,.T.) ;
#24384 = ORIENTED_EDGE('',*,*,#17474,.T.) ;
#24385 = ORIENTED_EDGE('',*,*,#17475,.T.) ;
#24386 = ORIENTED_EDGE('',*,*,#17476,.T.) ;
#24387 = ORIENTED_EDGE('',*,*,#17477,.T.) ;
#24388 = ORIENTED_EDGE('',*,*,#17478,.T.) ;
#24389 = ORIENTED_EDGE('',*,*,#17479,.T.) ;
#24390 = ORIENTED_EDGE('',*,*,#17480,.T.) ;
#24391 = ORIENTED_EDGE('',*,*,#17481,.T.) ;
#24392 = ORIENTED_EDGE('',*,*,#17482,.T.) ;
#24393 = ORIENTED_EDGE('',*,*,#17483,.T.) ;
#24394 = ORIENTED_EDGE('',*,*,#17484,.T.) ;
#24395 = ORIENTED_EDGE('',*,*,#17484,.F.) ;
#24396 = ORIENTED_EDGE('',*,*,#17485,.T.) ;
#24397 = ORIENTED_EDGE('',*,*,#17486,.T.) ;
#24398 = ORIENTED_EDGE('',*,*,#17487,.T.) ;
#24399 = ORIENTED_EDGE('',*,*,#17488,.T.) ;
#24400 = ORIENTED_EDGE('',*,*,#17489,.T.) ;
#24401 = ORIENTED_EDGE('',*,*,#17490,.T.) ;
#24402 = ORIENTED_EDGE('',*,*,#17491,.T.) ;
#24403 = ORIENTED_EDGE('',*,*,#17492,.T.) ;
#24404 = ORIENTED_EDGE('',*,*,#17493,.T.) ;
#24405 = ORIENTED_EDGE('',*,*,#17494,.T.) ;
#24406 = ORIENTED_EDGE('',*,*,#17495,.T.) ;
#24407 = ORIENTED_EDGE('',*,*,#17496,.T.) ;
#24408 = ORIENTED_EDGE('',*,*,#17497,.T.) ;
#24409 = ORIENTED_EDGE('',*,*,#17498,.F.) ;
#24410 = ORIENTED_EDGE('',*,*,#17498,.T.) ;
#24411 = ORIENTED_EDGE('',*,*,#17499,.T.) ;
#24412 = ORIENTED_EDGE('',*,*,#17500,.T.) ;
#24413 = ORIENTED_EDGE('',*,*,#17501,.T.) ;
#24414 = ORIENTED_EDGE('',*,*,#17502,.T.) ;
#24415 = ORIENTED_EDGE('',*,*,#17503,.T.) ;
#24416 = ORIENTED_EDGE('',*,*,#17504,.T.) ;
#24417 = ORIENTED_EDGE('',*,*,#17505,.T.) ;
#24418 = ORIENTED_EDGE('',*,*,#17506,.T.) ;
#24419 = ORIENTED_EDGE('',*,*,#17507,.T.) ;
#24420 = ORIENTED_EDGE('',*,*,#17508,.T.) ;
#24421 = ORIENTED_EDGE('',*,*,#17509,.T.) ;
#24422 = ORIENTED_EDGE('',*,*,#17510,.T.) ;
#24423 = ORIENTED_EDGE('',*,*,#17511,.T.) ;
#24424 = ORIENTED_EDGE('',*,*,#17512,.T.) ;
#24425 = ORIENTED_EDGE('',*,*,#17512,.F.) ;
#24426 = ORIENTED_EDGE('',*,*,#17513,.T.) ;
#24427 = ORIENTED_EDGE('',*,*,#17514,.T.) ;
#24428 = ORIENTED_EDGE('',*,*,#17515,.T.) ;
#24429 = ORIENTED_EDGE('',*,*,#17516,.T.) ;
#24430 = ORIENTED_EDGE('',*,*,#17517,.T.) ;
#24431 = ORIENTED_EDGE('',*,*,#17518,.T.) ;
#24432 = ORIENTED_EDGE('',*,*,#17519,.T.) ;
#24433 = ORIENTED_EDGE('',*,*,#17520,.T.) ;
#24434 = ORIENTED_EDGE('',*,*,#17521,.T.) ;
#24435 = ORIENTED_EDGE('',*,*,#17522,.T.) ;
#24436 = ORIENTED_EDGE('',*,*,#17523,.T.) ;
#24437 = ORIENTED_EDGE('',*,*,#17524,.T.) ;
#24438 = ORIENTED_EDGE('',*,*,#17525,.T.) ;
#24439 = ORIENTED_EDGE('',*,*,#17526,.F.) ;
#24440 = ORIENTED_EDGE('',*,*,#17526,.T.) ;
#24441 = ORIENTED_EDGE('',*,*,#17527,.T.) ;
#24442 = ORIENTED_EDGE('',*,*,#17528,.T.) ;
#24443 = ORIENTED_EDGE('',*,*,#17529,.T.) ;
#24444 = ORIENTED_EDGE('',*,*,#17530,.T.) ;
#24445 = ORIENTED_EDGE('',*,*,#17531,.T.) ;
#24446 = ORIENTED_EDGE('',*,*,#17532,.T.) ;
#24447 = ORIENTED_EDGE('',*,*,#17533,.T.) ;
#24448 = ORIENTED_EDGE('',*,*,#17534,.T.) ;
#24449 = ORIENTED_EDGE('',*,*,#17535,.T.) ;
#24450 = ORIENTED_EDGE('',*,*,#17536,.T.) ;
#24451 = ORIENTED_EDGE('',*,*,#17537,.T.) ;
#24452 = ORIENTED_EDGE('',*,*,#17538,.T.) ;
#24453 = ORIENTED_EDGE('',*,*,#17539,.T.) ;
#24454 = ORIENTED_EDGE('',*,*,#17540,.T.) ;
#24455 = ORIENTED_EDGE('',*,*,#17540,.F.) ;
#24456 = ORIENTED_EDGE('',*,*,#17541,.T.) ;
#24457 = ORIENTED_EDGE('',*,*,#17542,.T.) ;
#24458 = ORIENTED_EDGE('',*,*,#17543,.T.) ;
#24459 = ORIENTED_EDGE('',*,*,#17544,.T.) ;
#24460 = ORIENTED_EDGE('',*,*,#17545,.T.) ;
#24461 = ORIENTED_EDGE('',*,*,#17546,.T.) ;
#24462 = ORIENTED_EDGE('',*,*,#17547,.T.) ;
#24463 = ORIENTED_EDGE('',*,*,#17548,.T.) ;
#24464 = ORIENTED_EDGE('',*,*,#17549,.T.) ;
#24465 = ORIENTED_EDGE('',*,*,#17550,.T.) ;
#24466 = ORIENTED_EDGE('',*,*,#17551,.T.) ;
#24467 = ORIENTED_EDGE('',*,*,#17552,.T.) ;
#24468 = ORIENTED_EDGE('',*,*,#17553,.T.) ;
#24469 = ORIENTED_EDGE('',*,*,#17554,.F.) ;
#24470 = ORIENTED_EDGE('',*,*,#17554,.T.) ;
#24471 = ORIENTED_EDGE('',*,*,#17555,.T.) ;
#24472 = ORIENTED_EDGE('',*,*,#17556,.T.) ;
#24473 = ORIENTED_EDGE('',*,*,#17557,.T.) ;
#24474 = ORIENTED_EDGE('',*,*,#17558,.T.) ;
#24475 = ORIENTED_EDGE('',*,*,#17559,.T.) ;
#24476 = ORIENTED_EDGE('',*,*,#17560,.T.) ;
#24477 = ORIENTED_EDGE('',*,*,#17561,.T.) ;
#24478 = ORIENTED_EDGE('',*,*,#17562,.T.) ;
#24479 = ORIENTED_EDGE('',*,*,#17563,.T.) ;
#24480 = ORIENTED_EDGE('',*,*,#17564,.T.) ;
#24481 = ORIENTED_EDGE('',*,*,#17565,.T.) ;
#24482 = ORIENTED_EDGE('',*,*,#17566,.T.) ;
#24483 = ORIENTED_EDGE('',*,*,#17567,.T.) ;
#24484 = ORIENTED_EDGE('',*,*,#17568,.T.) ;
#24485 = ORIENTED_EDGE('',*,*,#17568,.F.) ;
#24486 = ORIENTED_EDGE('',*,*,#17569,.T.) ;
#24487 = ORIENTED_EDGE('',*,*,#17570,.T.) ;
#24488 = ORIENTED_EDGE('',*,*,#17571,.T.) ;
#24489 = ORIENTED_EDGE('',*,*,#17572,.T.) ;
#24490 = ORIENTED_EDGE('',*,*,#17573,.T.) ;
#24491 = ORIENTED_EDGE('',*,*,#17574,.T.) ;
#24492 = ORIENTED_EDGE('',*,*,#17575,.T.) ;
#24493 = ORIENTED_EDGE('',*,*,#17576,.T.) ;
#24494 = ORIENTED_EDGE('',*,*,#17577,.T.) ;
#24495 = ORIENTED_EDGE('',*,*,#17578,.T.) ;
#24496 = ORIENTED_EDGE('',*,*,#17579,.T.) ;
#24497 = ORIENTED_EDGE('',*,*,#17580,.T.) ;
#24498 = ORIENTED_EDGE('',*,*,#17581,.T.) ;
#24499 = ORIENTED_EDGE('',*,*,#17582,.F.) ;
#24500 = ORIENTED_EDGE('',*,*,#17582,.T.) ;
#24501 = ORIENTED_EDGE('',*,*,#17583,.T.) ;
#24502 = ORIENTED_EDGE('',*,*,#17584,.T.) ;
#24503 = ORIENTED_EDGE('',*,*,#17585,.T.) ;
#24504 = ORIENTED_EDGE('',*,*,#17586,.T.) ;
#24505 = ORIENTED_EDGE('',*,*,#17587,.T.) ;
#24506 = ORIENTED_EDGE('',*,*,#17588,.T.) ;
#24507 = ORIENTED_EDGE('',*,*,#17589,.T.) ;
#24508 = ORIENTED_EDGE('',*,*,#17590,.T.) ;
#24509 = ORIENTED_EDGE('',*,*,#17591,.T.) ;
#24510 = ORIENTED_EDGE('',*,*,#17592,.T.) ;
#24511 = ORIENTED_EDGE('',*,*,#17593,.T.) ;
#24512 = ORIENTED_EDGE('',*,*,#17594,.T.) ;
#24513 = ORIENTED_EDGE('',*,*,#17595,.T.) ;
#24514 = ORIENTED_EDGE('',*,*,#17596,.T.) ;
#24515 = ORIENTED_EDGE('',*,*,#17596,.F.) ;
#24516 = ORIENTED_EDGE('',*,*,#17597,.T.) ;
#24517 = ORIENTED_EDGE('',*,*,#17598,.T.) ;
#24518 = ORIENTED_EDGE('',*,*,#17599,.T.) ;
#24519 = ORIENTED_EDGE('',*,*,#17600,.T.) ;
#24520 = ORIENTED_EDGE('',*,*,#17601,.T.) ;
#24521 = ORIENTED_EDGE('',*,*,#17602,.T.) ;
#24522 = ORIENTED_EDGE('',*,*,#17603,.T.) ;
#24523 = ORIENTED_EDGE('',*,*,#17604,.T.) ;
#24524 = ORIENTED_EDGE('',*,*,#17605,.T.) ;
#24525 = ORIENTED_EDGE('',*,*,#17606,.T.) ;
#24526 = ORIENTED_EDGE('',*,*,#17607,.T.) ;
#24527 = ORIENTED_EDGE('',*,*,#17608,.T.) ;
#24528 = ORIENTED_EDGE('',*,*,#17609,.T.) ;
#24529 = ORIENTED_EDGE('',*,*,#17610,.F.) ;
#24530 = ORIENTED_EDGE('',*,*,#17610,.T.) ;
#24531 = ORIENTED_EDGE('',*,*,#17611,.T.) ;
#24532 = ORIENTED_EDGE('',*,*,#17612,.T.) ;
#24533 = ORIENTED_EDGE('',*,*,#17613,.T.) ;
#24534 = ORIENTED_EDGE('',*,*,#17614,.T.) ;
#24535 = ORIENTED_EDGE('',*,*,#17615,.T.) ;
#24536 = ORIENTED_EDGE('',*,*,#17616,.T.) ;
#24537 = ORIENTED_EDGE('',*,*,#17617,.T.) ;
#24538 = ORIENTED_EDGE('',*,*,#17618,.T.) ;
#24539 = ORIENTED_EDGE('',*,*,#17619,.T.) ;
#24540 = ORIENTED_EDGE('',*,*,#17620,.T.) ;
#24541 = ORIENTED_EDGE('',*,*,#17621,.T.) ;
#24542 = ORIENTED_EDGE('',*,*,#17622,.T.) ;
#24543 = ORIENTED_EDGE('',*,*,#17623,.T.) ;
#24544 = ORIENTED_EDGE('',*,*,#17624,.T.) ;
#24545 = ORIENTED_EDGE('',*,*,#17624,.F.) ;
#24546 = ORIENTED_EDGE('',*,*,#17625,.T.) ;
#24547 = ORIENTED_EDGE('',*,*,#17626,.T.) ;
#24548 = ORIENTED_EDGE('',*,*,#17627,.T.) ;
#24549 = ORIENTED_EDGE('',*,*,#17628,.T.) ;
#24550 = ORIENTED_EDGE('',*,*,#17629,.T.) ;
#24551 = ORIENTED_EDGE('',*,*,#17630,.T.) ;
#24552 = ORIENTED_EDGE('',*,*,#17631,.T.) ;
#24553 = ORIENTED_EDGE('',*,*,#17632,.T.) ;
#24554 = ORIENTED_EDGE('',*,*,#17633,.T.) ;
#24555 = ORIENTED_EDGE('',*,*,#17634,.T.) ;
#24556 = ORIENTED_EDGE('',*,*,#17635,.T.) ;
#24557 = ORIENTED_EDGE('',*,*,#17636,.T.) ;
#24558 = ORIENTED_EDGE('',*,*,#17637,.T.) ;
#24559 = ORIENTED_EDGE('',*,*,#17638,.F.) ;
#24560 = ORIENTED_EDGE('',*,*,#17638,.T.) ;
#24561 = ORIENTED_EDGE('',*,*,#17639,.T.) ;
#24562 = ORIENTED_EDGE('',*,*,#17640,.T.) ;
#24563 = ORIENTED_EDGE('',*,*,#17641,.T.) ;
#24564 = ORIENTED_EDGE('',*,*,#17642,.T.) ;
#24565 = ORIENTED_EDGE('',*,*,#17643,.T.) ;
#24566 = ORIENTED_EDGE('',*,*,#17644,.T.) ;
#24567 = ORIENTED_EDGE('',*,*,#17645,.T.) ;
#24568 = ORIENTED_EDGE('',*,*,#17646,.T.) ;
#24569 = ORIENTED_EDGE('',*,*,#17647,.T.) ;
#24570 = ORIENTED_EDGE('',*,*,#17648,.T.) ;
#24571 = ORIENTED_EDGE('',*,*,#17649,.T.) ;
#24572 = ORIENTED_EDGE('',*,*,#17650,.T.) ;
#24573 = ORIENTED_EDGE('',*,*,#17651,.T.) ;
#24574 = ORIENTED_EDGE('',*,*,#17652,.T.) ;
#24575 = ORIENTED_EDGE('',*,*,#17652,.F.) ;
#24576 = ORIENTED_EDGE('',*,*,#17653,.T.) ;
#24577 = ORIENTED_EDGE('',*,*,#17654,.T.) ;
#24578 = ORIENTED_EDGE('',*,*,#17655,.T.) ;
#24579 = ORIENTED_EDGE('',*,*,#17656,.T.) ;
#24580 = ORIENTED_EDGE('',*,*,#17657,.T.) ;
#24581 = ORIENTED_EDGE('',*,*,#17658,.T.) ;
#24582 = ORIENTED_EDGE('',*,*,#17659,.T.) ;
#24583 = ORIENTED_EDGE('',*,*,#17660,.T.) ;
#24584 = ORIENTED_EDGE('',*,*,#17661,.T.) ;
#24585 = ORIENTED_EDGE('',*,*,#17662,.T.) ;
#24586 = ORIENTED_EDGE('',*,*,#17663,.T.) ;
#24587 = ORIENTED_EDGE('',*,*,#17664,.T.) ;
#24588 = ORIENTED_EDGE('',*,*,#17665,.T.) ;
#24589 = ORIENTED_EDGE('',*,*,#17666,.F.) ;
#24590 = ORIENTED_EDGE('',*,*,#17666,.T.) ;
#24591 = ORIENTED_EDGE('',*,*,#17667,.T.) ;
#24592 = ORIENTED_EDGE('',*,*,#17668,.T.) ;
#24593 = ORIENTED_EDGE('',*,*,#17669,.T.) ;
#24594 = ORIENTED_EDGE('',*,*,#17670,.T.) ;
#24595 = ORIENTED_EDGE('',*,*,#17671,.T.) ;
#24596 = ORIENTED_EDGE('',*,*,#17672,.T.) ;
#24597 = ORIENTED_EDGE('',*,*,#17673,.T.) ;
#24598 = ORIENTED_EDGE('',*,*,#17674,.T.) ;
#24599 = ORIENTED_EDGE('',*,*,#17675,.T.) ;
#24600 = ORIENTED_EDGE('',*,*,#17676,.T.) ;
#24601 = ORIENTED_EDGE('',*,*,#17677,.T.) ;
#24602 = ORIENTED_EDGE('',*,*,#17678,.T.) ;
#24603 = ORIENTED_EDGE('',*,*,#17679,.T.) ;
#24604 = ORIENTED_EDGE('',*,*,#17680,.T.) ;
#24605 = ORIENTED_EDGE('',*,*,#17680,.F.) ;
#24606 = ORIENTED_EDGE('',*,*,#17681,.T.) ;
#24607 = ORIENTED_EDGE('',*,*,#17682,.T.) ;
#24608 = ORIENTED_EDGE('',*,*,#17683,.T.) ;
#24609 = ORIENTED_EDGE('',*,*,#17684,.T.) ;
#24610 = ORIENTED_EDGE('',*,*,#17685,.T.) ;
#24611 = ORIENTED_EDGE('',*,*,#17686,.T.) ;
#24612 = ORIENTED_EDGE('',*,*,#17687,.T.) ;
#24613 = ORIENTED_EDGE('',*,*,#17688,.T.) ;
#24614 = ORIENTED_EDGE('',*,*,#17689,.T.) ;
#24615 = ORIENTED_EDGE('',*,*,#17690,.T.) ;
#24616 = ORIENTED_EDGE('',*,*,#17691,.T.) ;
#24617 = ORIENTED_EDGE('',*,*,#17692,.T.) ;
#24618 = ORIENTED_EDGE('',*,*,#17693,.T.) ;
#24619 = ORIENTED_EDGE('',*,*,#17694,.F.) ;
#24620 = ORIENTED_EDGE('',*,*,#17694,.T.) ;
#24621 = ORIENTED_EDGE('',*,*,#17695,.T.) ;
#24622 = ORIENTED_EDGE('',*,*,#17696,.T.) ;
#24623 = ORIENTED_EDGE('',*,*,#17697,.T.) ;
#24624 = ORIENTED_EDGE('',*,*,#17698,.T.) ;
#24625 = ORIENTED_EDGE('',*,*,#17699,.T.) ;
#24626 = ORIENTED_EDGE('',*,*,#17700,.T.) ;
#24627 = ORIENTED_EDGE('',*,*,#17701,.T.) ;
#24628 = ORIENTED_EDGE('',*,*,#17702,.T.) ;
#24629 = ORIENTED_EDGE('',*,*,#17703,.T.) ;
#24630 = ORIENTED_EDGE('',*,*,#17704,.T.) ;
#24631 = ORIENTED_EDGE('',*,*,#17705,.T.) ;
#24632 = ORIENTED_EDGE('',*,*,#17706,.T.) ;
#24633 = ORIENTED_EDGE('',*,*,#17707,.T.) ;
#24634 = ORIENTED_EDGE('',*,*,#17708,.T.) ;
#24635 = ORIENTED_EDGE('',*,*,#17708,.F.) ;
#24636 = ORIENTED_EDGE('',*,*,#17709,.T.) ;
#24637 = ORIENTED_EDGE('',*,*,#17710,.T.) ;
#24638 = ORIENTED_EDGE('',*,*,#17711,.T.) ;
#24639 = ORIENTED_EDGE('',*,*,#17712,.T.) ;
#24640 = ORIENTED_EDGE('',*,*,#17713,.T.) ;
#24641 = ORIENTED_EDGE('',*,*,#17714,.T.) ;
#24642 = ORIENTED_EDGE('',*,*,#17715,.T.) ;
#24643 = ORIENTED_EDGE('',*,*,#17716,.T.) ;
#24644 = ORIENTED_EDGE('',*,*,#17717,.T.) ;
#24645 = ORIENTED_EDGE('',*,*,#17718,.T.) ;
#24646 = ORIENTED_EDGE('',*,*,#17719,.T.) ;
#24647 = ORIENTED_EDGE('',*,*,#17720,.T.) ;
#24648 = ORIENTED_EDGE('',*,*,#17721,.T.) ;
#24649 = ORIENTED_EDGE('',*,*,#17722,.F.) ;
#24650 = ORIENTED_EDGE('',*,*,#17722,.T.) ;
#24651 = ORIENTED_EDGE('',*,*,#17723,.T.) ;
#24652 = ORIENTED_EDGE('',*,*,#17724,.T.) ;
#24653 = ORIENTED_EDGE('',*,*,#17725,.T.) ;
#24654 = ORIENTED_EDGE('',*,*,#17726,.T.) ;
#24655 = ORIENTED_EDGE('',*,*,#17727,.T.) ;
#24656 = ORIENTED_EDGE('',*,*,#17728,.T.) ;
#24657 = ORIENTED_EDGE('',*,*,#17729,.T.) ;
#24658 = ORIENTED_EDGE('',*,*,#17730,.T.) ;
#24659 = ORIENTED_EDGE('',*,*,#17731,.T.) ;
#24660 = ORIENTED_EDGE('',*,*,#17732,.T.) ;
#24661 = ORIENTED_EDGE('',*,*,#17733,.T.) ;
#24662 = ORIENTED_EDGE('',*,*,#17734,.T.) ;
#24663 = ORIENTED_EDGE('',*,*,#17735,.T.) ;
#24664 = ORIENTED_EDGE('',*,*,#17736,.T.) ;
#24665 = ORIENTED_EDGE('',*,*,#17736,.F.) ;
#24666 = ORIENTED_EDGE('',*,*,#17737,.T.) ;
#24667 = ORIENTED_EDGE('',*,*,#17738,.T.) ;
#24668 = ORIENTED_EDGE('',*,*,#17739,.T.) ;
#24669 = ORIENTED_EDGE('',*,*,#17740,.T.) ;
#24670 = ORIENTED_EDGE('',*,*,#17741,.T.) ;
#24671 = ORIENTED_EDGE('',*,*,#17742,.T.) ;
#24672 = ORIENTED_EDGE('',*,*,#17743,.T.) ;
#24673 = ORIENTED_EDGE('',*,*,#17744,.T.) ;
#24674 = ORIENTED_EDGE('',*,*,#17745,.T.) ;
#24675 = ORIENTED_EDGE('',*,*,#17746,.T.) ;
#24676 = ORIENTED_EDGE('',*,*,#17747,.T.) ;
#24677 = ORIENTED_EDGE('',*,*,#17748,.T.) ;
#24678 = ORIENTED_EDGE('',*,*,#17749,.T.) ;
#24679 = ORIENTED_EDGE('',*,*,#17750,.F.) ;
#24680 = ORIENTED_EDGE('',*,*,#17750,.T.) ;
#24681 = ORIENTED_EDGE('',*,*,#17751,.T.) ;
#24682 = ORIENTED_EDGE('',*,*,#17752,.T.) ;
#24683 = ORIENTED_EDGE('',*,*,#17753,.T.) ;
#24684 = ORIENTED_EDGE('',*,*,#17754,.T.) ;
#24685 = ORIENTED_EDGE('',*,*,#17755,.T.) ;
#24686 = ORIENTED_EDGE('',*,*,#17756,.T.) ;
#24687 = ORIENTED_EDGE('',*,*,#17757,.T.) ;
#24688 = ORIENTED_EDGE('',*,*,#17758,.T.) ;
#24689 = ORIENTED_EDGE('',*,*,#17759,.T.) ;
#24690 = ORIENTED_EDGE('',*,*,#17760,.T.) ;
#24691 = ORIENTED_EDGE('',*,*,#17761,.T.) ;
#24692 = ORIENTED_EDGE('',*,*,#17762,.T.) ;
#24693 = ORIENTED_EDGE('',*,*,#17763,.T.) ;
#24694 = ORIENTED_EDGE('',*,*,#17764,.T.) ;
#24695 = ORIENTED_EDGE('',*,*,#17764,.F.) ;
#24696 = ORIENTED_EDGE('',*,*,#17765,.T.) ;
#24697 = ORIENTED_EDGE('',*,*,#17766,.T.) ;
#24698 = ORIENTED_EDGE('',*,*,#17767,.T.) ;
#24699 = ORIENTED_EDGE('',*,*,#17768,.T.) ;
#24700 = ORIENTED_EDGE('',*,*,#17769,.T.) ;
#24701 = ORIENTED_EDGE('',*,*,#17770,.T.) ;
#24702 = ORIENTED_EDGE('',*,*,#17771,.T.) ;
#24703 = ORIENTED_EDGE('',*,*,#17772,.T.) ;
#24704 = ORIENTED_EDGE('',*,*,#17773,.T.) ;
#24705 = ORIENTED_EDGE('',*,*,#17774,.T.) ;
#24706 = ORIENTED_EDGE('',*,*,#17775,.T.) ;
#24707 = ORIENTED_EDGE('',*,*,#17776,.T.) ;
#24708 = ORIENTED_EDGE('',*,*,#17777,.T.) ;
#24709 = ORIENTED_EDGE('',*,*,#17778,.F.) ;
#24710 = ORIENTED_EDGE('',*,*,#17778,.T.) ;
#24711 = ORIENTED_EDGE('',*,*,#17779,.T.) ;
#24712 = ORIENTED_EDGE('',*,*,#17780,.T.) ;
#24713 = ORIENTED_EDGE('',*,*,#17781,.T.) ;
#24714 = ORIENTED_EDGE('',*,*,#17782,.T.) ;
#24715 = ORIENTED_EDGE('',*,*,#17783,.T.) ;
#24716 = ORIENTED_EDGE('',*,*,#17784,.T.) ;
#24717 = ORIENTED_EDGE('',*,*,#17785,.T.) ;
#24718 = ORIENTED_EDGE('',*,*,#17786,.T.) ;
#24719 = ORIENTED_EDGE('',*,*,#17787,.T.) ;
#24720 = ORIENTED_EDGE('',*,*,#17788,.T.) ;
#24721 = ORIENTED_EDGE('',*,*,#17789,.T.) ;
#24722 = ORIENTED_EDGE('',*,*,#17790,.T.) ;
#24723 = ORIENTED_EDGE('',*,*,#17791,.T.) ;
#24724 = ORIENTED_EDGE('',*,*,#17792,.T.) ;
#24725 = ORIENTED_EDGE('',*,*,#17792,.F.) ;
#24726 = ORIENTED_EDGE('',*,*,#17793,.T.) ;
#24727 = ORIENTED_EDGE('',*,*,#17794,.T.) ;
#24728 = ORIENTED_EDGE('',*,*,#17795,.T.) ;
#24729 = ORIENTED_EDGE('',*,*,#17796,.T.) ;
#24730 = ORIENTED_EDGE('',*,*,#17797,.T.) ;
#24731 = ORIENTED_EDGE('',*,*,#17798,.T.) ;
#24732 = ORIENTED_EDGE('',*,*,#17799,.T.) ;
#24733 = ORIENTED_EDGE('',*,*,#17800,.T.) ;
#24734 = ORIENTED_EDGE('',*,*,#17801,.T.) ;
#24735 = ORIENTED_EDGE('',*,*,#17802,.T.) ;
#24736 = ORIENTED_EDGE('',*,*,#17803,.T.) ;
#24737 = ORIENTED_EDGE('',*,*,#17804,.T.) ;
#24738 = ORIENTED_EDGE('',*,*,#17805,.T.) ;
#24739 = ORIENTED_EDGE('',*,*,#17806,.F.) ;
#24740 = ORIENTED_EDGE('',*,*,#17806,.T.) ;
#24741 = ORIENTED_EDGE('',*,*,#17807,.T.) ;
#24742 = ORIENTED_EDGE('',*,*,#17808,.T.) ;
#24743 = ORIENTED_EDGE('',*,*,#17809,.T.) ;
#24744 = ORIENTED_EDGE('',*,*,#17810,.T.) ;
#24745 = ORIENTED_EDGE('',*,*,#17811,.T.) ;
#24746 = ORIENTED_EDGE('',*,*,#17812,.T.) ;
#24747 = ORIENTED_EDGE('',*,*,#17813,.T.) ;
#24748 = ORIENTED_EDGE('',*,*,#17814,.T.) ;
#24749 = ORIENTED_EDGE('',*,*,#17815,.T.) ;
#24750 = ORIENTED_EDGE('',*,*,#17816,.T.) ;
#24751 = ORIENTED_EDGE('',*,*,#17817,.T.) ;
#24752 = ORIENTED_EDGE('',*,*,#17818,.T.) ;
#24753 = ORIENTED_EDGE('',*,*,#17819,.T.) ;
#24754 = ORIENTED_EDGE('',*,*,#17820,.T.) ;
#24755 = ORIENTED_EDGE('',*,*,#17820,.F.) ;
#24756 = ORIENTED_EDGE('',*,*,#17821,.T.) ;
#24757 = ORIENTED_EDGE('',*,*,#17822,.T.) ;
#24758 = ORIENTED_EDGE('',*,*,#17823,.T.) ;
#24759 = ORIENTED_EDGE('',*,*,#17824,.T.) ;
#24760 = ORIENTED_EDGE('',*,*,#17825,.T.) ;
#24761 = ORIENTED_EDGE('',*,*,#17826,.T.) ;
#24762 = ORIENTED_EDGE('',*,*,#17827,.T.) ;
#24763 = ORIENTED_EDGE('',*,*,#17828,.T.) ;
#24764 = ORIENTED_EDGE('',*,*,#17829,.T.) ;
#24765 = ORIENTED_EDGE('',*,*,#17830,.T.) ;
#24766 = ORIENTED_EDGE('',*,*,#17831,.T.) ;
#24767 = ORIENTED_EDGE('',*,*,#17832,.T.) ;
#24768 = ORIENTED_EDGE('',*,*,#17833,.T.) ;
#24769 = ORIENTED_EDGE('',*,*,#17834,.F.) ;
#24770 = ORIENTED_EDGE('',*,*,#17834,.T.) ;
#24771 = ORIENTED_EDGE('',*,*,#17835,.T.) ;
#24772 = ORIENTED_EDGE('',*,*,#17836,.T.) ;
#24773 = ORIENTED_EDGE('',*,*,#17837,.T.) ;
#24774 = ORIENTED_EDGE('',*,*,#17838,.T.) ;
#24775 = ORIENTED_EDGE('',*,*,#17839,.T.) ;
#24776 = ORIENTED_EDGE('',*,*,#17840,.T.) ;
#24777 = ORIENTED_EDGE('',*,*,#17841,.T.) ;
#24778 = ORIENTED_EDGE('',*,*,#17842,.T.) ;
#24779 = ORIENTED_EDGE('',*,*,#17843,.T.) ;
#24780 = ORIENTED_EDGE('',*,*,#17844,.T.) ;
#24781 = ORIENTED_EDGE('',*,*,#17845,.T.) ;
#24782 = ORIENTED_EDGE('',*,*,#17846,.T.) ;
#24783 = ORIENTED_EDGE('',*,*,#17847,.T.) ;
#24784 = ORIENTED_EDGE('',*,*,#17848,.T.) ;
#24785 = ORIENTED_EDGE('',*,*,#17848,.F.) ;
#24786 = ORIENTED_EDGE('',*,*,#17849,.T.) ;
#24787 = ORIENTED_EDGE('',*,*,#17850,.T.) ;
#24788 = ORIENTED_EDGE('',*,*,#17851,.T.) ;
#24789 = ORIENTED_EDGE('',*,*,#17852,.T.) ;
#24790 = ORIENTED_EDGE('',*,*,#17853,.T.) ;
#24791 = ORIENTED_EDGE('',*,*,#17854,.T.) ;
#24792 = ORIENTED_EDGE('',*,*,#17855,.T.) ;
#24793 = ORIENTED_EDGE('',*,*,#17856,.T.) ;
#24794 = ORIENTED_EDGE('',*,*,#17857,.T.) ;
#24795 = ORIENTED_EDGE('',*,*,#17858,.T.) ;
#24796 = ORIENTED_EDGE('',*,*,#17859,.T.) ;
#24797 = ORIENTED_EDGE('',*,*,#17860,.T.) ;
#24798 = ORIENTED_EDGE('',*,*,#17861,.T.) ;
#24799 = ORIENTED_EDGE('',*,*,#17862,.F.) ;
#24800 = ORIENTED_EDGE('',*,*,#17862,.T.) ;
#24801 = ORIENTED_EDGE('',*,*,#17863,.T.) ;
#24802 = ORIENTED_EDGE('',*,*,#17864,.T.) ;
#24803 = ORIENTED_EDGE('',*,*,#17865,.T.) ;
#24804 = ORIENTED_EDGE('',*,*,#17866,.T.) ;
#24805 = ORIENTED_EDGE('',*,*,#17867,.T.) ;
#24806 = ORIENTED_EDGE('',*,*,#17868,.T.) ;
#24807 = ORIENTED_EDGE('',*,*,#17869,.T.) ;
#24808 = ORIENTED_EDGE('',*,*,#17870,.T.) ;
#24809 = ORIENTED_EDGE('',*,*,#17871,.T.) ;
#24810 = ORIENTED_EDGE('',*,*,#17872,.T.) ;
#24811 = ORIENTED_EDGE('',*,*,#17873,.T.) ;
#24812 = ORIENTED_EDGE('',*,*,#17874,.T.) ;
#24813 = ORIENTED_EDGE('',*,*,#17875,.T.) ;
#24814 = ORIENTED_EDGE('',*,*,#17876,.T.) ;
#24815 = ORIENTED_EDGE('',*,*,#17876,.F.) ;
#24816 = ORIENTED_EDGE('',*,*,#17877,.T.) ;
#24817 = ORIENTED_EDGE('',*,*,#17878,.T.) ;
#24818 = ORIENTED_EDGE('',*,*,#17879,.T.) ;
#24819 = ORIENTED_EDGE('',*,*,#17880,.T.) ;
#24820 = ORIENTED_EDGE('',*,*,#17881,.T.) ;
#24821 = ORIENTED_EDGE('',*,*,#17882,.T.) ;
#24822 = ORIENTED_EDGE('',*,*,#17883,.T.) ;
#24823 = ORIENTED_EDGE('',*,*,#17884,.T.) ;
#24824 = ORIENTED_EDGE('',*,*,#17885,.T.) ;
#24825 = ORIENTED_EDGE('',*,*,#17886,.T.) ;
#24826 = ORIENTED_EDGE('',*,*,#17887,.T.) ;
#24827 = ORIENTED_EDGE('',*,*,#17430,.T.) ;
#24828 = ORIENTED_EDGE('',*,*,#17445,.F.) ;
#24829 = ORIENTED_EDGE('',*,*,#17444,.T.) ;
#24830 = ORIENTED_EDGE('',*,*,#17447,.F.) ;
#24831 = ORIENTED_EDGE('',*,*,#17888,.F.) ;
#24832 = ORIENTED_EDGE('',*,*,#17431,.T.) ;
#24833 = ORIENTED_EDGE('',*,*,#17888,.T.) ;
#24834 = ORIENTED_EDGE('',*,*,#17446,.F.) ;
#24835 = ORIENTED_EDGE('',*,*,#17442,.T.) ;
#24836 = ORIENTED_EDGE('',*,*,#17450,.F.) ;
#24837 = ORIENTED_EDGE('',*,*,#17889,.F.) ;
#24838 = ORIENTED_EDGE('',*,*,#17432,.T.) ;
#24839 = ORIENTED_EDGE('',*,*,#17889,.T.) ;
#24840 = ORIENTED_EDGE('',*,*,#17449,.F.) ;
#24841 = ORIENTED_EDGE('',*,*,#17890,.T.) ;
#24842 = ORIENTED_EDGE('',*,*,#17891,.F.) ;
#24843 = ORIENTED_EDGE('',*,*,#17451,.F.) ;
#24844 = ORIENTED_EDGE('',*,*,#17892,.F.) ;
#24845 = ORIENTED_EDGE('',*,*,#17890,.F.) ;
#24846 = ORIENTED_EDGE('',*,*,#17448,.F.) ;
#24847 = ORIENTED_EDGE('',*,*,#17440,.T.) ;
#24848 = ORIENTED_EDGE('',*,*,#17891,.T.) ;
#24849 = ORIENTED_EDGE('',*,*,#17892,.T.) ;
#24850 = ORIENTED_EDGE('',*,*,#17453,.F.) ;
#24851 = ORIENTED_EDGE('',*,*,#17893,.T.) ;
#24852 = ORIENTED_EDGE('',*,*,#17894,.F.) ;
#24853 = ORIENTED_EDGE('',*,*,#17454,.F.) ;
#24854 = ORIENTED_EDGE('',*,*,#17895,.F.) ;
#24855 = ORIENTED_EDGE('',*,*,#17893,.F.) ;
#24856 = ORIENTED_EDGE('',*,*,#17452,.F.) ;
#24857 = ORIENTED_EDGE('',*,*,#17894,.T.) ;
#24858 = ORIENTED_EDGE('',*,*,#17895,.T.) ;
#24859 = ORIENTED_EDGE('',*,*,#17458,.F.) ;
#24860 = ORIENTED_EDGE('',*,*,#17896,.T.) ;
#24861 = ORIENTED_EDGE('',*,*,#17897,.F.) ;
#24862 = ORIENTED_EDGE('',*,*,#17459,.F.) ;
#24863 = ORIENTED_EDGE('',*,*,#17898,.F.) ;
#24864 = ORIENTED_EDGE('',*,*,#17896,.F.) ;
#24865 = ORIENTED_EDGE('',*,*,#17457,.F.) ;
#24866 = ORIENTED_EDGE('',*,*,#17455,.F.) ;
#24867 = ORIENTED_EDGE('',*,*,#17897,.T.) ;
#24868 = ORIENTED_EDGE('',*,*,#17898,.T.) ;
#24869 = ORIENTED_EDGE('',*,*,#17461,.F.) ;
#24870 = ORIENTED_EDGE('',*,*,#17899,.T.) ;
#24871 = ORIENTED_EDGE('',*,*,#17900,.F.) ;
#24872 = ORIENTED_EDGE('',*,*,#17462,.F.) ;
#24873 = ORIENTED_EDGE('',*,*,#17901,.F.) ;
#24874 = ORIENTED_EDGE('',*,*,#17899,.F.) ;
#24875 = ORIENTED_EDGE('',*,*,#17460,.F.) ;
#24876 = ORIENTED_EDGE('',*,*,#17900,.T.) ;
#24877 = ORIENTED_EDGE('',*,*,#17901,.T.) ;
#24878 = ORIENTED_EDGE('',*,*,#17464,.F.) ;
#24879 = ORIENTED_EDGE('',*,*,#17902,.T.) ;
#24880 = ORIENTED_EDGE('',*,*,#17903,.F.) ;
#24881 = ORIENTED_EDGE('',*,*,#17465,.F.) ;
#24882 = ORIENTED_EDGE('',*,*,#17904,.F.) ;
#24883 = ORIENTED_EDGE('',*,*,#17902,.F.) ;
#24884 = ORIENTED_EDGE('',*,*,#17463,.F.) ;
#24885 = ORIENTED_EDGE('',*,*,#17903,.T.) ;
#24886 = ORIENTED_EDGE('',*,*,#17904,.T.) ;
#24887 = ORIENTED_EDGE('',*,*,#17467,.F.) ;
#24888 = ORIENTED_EDGE('',*,*,#17905,.T.) ;
#24889 = ORIENTED_EDGE('',*,*,#17906,.F.) ;
#24890 = ORIENTED_EDGE('',*,*,#17468,.F.) ;
#24891 = ORIENTED_EDGE('',*,*,#17907,.F.) ;
#24892 = ORIENTED_EDGE('',*,*,#17905,.F.) ;
#24893 = ORIENTED_EDGE('',*,*,#17466,.F.) ;
#24894 = ORIENTED_EDGE('',*,*,#17906,.T.) ;
#24895 = ORIENTED_EDGE('',*,*,#17907,.T.) ;
#24896 = ORIENTED_EDGE('',*,*,#17472,.F.) ;
#24897 = ORIENTED_EDGE('',*,*,#17908,.T.) ;
#24898 = ORIENTED_EDGE('',*,*,#17909,.F.) ;
#24899 = ORIENTED_EDGE('',*,*,#17473,.F.) ;
#24900 = ORIENTED_EDGE('',*,*,#17910,.F.) ;
#24901 = ORIENTED_EDGE('',*,*,#17908,.F.) ;
#24902 = ORIENTED_EDGE('',*,*,#17471,.F.) ;
#24903 = ORIENTED_EDGE('',*,*,#17469,.F.) ;
#24904 = ORIENTED_EDGE('',*,*,#17909,.T.) ;
#24905 = ORIENTED_EDGE('',*,*,#17910,.T.) ;
#24906 = ORIENTED_EDGE('',*,*,#17475,.F.) ;
#24907 = ORIENTED_EDGE('',*,*,#17911,.T.) ;
#24908 = ORIENTED_EDGE('',*,*,#17912,.F.) ;
#24909 = ORIENTED_EDGE('',*,*,#17476,.F.) ;
#24910 = ORIENTED_EDGE('',*,*,#17913,.F.) ;
#24911 = ORIENTED_EDGE('',*,*,#17911,.F.) ;
#24912 = ORIENTED_EDGE('',*,*,#17474,.F.) ;
#24913 = ORIENTED_EDGE('',*,*,#17912,.T.) ;
#24914 = ORIENTED_EDGE('',*,*,#17913,.T.) ;
#24915 = ORIENTED_EDGE('',*,*,#17478,.F.) ;
#24916 = ORIENTED_EDGE('',*,*,#17914,.T.) ;
#24917 = ORIENTED_EDGE('',*,*,#17915,.F.) ;
#24918 = ORIENTED_EDGE('',*,*,#17479,.F.) ;
#24919 = ORIENTED_EDGE('',*,*,#17916,.F.) ;
#24920 = ORIENTED_EDGE('',*,*,#17914,.F.) ;
#24921 = ORIENTED_EDGE('',*,*,#17477,.F.) ;
#24922 = ORIENTED_EDGE('',*,*,#17915,.T.) ;
#24923 = ORIENTED_EDGE('',*,*,#17916,.T.) ;
#24924 = ORIENTED_EDGE('',*,*,#17481,.F.) ;
#24925 = ORIENTED_EDGE('',*,*,#17917,.T.) ;
#24926 = ORIENTED_EDGE('',*,*,#17918,.F.) ;
#24927 = ORIENTED_EDGE('',*,*,#17482,.F.) ;
#24928 = ORIENTED_EDGE('',*,*,#17919,.F.) ;
#24929 = ORIENTED_EDGE('',*,*,#17917,.F.) ;
#24930 = ORIENTED_EDGE('',*,*,#17480,.F.) ;
#24931 = ORIENTED_EDGE('',*,*,#17918,.T.) ;
#24932 = ORIENTED_EDGE('',*,*,#17919,.T.) ;
#24933 = ORIENTED_EDGE('',*,*,#17486,.F.) ;
#24934 = ORIENTED_EDGE('',*,*,#17920,.T.) ;
#24935 = ORIENTED_EDGE('',*,*,#17921,.F.) ;
#24936 = ORIENTED_EDGE('',*,*,#17487,.F.) ;
#24937 = ORIENTED_EDGE('',*,*,#17922,.F.) ;
#24938 = ORIENTED_EDGE('',*,*,#17920,.F.) ;
#24939 = ORIENTED_EDGE('',*,*,#17485,.F.) ;
#24940 = ORIENTED_EDGE('',*,*,#17483,.F.) ;
#24941 = ORIENTED_EDGE('',*,*,#17921,.T.) ;
#24942 = ORIENTED_EDGE('',*,*,#17922,.T.) ;
#24943 = ORIENTED_EDGE('',*,*,#17489,.F.) ;
#24944 = ORIENTED_EDGE('',*,*,#17923,.T.) ;
#24945 = ORIENTED_EDGE('',*,*,#17924,.F.) ;
#24946 = ORIENTED_EDGE('',*,*,#17490,.F.) ;
#24947 = ORIENTED_EDGE('',*,*,#17925,.F.) ;
#24948 = ORIENTED_EDGE('',*,*,#17923,.F.) ;
#24949 = ORIENTED_EDGE('',*,*,#17488,.F.) ;
#24950 = ORIENTED_EDGE('',*,*,#17924,.T.) ;
#24951 = ORIENTED_EDGE('',*,*,#17925,.T.) ;
#24952 = ORIENTED_EDGE('',*,*,#17492,.F.) ;
#24953 = ORIENTED_EDGE('',*,*,#17926,.T.) ;
#24954 = ORIENTED_EDGE('',*,*,#17927,.F.) ;
#24955 = ORIENTED_EDGE('',*,*,#17493,.F.) ;
#24956 = ORIENTED_EDGE('',*,*,#17928,.F.) ;
#24957 = ORIENTED_EDGE('',*,*,#17926,.F.) ;
#24958 = ORIENTED_EDGE('',*,*,#17491,.F.) ;
#24959 = ORIENTED_EDGE('',*,*,#17927,.T.) ;
#24960 = ORIENTED_EDGE('',*,*,#17928,.T.) ;
#24961 = ORIENTED_EDGE('',*,*,#17495,.F.) ;
#24962 = ORIENTED_EDGE('',*,*,#17929,.T.) ;
#24963 = ORIENTED_EDGE('',*,*,#17930,.F.) ;
#24964 = ORIENTED_EDGE('',*,*,#17496,.F.) ;
#24965 = ORIENTED_EDGE('',*,*,#17931,.F.) ;
#24966 = ORIENTED_EDGE('',*,*,#17929,.F.) ;
#24967 = ORIENTED_EDGE('',*,*,#17494,.F.) ;
#24968 = ORIENTED_EDGE('',*,*,#17930,.T.) ;
#24969 = ORIENTED_EDGE('',*,*,#17931,.T.) ;
#24970 = ORIENTED_EDGE('',*,*,#17500,.F.) ;
#24971 = ORIENTED_EDGE('',*,*,#17932,.T.) ;
#24972 = ORIENTED_EDGE('',*,*,#17933,.F.) ;
#24973 = ORIENTED_EDGE('',*,*,#17501,.F.) ;
#24974 = ORIENTED_EDGE('',*,*,#17934,.F.) ;
#24975 = ORIENTED_EDGE('',*,*,#17932,.F.) ;
#24976 = ORIENTED_EDGE('',*,*,#17499,.F.) ;
#24977 = ORIENTED_EDGE('',*,*,#17497,.F.) ;
#24978 = ORIENTED_EDGE('',*,*,#17933,.T.) ;
#24979 = ORIENTED_EDGE('',*,*,#17934,.T.) ;
#24980 = ORIENTED_EDGE('',*,*,#17503,.F.) ;
#24981 = ORIENTED_EDGE('',*,*,#17935,.T.) ;
#24982 = ORIENTED_EDGE('',*,*,#17936,.F.) ;
#24983 = ORIENTED_EDGE('',*,*,#17504,.F.) ;
#24984 = ORIENTED_EDGE('',*,*,#17937,.F.) ;
#24985 = ORIENTED_EDGE('',*,*,#17935,.F.) ;
#24986 = ORIENTED_EDGE('',*,*,#17502,.F.) ;
#24987 = ORIENTED_EDGE('',*,*,#17936,.T.) ;
#24988 = ORIENTED_EDGE('',*,*,#17937,.T.) ;
#24989 = ORIENTED_EDGE('',*,*,#17506,.F.) ;
#24990 = ORIENTED_EDGE('',*,*,#17938,.T.) ;
#24991 = ORIENTED_EDGE('',*,*,#17939,.F.) ;
#24992 = ORIENTED_EDGE('',*,*,#17507,.F.) ;
#24993 = ORIENTED_EDGE('',*,*,#17940,.F.) ;
#24994 = ORIENTED_EDGE('',*,*,#17938,.F.) ;
#24995 = ORIENTED_EDGE('',*,*,#17505,.F.) ;
#24996 = ORIENTED_EDGE('',*,*,#17939,.T.) ;
#24997 = ORIENTED_EDGE('',*,*,#17940,.T.) ;
#24998 = ORIENTED_EDGE('',*,*,#17509,.F.) ;
#24999 = ORIENTED_EDGE('',*,*,#17941,.T.) ;
#25000 = ORIENTED_EDGE('',*,*,#17942,.F.) ;
#25001 = ORIENTED_EDGE('',*,*,#17510,.F.) ;
#25002 = ORIENTED_EDGE('',*,*,#17943,.F.) ;
#25003 = ORIENTED_EDGE('',*,*,#17941,.F.) ;
#25004 = ORIENTED_EDGE('',*,*,#17508,.F.) ;
#25005 = ORIENTED_EDGE('',*,*,#17942,.T.) ;
#25006 = ORIENTED_EDGE('',*,*,#17943,.T.) ;
#25007 = ORIENTED_EDGE('',*,*,#17514,.F.) ;
#25008 = ORIENTED_EDGE('',*,*,#17944,.T.) ;
#25009 = ORIENTED_EDGE('',*,*,#17945,.F.) ;
#25010 = ORIENTED_EDGE('',*,*,#17515,.F.) ;
#25011 = ORIENTED_EDGE('',*,*,#17946,.F.) ;
#25012 = ORIENTED_EDGE('',*,*,#17944,.F.) ;
#25013 = ORIENTED_EDGE('',*,*,#17513,.F.) ;
#25014 = ORIENTED_EDGE('',*,*,#17511,.F.) ;
#25015 = ORIENTED_EDGE('',*,*,#17945,.T.) ;
#25016 = ORIENTED_EDGE('',*,*,#17946,.T.) ;
#25017 = ORIENTED_EDGE('',*,*,#17517,.F.) ;
#25018 = ORIENTED_EDGE('',*,*,#17947,.T.) ;
#25019 = ORIENTED_EDGE('',*,*,#17948,.F.) ;
#25020 = ORIENTED_EDGE('',*,*,#17518,.F.) ;
#25021 = ORIENTED_EDGE('',*,*,#17949,.F.) ;
#25022 = ORIENTED_EDGE('',*,*,#17947,.F.) ;
#25023 = ORIENTED_EDGE('',*,*,#17516,.F.) ;
#25024 = ORIENTED_EDGE('',*,*,#17948,.T.) ;
#25025 = ORIENTED_EDGE('',*,*,#17949,.T.) ;
#25026 = ORIENTED_EDGE('',*,*,#17520,.F.) ;
#25027 = ORIENTED_EDGE('',*,*,#17950,.T.) ;
#25028 = ORIENTED_EDGE('',*,*,#17951,.F.) ;
#25029 = ORIENTED_EDGE('',*,*,#17521,.F.) ;
#25030 = ORIENTED_EDGE('',*,*,#17952,.F.) ;
#25031 = ORIENTED_EDGE('',*,*,#17950,.F.) ;
#25032 = ORIENTED_EDGE('',*,*,#17519,.F.) ;
#25033 = ORIENTED_EDGE('',*,*,#17951,.T.) ;
#25034 = ORIENTED_EDGE('',*,*,#17952,.T.) ;
#25035 = ORIENTED_EDGE('',*,*,#17523,.F.) ;
#25036 = ORIENTED_EDGE('',*,*,#17953,.T.) ;
#25037 = ORIENTED_EDGE('',*,*,#17954,.F.) ;
#25038 = ORIENTED_EDGE('',*,*,#17524,.F.) ;
#25039 = ORIENTED_EDGE('',*,*,#17955,.F.) ;
#25040 = ORIENTED_EDGE('',*,*,#17953,.F.) ;
#25041 = ORIENTED_EDGE('',*,*,#17522,.F.) ;
#25042 = ORIENTED_EDGE('',*,*,#17954,.T.) ;
#25043 = ORIENTED_EDGE('',*,*,#17955,.T.) ;
#25044 = ORIENTED_EDGE('',*,*,#17528,.F.) ;
#25045 = ORIENTED_EDGE('',*,*,#17956,.T.) ;
#25046 = ORIENTED_EDGE('',*,*,#17957,.F.) ;
#25047 = ORIENTED_EDGE('',*,*,#17529,.F.) ;
#25048 = ORIENTED_EDGE('',*,*,#17958,.F.) ;
#25049 = ORIENTED_EDGE('',*,*,#17956,.F.) ;
#25050 = ORIENTED_EDGE('',*,*,#17527,.F.) ;
#25051 = ORIENTED_EDGE('',*,*,#17525,.F.) ;
#25052 = ORIENTED_EDGE('',*,*,#17957,.T.) ;
#25053 = ORIENTED_EDGE('',*,*,#17958,.T.) ;
#25054 = ORIENTED_EDGE('',*,*,#17531,.F.) ;
#25055 = ORIENTED_EDGE('',*,*,#17959,.T.) ;
#25056 = ORIENTED_EDGE('',*,*,#17960,.F.) ;
#25057 = ORIENTED_EDGE('',*,*,#17532,.F.) ;
#25058 = ORIENTED_EDGE('',*,*,#17961,.F.) ;
#25059 = ORIENTED_EDGE('',*,*,#17959,.F.) ;
#25060 = ORIENTED_EDGE('',*,*,#17530,.F.) ;
#25061 = ORIENTED_EDGE('',*,*,#17960,.T.) ;
#25062 = ORIENTED_EDGE('',*,*,#17961,.T.) ;
#25063 = ORIENTED_EDGE('',*,*,#17534,.F.) ;
#25064 = ORIENTED_EDGE('',*,*,#17962,.T.) ;
#25065 = ORIENTED_EDGE('',*,*,#17963,.F.) ;
#25066 = ORIENTED_EDGE('',*,*,#17535,.F.) ;
#25067 = ORIENTED_EDGE('',*,*,#17964,.F.) ;
#25068 = ORIENTED_EDGE('',*,*,#17962,.F.) ;
#25069 = ORIENTED_EDGE('',*,*,#17533,.F.) ;
#25070 = ORIENTED_EDGE('',*,*,#17963,.T.) ;
#25071 = ORIENTED_EDGE('',*,*,#17964,.T.) ;
#25072 = ORIENTED_EDGE('',*,*,#17537,.F.) ;
#25073 = ORIENTED_EDGE('',*,*,#17965,.T.) ;
#25074 = ORIENTED_EDGE('',*,*,#17966,.F.) ;
#25075 = ORIENTED_EDGE('',*,*,#17538,.F.) ;
#25076 = ORIENTED_EDGE('',*,*,#17967,.F.) ;
#25077 = ORIENTED_EDGE('',*,*,#17965,.F.) ;
#25078 = ORIENTED_EDGE('',*,*,#17536,.F.) ;
#25079 = ORIENTED_EDGE('',*,*,#17966,.T.) ;
#25080 = ORIENTED_EDGE('',*,*,#17967,.T.) ;
#25081 = ORIENTED_EDGE('',*,*,#17542,.F.) ;
#25082 = ORIENTED_EDGE('',*,*,#17968,.T.) ;
#25083 = ORIENTED_EDGE('',*,*,#17969,.F.) ;
#25084 = ORIENTED_EDGE('',*,*,#17543,.F.) ;
#25085 = ORIENTED_EDGE('',*,*,#17970,.F.) ;
#25086 = ORIENTED_EDGE('',*,*,#17968,.F.) ;
#25087 = ORIENTED_EDGE('',*,*,#17541,.F.) ;
#25088 = ORIENTED_EDGE('',*,*,#17539,.F.) ;
#25089 = ORIENTED_EDGE('',*,*,#17969,.T.) ;
#25090 = ORIENTED_EDGE('',*,*,#17970,.T.) ;
#25091 = ORIENTED_EDGE('',*,*,#17545,.F.) ;
#25092 = ORIENTED_EDGE('',*,*,#17971,.T.) ;
#25093 = ORIENTED_EDGE('',*,*,#17972,.F.) ;
#25094 = ORIENTED_EDGE('',*,*,#17546,.F.) ;
#25095 = ORIENTED_EDGE('',*,*,#17973,.F.) ;
#25096 = ORIENTED_EDGE('',*,*,#17971,.F.) ;
#25097 = ORIENTED_EDGE('',*,*,#17544,.F.) ;
#25098 = ORIENTED_EDGE('',*,*,#17972,.T.) ;
#25099 = ORIENTED_EDGE('',*,*,#17973,.T.) ;
#25100 = ORIENTED_EDGE('',*,*,#17548,.F.) ;
#25101 = ORIENTED_EDGE('',*,*,#17974,.T.) ;
#25102 = ORIENTED_EDGE('',*,*,#17975,.F.) ;
#25103 = ORIENTED_EDGE('',*,*,#17549,.F.) ;
#25104 = ORIENTED_EDGE('',*,*,#17976,.F.) ;
#25105 = ORIENTED_EDGE('',*,*,#17974,.F.) ;
#25106 = ORIENTED_EDGE('',*,*,#17547,.F.) ;
#25107 = ORIENTED_EDGE('',*,*,#17975,.T.) ;
#25108 = ORIENTED_EDGE('',*,*,#17976,.T.) ;
#25109 = ORIENTED_EDGE('',*,*,#17551,.F.) ;
#25110 = ORIENTED_EDGE('',*,*,#17977,.T.) ;
#25111 = ORIENTED_EDGE('',*,*,#17978,.F.) ;
#25112 = ORIENTED_EDGE('',*,*,#17552,.F.) ;
#25113 = ORIENTED_EDGE('',*,*,#17979,.F.) ;
#25114 = ORIENTED_EDGE('',*,*,#17977,.F.) ;
#25115 = ORIENTED_EDGE('',*,*,#17550,.F.) ;
#25116 = ORIENTED_EDGE('',*,*,#17978,.T.) ;
#25117 = ORIENTED_EDGE('',*,*,#17979,.T.) ;
#25118 = ORIENTED_EDGE('',*,*,#17556,.F.) ;
#25119 = ORIENTED_EDGE('',*,*,#17980,.T.) ;
#25120 = ORIENTED_EDGE('',*,*,#17981,.F.) ;
#25121 = ORIENTED_EDGE('',*,*,#17557,.F.) ;
#25122 = ORIENTED_EDGE('',*,*,#17982,.F.) ;
#25123 = ORIENTED_EDGE('',*,*,#17980,.F.) ;
#25124 = ORIENTED_EDGE('',*,*,#17555,.F.) ;
#25125 = ORIENTED_EDGE('',*,*,#17553,.F.) ;
#25126 = ORIENTED_EDGE('',*,*,#17981,.T.) ;
#25127 = ORIENTED_EDGE('',*,*,#17982,.T.) ;
#25128 = ORIENTED_EDGE('',*,*,#17559,.F.) ;
#25129 = ORIENTED_EDGE('',*,*,#17983,.T.) ;
#25130 = ORIENTED_EDGE('',*,*,#17984,.F.) ;
#25131 = ORIENTED_EDGE('',*,*,#17560,.F.) ;
#25132 = ORIENTED_EDGE('',*,*,#17985,.F.) ;
#25133 = ORIENTED_EDGE('',*,*,#17983,.F.) ;
#25134 = ORIENTED_EDGE('',*,*,#17558,.F.) ;
#25135 = ORIENTED_EDGE('',*,*,#17984,.T.) ;
#25136 = ORIENTED_EDGE('',*,*,#17985,.T.) ;
#25137 = ORIENTED_EDGE('',*,*,#17562,.F.) ;
#25138 = ORIENTED_EDGE('',*,*,#17986,.T.) ;
#25139 = ORIENTED_EDGE('',*,*,#17987,.F.) ;
#25140 = ORIENTED_EDGE('',*,*,#17563,.F.) ;
#25141 = ORIENTED_EDGE('',*,*,#17988,.F.) ;
#25142 = ORIENTED_EDGE('',*,*,#17986,.F.) ;
#25143 = ORIENTED_EDGE('',*,*,#17561,.F.) ;
#25144 = ORIENTED_EDGE('',*,*,#17987,.T.) ;
#25145 = ORIENTED_EDGE('',*,*,#17988,.T.) ;
#25146 = ORIENTED_EDGE('',*,*,#17565,.F.) ;
#25147 = ORIENTED_EDGE('',*,*,#17989,.T.) ;
#25148 = ORIENTED_EDGE('',*,*,#17990,.F.) ;
#25149 = ORIENTED_EDGE('',*,*,#17566,.F.) ;
#25150 = ORIENTED_EDGE('',*,*,#17991,.F.) ;
#25151 = ORIENTED_EDGE('',*,*,#17989,.F.) ;
#25152 = ORIENTED_EDGE('',*,*,#17564,.F.) ;
#25153 = ORIENTED_EDGE('',*,*,#17990,.T.) ;
#25154 = ORIENTED_EDGE('',*,*,#17991,.T.) ;
#25155 = ORIENTED_EDGE('',*,*,#17570,.F.) ;
#25156 = ORIENTED_EDGE('',*,*,#17992,.T.) ;
#25157 = ORIENTED_EDGE('',*,*,#17993,.F.) ;
#25158 = ORIENTED_EDGE('',*,*,#17571,.F.) ;
#25159 = ORIENTED_EDGE('',*,*,#17994,.F.) ;
#25160 = ORIENTED_EDGE('',*,*,#17992,.F.) ;
#25161 = ORIENTED_EDGE('',*,*,#17569,.F.) ;
#25162 = ORIENTED_EDGE('',*,*,#17567,.F.) ;
#25163 = ORIENTED_EDGE('',*,*,#17993,.T.) ;
#25164 = ORIENTED_EDGE('',*,*,#17994,.T.) ;
#25165 = ORIENTED_EDGE('',*,*,#17573,.F.) ;
#25166 = ORIENTED_EDGE('',*,*,#17995,.T.) ;
#25167 = ORIENTED_EDGE('',*,*,#17996,.F.) ;
#25168 = ORIENTED_EDGE('',*,*,#17574,.F.) ;
#25169 = ORIENTED_EDGE('',*,*,#17997,.F.) ;
#25170 = ORIENTED_EDGE('',*,*,#17995,.F.) ;
#25171 = ORIENTED_EDGE('',*,*,#17572,.F.) ;
#25172 = ORIENTED_EDGE('',*,*,#17996,.T.) ;
#25173 = ORIENTED_EDGE('',*,*,#17997,.T.) ;
#25174 = ORIENTED_EDGE('',*,*,#17576,.F.) ;
#25175 = ORIENTED_EDGE('',*,*,#17998,.T.) ;
#25176 = ORIENTED_EDGE('',*,*,#17999,.F.) ;
#25177 = ORIENTED_EDGE('',*,*,#17577,.F.) ;
#25178 = ORIENTED_EDGE('',*,*,#18000,.F.) ;
#25179 = ORIENTED_EDGE('',*,*,#17998,.F.) ;
#25180 = ORIENTED_EDGE('',*,*,#17575,.F.) ;
#25181 = ORIENTED_EDGE('',*,*,#17999,.T.) ;
#25182 = ORIENTED_EDGE('',*,*,#18000,.T.) ;
#25183 = ORIENTED_EDGE('',*,*,#17579,.F.) ;
#25184 = ORIENTED_EDGE('',*,*,#18001,.T.) ;
#25185 = ORIENTED_EDGE('',*,*,#18002,.F.) ;
#25186 = ORIENTED_EDGE('',*,*,#17580,.F.) ;
#25187 = ORIENTED_EDGE('',*,*,#18003,.F.) ;
#25188 = ORIENTED_EDGE('',*,*,#18001,.F.) ;
#25189 = ORIENTED_EDGE('',*,*,#17578,.F.) ;
#25190 = ORIENTED_EDGE('',*,*,#18002,.T.) ;
#25191 = ORIENTED_EDGE('',*,*,#18003,.T.) ;
#25192 = ORIENTED_EDGE('',*,*,#17584,.F.) ;
#25193 = ORIENTED_EDGE('',*,*,#18004,.T.) ;
#25194 = ORIENTED_EDGE('',*,*,#18005,.F.) ;
#25195 = ORIENTED_EDGE('',*,*,#17585,.F.) ;
#25196 = ORIENTED_EDGE('',*,*,#18006,.F.) ;
#25197 = ORIENTED_EDGE('',*,*,#18004,.F.) ;
#25198 = ORIENTED_EDGE('',*,*,#17583,.F.) ;
#25199 = ORIENTED_EDGE('',*,*,#17581,.F.) ;
#25200 = ORIENTED_EDGE('',*,*,#18005,.T.) ;
#25201 = ORIENTED_EDGE('',*,*,#18006,.T.) ;
#25202 = ORIENTED_EDGE('',*,*,#17587,.F.) ;
#25203 = ORIENTED_EDGE('',*,*,#18007,.T.) ;
#25204 = ORIENTED_EDGE('',*,*,#18008,.F.) ;
#25205 = ORIENTED_EDGE('',*,*,#17588,.F.) ;
#25206 = ORIENTED_EDGE('',*,*,#18009,.F.) ;
#25207 = ORIENTED_EDGE('',*,*,#18007,.F.) ;
#25208 = ORIENTED_EDGE('',*,*,#17586,.F.) ;
#25209 = ORIENTED_EDGE('',*,*,#18008,.T.) ;
#25210 = ORIENTED_EDGE('',*,*,#18009,.T.) ;
#25211 = ORIENTED_EDGE('',*,*,#17590,.F.) ;
#25212 = ORIENTED_EDGE('',*,*,#18010,.T.) ;
#25213 = ORIENTED_EDGE('',*,*,#18011,.F.) ;
#25214 = ORIENTED_EDGE('',*,*,#17591,.F.) ;
#25215 = ORIENTED_EDGE('',*,*,#18012,.F.) ;
#25216 = ORIENTED_EDGE('',*,*,#18010,.F.) ;
#25217 = ORIENTED_EDGE('',*,*,#17589,.F.) ;
#25218 = ORIENTED_EDGE('',*,*,#18011,.T.) ;
#25219 = ORIENTED_EDGE('',*,*,#18012,.T.) ;
#25220 = ORIENTED_EDGE('',*,*,#17593,.F.) ;
#25221 = ORIENTED_EDGE('',*,*,#18013,.T.) ;
#25222 = ORIENTED_EDGE('',*,*,#18014,.F.) ;
#25223 = ORIENTED_EDGE('',*,*,#17594,.F.) ;
#25224 = ORIENTED_EDGE('',*,*,#18015,.F.) ;
#25225 = ORIENTED_EDGE('',*,*,#18013,.F.) ;
#25226 = ORIENTED_EDGE('',*,*,#17592,.F.) ;
#25227 = ORIENTED_EDGE('',*,*,#18014,.T.) ;
#25228 = ORIENTED_EDGE('',*,*,#18015,.T.) ;
#25229 = ORIENTED_EDGE('',*,*,#17598,.F.) ;
#25230 = ORIENTED_EDGE('',*,*,#18016,.T.) ;
#25231 = ORIENTED_EDGE('',*,*,#18017,.F.) ;
#25232 = ORIENTED_EDGE('',*,*,#17599,.F.) ;
#25233 = ORIENTED_EDGE('',*,*,#18018,.F.) ;
#25234 = ORIENTED_EDGE('',*,*,#18016,.F.) ;
#25235 = ORIENTED_EDGE('',*,*,#17597,.F.) ;
#25236 = ORIENTED_EDGE('',*,*,#17595,.F.) ;
#25237 = ORIENTED_EDGE('',*,*,#18017,.T.) ;
#25238 = ORIENTED_EDGE('',*,*,#18018,.T.) ;
#25239 = ORIENTED_EDGE('',*,*,#17601,.F.) ;
#25240 = ORIENTED_EDGE('',*,*,#18019,.T.) ;
#25241 = ORIENTED_EDGE('',*,*,#18020,.F.) ;
#25242 = ORIENTED_EDGE('',*,*,#17602,.F.) ;
#25243 = ORIENTED_EDGE('',*,*,#18021,.F.) ;
#25244 = ORIENTED_EDGE('',*,*,#18019,.F.) ;
#25245 = ORIENTED_EDGE('',*,*,#17600,.F.) ;
#25246 = ORIENTED_EDGE('',*,*,#18020,.T.) ;
#25247 = ORIENTED_EDGE('',*,*,#18021,.T.) ;
#25248 = ORIENTED_EDGE('',*,*,#17604,.F.) ;
#25249 = ORIENTED_EDGE('',*,*,#18022,.T.) ;
#25250 = ORIENTED_EDGE('',*,*,#18023,.F.) ;
#25251 = ORIENTED_EDGE('',*,*,#17605,.F.) ;
#25252 = ORIENTED_EDGE('',*,*,#18024,.F.) ;
#25253 = ORIENTED_EDGE('',*,*,#18022,.F.) ;
#25254 = ORIENTED_EDGE('',*,*,#17603,.F.) ;
#25255 = ORIENTED_EDGE('',*,*,#18023,.T.) ;
#25256 = ORIENTED_EDGE('',*,*,#18024,.T.) ;
#25257 = ORIENTED_EDGE('',*,*,#17607,.F.) ;
#25258 = ORIENTED_EDGE('',*,*,#18025,.T.) ;
#25259 = ORIENTED_EDGE('',*,*,#18026,.F.) ;
#25260 = ORIENTED_EDGE('',*,*,#17608,.F.) ;
#25261 = ORIENTED_EDGE('',*,*,#18027,.F.) ;
#25262 = ORIENTED_EDGE('',*,*,#18025,.F.) ;
#25263 = ORIENTED_EDGE('',*,*,#17606,.F.) ;
#25264 = ORIENTED_EDGE('',*,*,#18026,.T.) ;
#25265 = ORIENTED_EDGE('',*,*,#18027,.T.) ;
#25266 = ORIENTED_EDGE('',*,*,#17612,.F.) ;
#25267 = ORIENTED_EDGE('',*,*,#18028,.T.) ;
#25268 = ORIENTED_EDGE('',*,*,#18029,.F.) ;
#25269 = ORIENTED_EDGE('',*,*,#17613,.F.) ;
#25270 = ORIENTED_EDGE('',*,*,#18030,.F.) ;
#25271 = ORIENTED_EDGE('',*,*,#18028,.F.) ;
#25272 = ORIENTED_EDGE('',*,*,#17611,.F.) ;
#25273 = ORIENTED_EDGE('',*,*,#17609,.F.) ;
#25274 = ORIENTED_EDGE('',*,*,#18029,.T.) ;
#25275 = ORIENTED_EDGE('',*,*,#18030,.T.) ;
#25276 = ORIENTED_EDGE('',*,*,#17615,.F.) ;
#25277 = ORIENTED_EDGE('',*,*,#18031,.T.) ;
#25278 = ORIENTED_EDGE('',*,*,#18032,.F.) ;
#25279 = ORIENTED_EDGE('',*,*,#17616,.F.) ;
#25280 = ORIENTED_EDGE('',*,*,#18033,.F.) ;
#25281 = ORIENTED_EDGE('',*,*,#18031,.F.) ;
#25282 = ORIENTED_EDGE('',*,*,#17614,.F.) ;
#25283 = ORIENTED_EDGE('',*,*,#18032,.T.) ;
#25284 = ORIENTED_EDGE('',*,*,#18033,.T.) ;
#25285 = ORIENTED_EDGE('',*,*,#17618,.F.) ;
#25286 = ORIENTED_EDGE('',*,*,#18034,.T.) ;
#25287 = ORIENTED_EDGE('',*,*,#18035,.F.) ;
#25288 = ORIENTED_EDGE('',*,*,#17619,.F.) ;
#25289 = ORIENTED_EDGE('',*,*,#18036,.F.) ;
#25290 = ORIENTED_EDGE('',*,*,#18034,.F.) ;
#25291 = ORIENTED_EDGE('',*,*,#17617,.F.) ;
#25292 = ORIENTED_EDGE('',*,*,#18035,.T.) ;
#25293 = ORIENTED_EDGE('',*,*,#18036,.T.) ;
#25294 = ORIENTED_EDGE('',*,*,#17621,.F.) ;
#25295 = ORIENTED_EDGE('',*,*,#18037,.T.) ;
#25296 = ORIENTED_EDGE('',*,*,#18038,.F.) ;
#25297 = ORIENTED_EDGE('',*,*,#17622,.F.) ;
#25298 = ORIENTED_EDGE('',*,*,#18039,.F.) ;
#25299 = ORIENTED_EDGE('',*,*,#18037,.F.) ;
#25300 = ORIENTED_EDGE('',*,*,#17620,.F.) ;
#25301 = ORIENTED_EDGE('',*,*,#18038,.T.) ;
#25302 = ORIENTED_EDGE('',*,*,#18039,.T.) ;
#25303 = ORIENTED_EDGE('',*,*,#17626,.F.) ;
#25304 = ORIENTED_EDGE('',*,*,#18040,.T.) ;
#25305 = ORIENTED_EDGE('',*,*,#18041,.F.) ;
#25306 = ORIENTED_EDGE('',*,*,#17627,.F.) ;
#25307 = ORIENTED_EDGE('',*,*,#18042,.F.) ;
#25308 = ORIENTED_EDGE('',*,*,#18040,.F.) ;
#25309 = ORIENTED_EDGE('',*,*,#17625,.F.) ;
#25310 = ORIENTED_EDGE('',*,*,#17623,.F.) ;
#25311 = ORIENTED_EDGE('',*,*,#18041,.T.) ;
#25312 = ORIENTED_EDGE('',*,*,#18042,.T.) ;
#25313 = ORIENTED_EDGE('',*,*,#17629,.F.) ;
#25314 = ORIENTED_EDGE('',*,*,#18043,.T.) ;
#25315 = ORIENTED_EDGE('',*,*,#18044,.F.) ;
#25316 = ORIENTED_EDGE('',*,*,#17630,.F.) ;
#25317 = ORIENTED_EDGE('',*,*,#18045,.F.) ;
#25318 = ORIENTED_EDGE('',*,*,#18043,.F.) ;
#25319 = ORIENTED_EDGE('',*,*,#17628,.F.) ;
#25320 = ORIENTED_EDGE('',*,*,#18044,.T.) ;
#25321 = ORIENTED_EDGE('',*,*,#18045,.T.) ;
#25322 = ORIENTED_EDGE('',*,*,#17632,.F.) ;
#25323 = ORIENTED_EDGE('',*,*,#18046,.T.) ;
#25324 = ORIENTED_EDGE('',*,*,#18047,.F.) ;
#25325 = ORIENTED_EDGE('',*,*,#17633,.F.) ;
#25326 = ORIENTED_EDGE('',*,*,#18048,.F.) ;
#25327 = ORIENTED_EDGE('',*,*,#18046,.F.) ;
#25328 = ORIENTED_EDGE('',*,*,#17631,.F.) ;
#25329 = ORIENTED_EDGE('',*,*,#18047,.T.) ;
#25330 = ORIENTED_EDGE('',*,*,#18048,.T.) ;
#25331 = ORIENTED_EDGE('',*,*,#17635,.F.) ;
#25332 = ORIENTED_EDGE('',*,*,#18049,.T.) ;
#25333 = ORIENTED_EDGE('',*,*,#18050,.F.) ;
#25334 = ORIENTED_EDGE('',*,*,#17636,.F.) ;
#25335 = ORIENTED_EDGE('',*,*,#18051,.F.) ;
#25336 = ORIENTED_EDGE('',*,*,#18049,.F.) ;
#25337 = ORIENTED_EDGE('',*,*,#17634,.F.) ;
#25338 = ORIENTED_EDGE('',*,*,#18050,.T.) ;
#25339 = ORIENTED_EDGE('',*,*,#18051,.T.) ;
#25340 = ORIENTED_EDGE('',*,*,#17640,.F.) ;
#25341 = ORIENTED_EDGE('',*,*,#18052,.T.) ;
#25342 = ORIENTED_EDGE('',*,*,#18053,.F.) ;
#25343 = ORIENTED_EDGE('',*,*,#17641,.F.) ;
#25344 = ORIENTED_EDGE('',*,*,#18054,.F.) ;
#25345 = ORIENTED_EDGE('',*,*,#18052,.F.) ;
#25346 = ORIENTED_EDGE('',*,*,#17639,.F.) ;
#25347 = ORIENTED_EDGE('',*,*,#17637,.F.) ;
#25348 = ORIENTED_EDGE('',*,*,#18053,.T.) ;
#25349 = ORIENTED_EDGE('',*,*,#18054,.T.) ;
#25350 = ORIENTED_EDGE('',*,*,#17643,.F.) ;
#25351 = ORIENTED_EDGE('',*,*,#18055,.T.) ;
#25352 = ORIENTED_EDGE('',*,*,#18056,.F.) ;
#25353 = ORIENTED_EDGE('',*,*,#17644,.F.) ;
#25354 = ORIENTED_EDGE('',*,*,#18057,.F.) ;
#25355 = ORIENTED_EDGE('',*,*,#18055,.F.) ;
#25356 = ORIENTED_EDGE('',*,*,#17642,.F.) ;
#25357 = ORIENTED_EDGE('',*,*,#18056,.T.) ;
#25358 = ORIENTED_EDGE('',*,*,#18057,.T.) ;
#25359 = ORIENTED_EDGE('',*,*,#17646,.F.) ;
#25360 = ORIENTED_EDGE('',*,*,#18058,.T.) ;
#25361 = ORIENTED_EDGE('',*,*,#18059,.F.) ;
#25362 = ORIENTED_EDGE('',*,*,#17647,.F.) ;
#25363 = ORIENTED_EDGE('',*,*,#18060,.F.) ;
#25364 = ORIENTED_EDGE('',*,*,#18058,.F.) ;
#25365 = ORIENTED_EDGE('',*,*,#17645,.F.) ;
#25366 = ORIENTED_EDGE('',*,*,#18059,.T.) ;
#25367 = ORIENTED_EDGE('',*,*,#18060,.T.) ;
#25368 = ORIENTED_EDGE('',*,*,#17649,.F.) ;
#25369 = ORIENTED_EDGE('',*,*,#18061,.T.) ;
#25370 = ORIENTED_EDGE('',*,*,#18062,.F.) ;
#25371 = ORIENTED_EDGE('',*,*,#17650,.F.) ;
#25372 = ORIENTED_EDGE('',*,*,#18063,.F.) ;
#25373 = ORIENTED_EDGE('',*,*,#18061,.F.) ;
#25374 = ORIENTED_EDGE('',*,*,#17648,.F.) ;
#25375 = ORIENTED_EDGE('',*,*,#18062,.T.) ;
#25376 = ORIENTED_EDGE('',*,*,#18063,.T.) ;
#25377 = ORIENTED_EDGE('',*,*,#17654,.F.) ;
#25378 = ORIENTED_EDGE('',*,*,#18064,.T.) ;
#25379 = ORIENTED_EDGE('',*,*,#18065,.F.) ;
#25380 = ORIENTED_EDGE('',*,*,#17655,.F.) ;
#25381 = ORIENTED_EDGE('',*,*,#18066,.F.) ;
#25382 = ORIENTED_EDGE('',*,*,#18064,.F.) ;
#25383 = ORIENTED_EDGE('',*,*,#17653,.F.) ;
#25384 = ORIENTED_EDGE('',*,*,#17651,.F.) ;
#25385 = ORIENTED_EDGE('',*,*,#18065,.T.) ;
#25386 = ORIENTED_EDGE('',*,*,#18066,.T.) ;
#25387 = ORIENTED_EDGE('',*,*,#17657,.F.) ;
#25388 = ORIENTED_EDGE('',*,*,#18067,.T.) ;
#25389 = ORIENTED_EDGE('',*,*,#18068,.F.) ;
#25390 = ORIENTED_EDGE('',*,*,#17658,.F.) ;
#25391 = ORIENTED_EDGE('',*,*,#18069,.F.) ;
#25392 = ORIENTED_EDGE('',*,*,#18067,.F.) ;
#25393 = ORIENTED_EDGE('',*,*,#17656,.F.) ;
#25394 = ORIENTED_EDGE('',*,*,#18068,.T.) ;
#25395 = ORIENTED_EDGE('',*,*,#18069,.T.) ;
#25396 = ORIENTED_EDGE('',*,*,#17660,.F.) ;
#25397 = ORIENTED_EDGE('',*,*,#18070,.T.) ;
#25398 = ORIENTED_EDGE('',*,*,#18071,.F.) ;
#25399 = ORIENTED_EDGE('',*,*,#17661,.F.) ;
#25400 = ORIENTED_EDGE('',*,*,#18072,.F.) ;
#25401 = ORIENTED_EDGE('',*,*,#18070,.F.) ;
#25402 = ORIENTED_EDGE('',*,*,#17659,.F.) ;
#25403 = ORIENTED_EDGE('',*,*,#18071,.T.) ;
#25404 = ORIENTED_EDGE('',*,*,#18072,.T.) ;
#25405 = ORIENTED_EDGE('',*,*,#17663,.F.) ;
#25406 = ORIENTED_EDGE('',*,*,#18073,.T.) ;
#25407 = ORIENTED_EDGE('',*,*,#18074,.F.) ;
#25408 = ORIENTED_EDGE('',*,*,#17664,.F.) ;
#25409 = ORIENTED_EDGE('',*,*,#18075,.F.) ;
#25410 = ORIENTED_EDGE('',*,*,#18073,.F.) ;
#25411 = ORIENTED_EDGE('',*,*,#17662,.F.) ;
#25412 = ORIENTED_EDGE('',*,*,#18074,.T.) ;
#25413 = ORIENTED_EDGE('',*,*,#18075,.T.) ;
#25414 = ORIENTED_EDGE('',*,*,#17668,.F.) ;
#25415 = ORIENTED_EDGE('',*,*,#18076,.T.) ;
#25416 = ORIENTED_EDGE('',*,*,#18077,.F.) ;
#25417 = ORIENTED_EDGE('',*,*,#17669,.F.) ;
#25418 = ORIENTED_EDGE('',*,*,#18078,.F.) ;
#25419 = ORIENTED_EDGE('',*,*,#18076,.F.) ;
#25420 = ORIENTED_EDGE('',*,*,#17667,.F.) ;
#25421 = ORIENTED_EDGE('',*,*,#17665,.F.) ;
#25422 = ORIENTED_EDGE('',*,*,#18077,.T.) ;
#25423 = ORIENTED_EDGE('',*,*,#18078,.T.) ;
#25424 = ORIENTED_EDGE('',*,*,#17671,.F.) ;
#25425 = ORIENTED_EDGE('',*,*,#18079,.T.) ;
#25426 = ORIENTED_EDGE('',*,*,#18080,.F.) ;
#25427 = ORIENTED_EDGE('',*,*,#17672,.F.) ;
#25428 = ORIENTED_EDGE('',*,*,#18081,.F.) ;
#25429 = ORIENTED_EDGE('',*,*,#18079,.F.) ;
#25430 = ORIENTED_EDGE('',*,*,#17670,.F.) ;
#25431 = ORIENTED_EDGE('',*,*,#18080,.T.) ;
#25432 = ORIENTED_EDGE('',*,*,#18081,.T.) ;
#25433 = ORIENTED_EDGE('',*,*,#17674,.F.) ;
#25434 = ORIENTED_EDGE('',*,*,#18082,.T.) ;
#25435 = ORIENTED_EDGE('',*,*,#18083,.F.) ;
#25436 = ORIENTED_EDGE('',*,*,#17675,.F.) ;
#25437 = ORIENTED_EDGE('',*,*,#18084,.F.) ;
#25438 = ORIENTED_EDGE('',*,*,#18082,.F.) ;
#25439 = ORIENTED_EDGE('',*,*,#17673,.F.) ;
#25440 = ORIENTED_EDGE('',*,*,#18083,.T.) ;
#25441 = ORIENTED_EDGE('',*,*,#18084,.T.) ;
#25442 = ORIENTED_EDGE('',*,*,#17677,.F.) ;
#25443 = ORIENTED_EDGE('',*,*,#18085,.T.) ;
#25444 = ORIENTED_EDGE('',*,*,#18086,.F.) ;
#25445 = ORIENTED_EDGE('',*,*,#17678,.F.) ;
#25446 = ORIENTED_EDGE('',*,*,#18087,.F.) ;
#25447 = ORIENTED_EDGE('',*,*,#18085,.F.) ;
#25448 = ORIENTED_EDGE('',*,*,#17676,.F.) ;
#25449 = ORIENTED_EDGE('',*,*,#18086,.T.) ;
#25450 = ORIENTED_EDGE('',*,*,#18087,.T.) ;
#25451 = ORIENTED_EDGE('',*,*,#17682,.F.) ;
#25452 = ORIENTED_EDGE('',*,*,#18088,.T.) ;
#25453 = ORIENTED_EDGE('',*,*,#18089,.F.) ;
#25454 = ORIENTED_EDGE('',*,*,#17683,.F.) ;
#25455 = ORIENTED_EDGE('',*,*,#18090,.F.) ;
#25456 = ORIENTED_EDGE('',*,*,#18088,.F.) ;
#25457 = ORIENTED_EDGE('',*,*,#17681,.F.) ;
#25458 = ORIENTED_EDGE('',*,*,#17679,.F.) ;
#25459 = ORIENTED_EDGE('',*,*,#18089,.T.) ;
#25460 = ORIENTED_EDGE('',*,*,#18090,.T.) ;
#25461 = ORIENTED_EDGE('',*,*,#17685,.F.) ;
#25462 = ORIENTED_EDGE('',*,*,#18091,.T.) ;
#25463 = ORIENTED_EDGE('',*,*,#18092,.F.) ;
#25464 = ORIENTED_EDGE('',*,*,#17686,.F.) ;
#25465 = ORIENTED_EDGE('',*,*,#18093,.F.) ;
#25466 = ORIENTED_EDGE('',*,*,#18091,.F.) ;
#25467 = ORIENTED_EDGE('',*,*,#17684,.F.) ;
#25468 = ORIENTED_EDGE('',*,*,#18092,.T.) ;
#25469 = ORIENTED_EDGE('',*,*,#18093,.T.) ;
#25470 = ORIENTED_EDGE('',*,*,#17688,.F.) ;
#25471 = ORIENTED_EDGE('',*,*,#18094,.T.) ;
#25472 = ORIENTED_EDGE('',*,*,#18095,.F.) ;
#25473 = ORIENTED_EDGE('',*,*,#17689,.F.) ;
#25474 = ORIENTED_EDGE('',*,*,#18096,.F.) ;
#25475 = ORIENTED_EDGE('',*,*,#18094,.F.) ;
#25476 = ORIENTED_EDGE('',*,*,#17687,.F.) ;
#25477 = ORIENTED_EDGE('',*,*,#18095,.T.) ;
#25478 = ORIENTED_EDGE('',*,*,#18096,.T.) ;
#25479 = ORIENTED_EDGE('',*,*,#17691,.F.) ;
#25480 = ORIENTED_EDGE('',*,*,#18097,.T.) ;
#25481 = ORIENTED_EDGE('',*,*,#18098,.F.) ;
#25482 = ORIENTED_EDGE('',*,*,#17692,.F.) ;
#25483 = ORIENTED_EDGE('',*,*,#18099,.F.) ;
#25484 = ORIENTED_EDGE('',*,*,#18097,.F.) ;
#25485 = ORIENTED_EDGE('',*,*,#17690,.F.) ;
#25486 = ORIENTED_EDGE('',*,*,#18098,.T.) ;
#25487 = ORIENTED_EDGE('',*,*,#18099,.T.) ;
#25488 = ORIENTED_EDGE('',*,*,#17696,.F.) ;
#25489 = ORIENTED_EDGE('',*,*,#18100,.T.) ;
#25490 = ORIENTED_EDGE('',*,*,#18101,.F.) ;
#25491 = ORIENTED_EDGE('',*,*,#17697,.F.) ;
#25492 = ORIENTED_EDGE('',*,*,#18102,.F.) ;
#25493 = ORIENTED_EDGE('',*,*,#18100,.F.) ;
#25494 = ORIENTED_EDGE('',*,*,#17695,.F.) ;
#25495 = ORIENTED_EDGE('',*,*,#17693,.F.) ;
#25496 = ORIENTED_EDGE('',*,*,#18101,.T.) ;
#25497 = ORIENTED_EDGE('',*,*,#18102,.T.) ;
#25498 = ORIENTED_EDGE('',*,*,#17699,.F.) ;
#25499 = ORIENTED_EDGE('',*,*,#18103,.T.) ;
#25500 = ORIENTED_EDGE('',*,*,#18104,.F.) ;
#25501 = ORIENTED_EDGE('',*,*,#17700,.F.) ;
#25502 = ORIENTED_EDGE('',*,*,#18105,.F.) ;
#25503 = ORIENTED_EDGE('',*,*,#18103,.F.) ;
#25504 = ORIENTED_EDGE('',*,*,#17698,.F.) ;
#25505 = ORIENTED_EDGE('',*,*,#18104,.T.) ;
#25506 = ORIENTED_EDGE('',*,*,#18105,.T.) ;
#25507 = ORIENTED_EDGE('',*,*,#17702,.F.) ;
#25508 = ORIENTED_EDGE('',*,*,#18106,.T.) ;
#25509 = ORIENTED_EDGE('',*,*,#18107,.F.) ;
#25510 = ORIENTED_EDGE('',*,*,#17703,.F.) ;
#25511 = ORIENTED_EDGE('',*,*,#18108,.F.) ;
#25512 = ORIENTED_EDGE('',*,*,#18106,.F.) ;
#25513 = ORIENTED_EDGE('',*,*,#17701,.F.) ;
#25514 = ORIENTED_EDGE('',*,*,#18107,.T.) ;
#25515 = ORIENTED_EDGE('',*,*,#18108,.T.) ;
#25516 = ORIENTED_EDGE('',*,*,#17705,.F.) ;
#25517 = ORIENTED_EDGE('',*,*,#18109,.T.) ;
#25518 = ORIENTED_EDGE('',*,*,#18110,.F.) ;
#25519 = ORIENTED_EDGE('',*,*,#17706,.F.) ;
#25520 = ORIENTED_EDGE('',*,*,#18111,.F.) ;
#25521 = ORIENTED_EDGE('',*,*,#18109,.F.) ;
#25522 = ORIENTED_EDGE('',*,*,#17704,.F.) ;
#25523 = ORIENTED_EDGE('',*,*,#18110,.T.) ;
#25524 = ORIENTED_EDGE('',*,*,#18111,.T.) ;
#25525 = ORIENTED_EDGE('',*,*,#17710,.F.) ;
#25526 = ORIENTED_EDGE('',*,*,#18112,.T.) ;
#25527 = ORIENTED_EDGE('',*,*,#18113,.F.) ;
#25528 = ORIENTED_EDGE('',*,*,#17711,.F.) ;
#25529 = ORIENTED_EDGE('',*,*,#18114,.F.) ;
#25530 = ORIENTED_EDGE('',*,*,#18112,.F.) ;
#25531 = ORIENTED_EDGE('',*,*,#17709,.F.) ;
#25532 = ORIENTED_EDGE('',*,*,#17707,.F.) ;
#25533 = ORIENTED_EDGE('',*,*,#18113,.T.) ;
#25534 = ORIENTED_EDGE('',*,*,#18114,.T.) ;
#25535 = ORIENTED_EDGE('',*,*,#17713,.F.) ;
#25536 = ORIENTED_EDGE('',*,*,#18115,.T.) ;
#25537 = ORIENTED_EDGE('',*,*,#18116,.F.) ;
#25538 = ORIENTED_EDGE('',*,*,#17714,.F.) ;
#25539 = ORIENTED_EDGE('',*,*,#18117,.F.) ;
#25540 = ORIENTED_EDGE('',*,*,#18115,.F.) ;
#25541 = ORIENTED_EDGE('',*,*,#17712,.F.) ;
#25542 = ORIENTED_EDGE('',*,*,#18116,.T.) ;
#25543 = ORIENTED_EDGE('',*,*,#18117,.T.) ;
#25544 = ORIENTED_EDGE('',*,*,#17716,.F.) ;
#25545 = ORIENTED_EDGE('',*,*,#18118,.T.) ;
#25546 = ORIENTED_EDGE('',*,*,#18119,.F.) ;
#25547 = ORIENTED_EDGE('',*,*,#17717,.F.) ;
#25548 = ORIENTED_EDGE('',*,*,#18120,.F.) ;
#25549 = ORIENTED_EDGE('',*,*,#18118,.F.) ;
#25550 = ORIENTED_EDGE('',*,*,#17715,.F.) ;
#25551 = ORIENTED_EDGE('',*,*,#18119,.T.) ;
#25552 = ORIENTED_EDGE('',*,*,#18120,.T.) ;
#25553 = ORIENTED_EDGE('',*,*,#17719,.F.) ;
#25554 = ORIENTED_EDGE('',*,*,#18121,.T.) ;
#25555 = ORIENTED_EDGE('',*,*,#18122,.F.) ;
#25556 = ORIENTED_EDGE('',*,*,#17720,.F.) ;
#25557 = ORIENTED_EDGE('',*,*,#18123,.F.) ;
#25558 = ORIENTED_EDGE('',*,*,#18121,.F.) ;
#25559 = ORIENTED_EDGE('',*,*,#17718,.F.) ;
#25560 = ORIENTED_EDGE('',*,*,#18122,.T.) ;
#25561 = ORIENTED_EDGE('',*,*,#18123,.T.) ;
#25562 = ORIENTED_EDGE('',*,*,#17724,.F.) ;
#25563 = ORIENTED_EDGE('',*,*,#18124,.T.) ;
#25564 = ORIENTED_EDGE('',*,*,#18125,.F.) ;
#25565 = ORIENTED_EDGE('',*,*,#17725,.F.) ;
#25566 = ORIENTED_EDGE('',*,*,#18126,.F.) ;
#25567 = ORIENTED_EDGE('',*,*,#18124,.F.) ;
#25568 = ORIENTED_EDGE('',*,*,#17723,.F.) ;
#25569 = ORIENTED_EDGE('',*,*,#17721,.F.) ;
#25570 = ORIENTED_EDGE('',*,*,#18125,.T.) ;
#25571 = ORIENTED_EDGE('',*,*,#18126,.T.) ;
#25572 = ORIENTED_EDGE('',*,*,#17727,.F.) ;
#25573 = ORIENTED_EDGE('',*,*,#18127,.T.) ;
#25574 = ORIENTED_EDGE('',*,*,#18128,.F.) ;
#25575 = ORIENTED_EDGE('',*,*,#17728,.F.) ;
#25576 = ORIENTED_EDGE('',*,*,#18129,.F.) ;
#25577 = ORIENTED_EDGE('',*,*,#18127,.F.) ;
#25578 = ORIENTED_EDGE('',*,*,#17726,.F.) ;
#25579 = ORIENTED_EDGE('',*,*,#18128,.T.) ;
#25580 = ORIENTED_EDGE('',*,*,#18129,.T.) ;
#25581 = ORIENTED_EDGE('',*,*,#17730,.F.) ;
#25582 = ORIENTED_EDGE('',*,*,#18130,.T.) ;
#25583 = ORIENTED_EDGE('',*,*,#18131,.F.) ;
#25584 = ORIENTED_EDGE('',*,*,#17731,.F.) ;
#25585 = ORIENTED_EDGE('',*,*,#18132,.F.) ;
#25586 = ORIENTED_EDGE('',*,*,#18130,.F.) ;
#25587 = ORIENTED_EDGE('',*,*,#17729,.F.) ;
#25588 = ORIENTED_EDGE('',*,*,#18131,.T.) ;
#25589 = ORIENTED_EDGE('',*,*,#18132,.T.) ;
#25590 = ORIENTED_EDGE('',*,*,#17733,.F.) ;
#25591 = ORIENTED_EDGE('',*,*,#18133,.T.) ;
#25592 = ORIENTED_EDGE('',*,*,#18134,.F.) ;
#25593 = ORIENTED_EDGE('',*,*,#17734,.F.) ;
#25594 = ORIENTED_EDGE('',*,*,#18135,.F.) ;
#25595 = ORIENTED_EDGE('',*,*,#18133,.F.) ;
#25596 = ORIENTED_EDGE('',*,*,#17732,.F.) ;
#25597 = ORIENTED_EDGE('',*,*,#18134,.T.) ;
#25598 = ORIENTED_EDGE('',*,*,#18135,.T.) ;
#25599 = ORIENTED_EDGE('',*,*,#17738,.F.) ;
#25600 = ORIENTED_EDGE('',*,*,#18136,.T.) ;
#25601 = ORIENTED_EDGE('',*,*,#18137,.F.) ;
#25602 = ORIENTED_EDGE('',*,*,#17739,.F.) ;
#25603 = ORIENTED_EDGE('',*,*,#18138,.F.) ;
#25604 = ORIENTED_EDGE('',*,*,#18136,.F.) ;
#25605 = ORIENTED_EDGE('',*,*,#17737,.F.) ;
#25606 = ORIENTED_EDGE('',*,*,#17735,.F.) ;
#25607 = ORIENTED_EDGE('',*,*,#18137,.T.) ;
#25608 = ORIENTED_EDGE('',*,*,#18138,.T.) ;
#25609 = ORIENTED_EDGE('',*,*,#17741,.F.) ;
#25610 = ORIENTED_EDGE('',*,*,#18139,.T.) ;
#25611 = ORIENTED_EDGE('',*,*,#18140,.F.) ;
#25612 = ORIENTED_EDGE('',*,*,#17742,.F.) ;
#25613 = ORIENTED_EDGE('',*,*,#18141,.F.) ;
#25614 = ORIENTED_EDGE('',*,*,#18139,.F.) ;
#25615 = ORIENTED_EDGE('',*,*,#17740,.F.) ;
#25616 = ORIENTED_EDGE('',*,*,#18140,.T.) ;
#25617 = ORIENTED_EDGE('',*,*,#18141,.T.) ;
#25618 = ORIENTED_EDGE('',*,*,#17744,.F.) ;
#25619 = ORIENTED_EDGE('',*,*,#18142,.T.) ;
#25620 = ORIENTED_EDGE('',*,*,#18143,.F.) ;
#25621 = ORIENTED_EDGE('',*,*,#17745,.F.) ;
#25622 = ORIENTED_EDGE('',*,*,#18144,.F.) ;
#25623 = ORIENTED_EDGE('',*,*,#18142,.F.) ;
#25624 = ORIENTED_EDGE('',*,*,#17743,.F.) ;
#25625 = ORIENTED_EDGE('',*,*,#18143,.T.) ;
#25626 = ORIENTED_EDGE('',*,*,#18144,.T.) ;
#25627 = ORIENTED_EDGE('',*,*,#17747,.F.) ;
#25628 = ORIENTED_EDGE('',*,*,#18145,.T.) ;
#25629 = ORIENTED_EDGE('',*,*,#18146,.F.) ;
#25630 = ORIENTED_EDGE('',*,*,#17748,.F.) ;
#25631 = ORIENTED_EDGE('',*,*,#18147,.F.) ;
#25632 = ORIENTED_EDGE('',*,*,#18145,.F.) ;
#25633 = ORIENTED_EDGE('',*,*,#17746,.F.) ;
#25634 = ORIENTED_EDGE('',*,*,#18146,.T.) ;
#25635 = ORIENTED_EDGE('',*,*,#18147,.T.) ;
#25636 = ORIENTED_EDGE('',*,*,#17752,.F.) ;
#25637 = ORIENTED_EDGE('',*,*,#18148,.T.) ;
#25638 = ORIENTED_EDGE('',*,*,#18149,.F.) ;
#25639 = ORIENTED_EDGE('',*,*,#17753,.F.) ;
#25640 = ORIENTED_EDGE('',*,*,#18150,.F.) ;
#25641 = ORIENTED_EDGE('',*,*,#18148,.F.) ;
#25642 = ORIENTED_EDGE('',*,*,#17751,.F.) ;
#25643 = ORIENTED_EDGE('',*,*,#17749,.F.) ;
#25644 = ORIENTED_EDGE('',*,*,#18149,.T.) ;
#25645 = ORIENTED_EDGE('',*,*,#18150,.T.) ;
#25646 = ORIENTED_EDGE('',*,*,#17755,.F.) ;
#25647 = ORIENTED_EDGE('',*,*,#18151,.T.) ;
#25648 = ORIENTED_EDGE('',*,*,#18152,.F.) ;
#25649 = ORIENTED_EDGE('',*,*,#17756,.F.) ;
#25650 = ORIENTED_EDGE('',*,*,#18153,.F.) ;
#25651 = ORIENTED_EDGE('',*,*,#18151,.F.) ;
#25652 = ORIENTED_EDGE('',*,*,#17754,.F.) ;
#25653 = ORIENTED_EDGE('',*,*,#18152,.T.) ;
#25654 = ORIENTED_EDGE('',*,*,#18153,.T.) ;
#25655 = ORIENTED_EDGE('',*,*,#17758,.F.) ;
#25656 = ORIENTED_EDGE('',*,*,#18154,.T.) ;
#25657 = ORIENTED_EDGE('',*,*,#18155,.F.) ;
#25658 = ORIENTED_EDGE('',*,*,#17759,.F.) ;
#25659 = ORIENTED_EDGE('',*,*,#18156,.F.) ;
#25660 = ORIENTED_EDGE('',*,*,#18154,.F.) ;
#25661 = ORIENTED_EDGE('',*,*,#17757,.F.) ;
#25662 = ORIENTED_EDGE('',*,*,#18155,.T.) ;
#25663 = ORIENTED_EDGE('',*,*,#18156,.T.) ;
#25664 = ORIENTED_EDGE('',*,*,#17761,.F.) ;
#25665 = ORIENTED_EDGE('',*,*,#18157,.T.) ;
#25666 = ORIENTED_EDGE('',*,*,#18158,.F.) ;
#25667 = ORIENTED_EDGE('',*,*,#17762,.F.) ;
#25668 = ORIENTED_EDGE('',*,*,#18159,.F.) ;
#25669 = ORIENTED_EDGE('',*,*,#18157,.F.) ;
#25670 = ORIENTED_EDGE('',*,*,#17760,.F.) ;
#25671 = ORIENTED_EDGE('',*,*,#18158,.T.) ;
#25672 = ORIENTED_EDGE('',*,*,#18159,.T.) ;
#25673 = ORIENTED_EDGE('',*,*,#17766,.F.) ;
#25674 = ORIENTED_EDGE('',*,*,#18160,.T.) ;
#25675 = ORIENTED_EDGE('',*,*,#18161,.F.) ;
#25676 = ORIENTED_EDGE('',*,*,#17767,.F.) ;
#25677 = ORIENTED_EDGE('',*,*,#18162,.F.) ;
#25678 = ORIENTED_EDGE('',*,*,#18160,.F.) ;
#25679 = ORIENTED_EDGE('',*,*,#17765,.F.) ;
#25680 = ORIENTED_EDGE('',*,*,#17763,.F.) ;
#25681 = ORIENTED_EDGE('',*,*,#18161,.T.) ;
#25682 = ORIENTED_EDGE('',*,*,#18162,.T.) ;
#25683 = ORIENTED_EDGE('',*,*,#17769,.F.) ;
#25684 = ORIENTED_EDGE('',*,*,#18163,.T.) ;
#25685 = ORIENTED_EDGE('',*,*,#18164,.F.) ;
#25686 = ORIENTED_EDGE('',*,*,#17770,.F.) ;
#25687 = ORIENTED_EDGE('',*,*,#18165,.F.) ;
#25688 = ORIENTED_EDGE('',*,*,#18163,.F.) ;
#25689 = ORIENTED_EDGE('',*,*,#17768,.F.) ;
#25690 = ORIENTED_EDGE('',*,*,#18164,.T.) ;
#25691 = ORIENTED_EDGE('',*,*,#18165,.T.) ;
#25692 = ORIENTED_EDGE('',*,*,#17772,.F.) ;
#25693 = ORIENTED_EDGE('',*,*,#18166,.T.) ;
#25694 = ORIENTED_EDGE('',*,*,#18167,.F.) ;
#25695 = ORIENTED_EDGE('',*,*,#17773,.F.) ;
#25696 = ORIENTED_EDGE('',*,*,#18168,.F.) ;
#25697 = ORIENTED_EDGE('',*,*,#18166,.F.) ;
#25698 = ORIENTED_EDGE('',*,*,#17771,.F.) ;
#25699 = ORIENTED_EDGE('',*,*,#18167,.T.) ;
#25700 = ORIENTED_EDGE('',*,*,#18168,.T.) ;
#25701 = ORIENTED_EDGE('',*,*,#17775,.F.) ;
#25702 = ORIENTED_EDGE('',*,*,#18169,.T.) ;
#25703 = ORIENTED_EDGE('',*,*,#18170,.F.) ;
#25704 = ORIENTED_EDGE('',*,*,#17776,.F.) ;
#25705 = ORIENTED_EDGE('',*,*,#18171,.F.) ;
#25706 = ORIENTED_EDGE('',*,*,#18169,.F.) ;
#25707 = ORIENTED_EDGE('',*,*,#17774,.F.) ;
#25708 = ORIENTED_EDGE('',*,*,#18170,.T.) ;
#25709 = ORIENTED_EDGE('',*,*,#18171,.T.) ;
#25710 = ORIENTED_EDGE('',*,*,#17780,.F.) ;
#25711 = ORIENTED_EDGE('',*,*,#18172,.T.) ;
#25712 = ORIENTED_EDGE('',*,*,#18173,.F.) ;
#25713 = ORIENTED_EDGE('',*,*,#17781,.F.) ;
#25714 = ORIENTED_EDGE('',*,*,#18174,.F.) ;
#25715 = ORIENTED_EDGE('',*,*,#18172,.F.) ;
#25716 = ORIENTED_EDGE('',*,*,#17779,.F.) ;
#25717 = ORIENTED_EDGE('',*,*,#17777,.F.) ;
#25718 = ORIENTED_EDGE('',*,*,#18173,.T.) ;
#25719 = ORIENTED_EDGE('',*,*,#18174,.T.) ;
#25720 = ORIENTED_EDGE('',*,*,#17783,.F.) ;
#25721 = ORIENTED_EDGE('',*,*,#18175,.T.) ;
#25722 = ORIENTED_EDGE('',*,*,#18176,.F.) ;
#25723 = ORIENTED_EDGE('',*,*,#17784,.F.) ;
#25724 = ORIENTED_EDGE('',*,*,#18177,.F.) ;
#25725 = ORIENTED_EDGE('',*,*,#18175,.F.) ;
#25726 = ORIENTED_EDGE('',*,*,#17782,.F.) ;
#25727 = ORIENTED_EDGE('',*,*,#18176,.T.) ;
#25728 = ORIENTED_EDGE('',*,*,#18177,.T.) ;
#25729 = ORIENTED_EDGE('',*,*,#17786,.F.) ;
#25730 = ORIENTED_EDGE('',*,*,#18178,.T.) ;
#25731 = ORIENTED_EDGE('',*,*,#18179,.F.) ;
#25732 = ORIENTED_EDGE('',*,*,#17787,.F.) ;
#25733 = ORIENTED_EDGE('',*,*,#18180,.F.) ;
#25734 = ORIENTED_EDGE('',*,*,#18178,.F.) ;
#25735 = ORIENTED_EDGE('',*,*,#17785,.F.) ;
#25736 = ORIENTED_EDGE('',*,*,#18179,.T.) ;
#25737 = ORIENTED_EDGE('',*,*,#18180,.T.) ;
#25738 = ORIENTED_EDGE('',*,*,#17789,.F.) ;
#25739 = ORIENTED_EDGE('',*,*,#18181,.T.) ;
#25740 = ORIENTED_EDGE('',*,*,#18182,.F.) ;
#25741 = ORIENTED_EDGE('',*,*,#17790,.F.) ;
#25742 = ORIENTED_EDGE('',*,*,#18183,.F.) ;
#25743 = ORIENTED_EDGE('',*,*,#18181,.F.) ;
#25744 = ORIENTED_EDGE('',*,*,#17788,.F.) ;
#25745 = ORIENTED_EDGE('',*,*,#18182,.T.) ;
#25746 = ORIENTED_EDGE('',*,*,#18183,.T.) ;
#25747 = ORIENTED_EDGE('',*,*,#17794,.F.) ;
#25748 = ORIENTED_EDGE('',*,*,#18184,.T.) ;
#25749 = ORIENTED_EDGE('',*,*,#18185,.F.) ;
#25750 = ORIENTED_EDGE('',*,*,#17795,.F.) ;
#25751 = ORIENTED_EDGE('',*,*,#18186,.F.) ;
#25752 = ORIENTED_EDGE('',*,*,#18184,.F.) ;
#25753 = ORIENTED_EDGE('',*,*,#17793,.F.) ;
#25754 = ORIENTED_EDGE('',*,*,#17791,.F.) ;
#25755 = ORIENTED_EDGE('',*,*,#18185,.T.) ;
#25756 = ORIENTED_EDGE('',*,*,#18186,.T.) ;
#25757 = ORIENTED_EDGE('',*,*,#17797,.F.) ;
#25758 = ORIENTED_EDGE('',*,*,#18187,.T.) ;
#25759 = ORIENTED_EDGE('',*,*,#18188,.F.) ;
#25760 = ORIENTED_EDGE('',*,*,#17798,.F.) ;
#25761 = ORIENTED_EDGE('',*,*,#18189,.F.) ;
#25762 = ORIENTED_EDGE('',*,*,#18187,.F.) ;
#25763 = ORIENTED_EDGE('',*,*,#17796,.F.) ;
#25764 = ORIENTED_EDGE('',*,*,#18188,.T.) ;
#25765 = ORIENTED_EDGE('',*,*,#18189,.T.) ;
#25766 = ORIENTED_EDGE('',*,*,#17800,.F.) ;
#25767 = ORIENTED_EDGE('',*,*,#18190,.T.) ;
#25768 = ORIENTED_EDGE('',*,*,#18191,.F.) ;
#25769 = ORIENTED_EDGE('',*,*,#17801,.F.) ;
#25770 = ORIENTED_EDGE('',*,*,#18192,.F.) ;
#25771 = ORIENTED_EDGE('',*,*,#18190,.F.) ;
#25772 = ORIENTED_EDGE('',*,*,#17799,.F.) ;
#25773 = ORIENTED_EDGE('',*,*,#18191,.T.) ;
#25774 = ORIENTED_EDGE('',*,*,#18192,.T.) ;
#25775 = ORIENTED_EDGE('',*,*,#17803,.F.) ;
#25776 = ORIENTED_EDGE('',*,*,#18193,.T.) ;
#25777 = ORIENTED_EDGE('',*,*,#18194,.F.) ;
#25778 = ORIENTED_EDGE('',*,*,#17804,.F.) ;
#25779 = ORIENTED_EDGE('',*,*,#18195,.F.) ;
#25780 = ORIENTED_EDGE('',*,*,#18193,.F.) ;
#25781 = ORIENTED_EDGE('',*,*,#17802,.F.) ;
#25782 = ORIENTED_EDGE('',*,*,#18194,.T.) ;
#25783 = ORIENTED_EDGE('',*,*,#18195,.T.) ;
#25784 = ORIENTED_EDGE('',*,*,#17808,.F.) ;
#25785 = ORIENTED_EDGE('',*,*,#18196,.T.) ;
#25786 = ORIENTED_EDGE('',*,*,#18197,.F.) ;
#25787 = ORIENTED_EDGE('',*,*,#17809,.F.) ;
#25788 = ORIENTED_EDGE('',*,*,#18198,.F.) ;
#25789 = ORIENTED_EDGE('',*,*,#18196,.F.) ;
#25790 = ORIENTED_EDGE('',*,*,#17807,.F.) ;
#25791 = ORIENTED_EDGE('',*,*,#17805,.F.) ;
#25792 = ORIENTED_EDGE('',*,*,#18197,.T.) ;
#25793 = ORIENTED_EDGE('',*,*,#18198,.T.) ;
#25794 = ORIENTED_EDGE('',*,*,#17811,.F.) ;
#25795 = ORIENTED_EDGE('',*,*,#18199,.T.) ;
#25796 = ORIENTED_EDGE('',*,*,#18200,.F.) ;
#25797 = ORIENTED_EDGE('',*,*,#17812,.F.) ;
#25798 = ORIENTED_EDGE('',*,*,#18201,.F.) ;
#25799 = ORIENTED_EDGE('',*,*,#18199,.F.) ;
#25800 = ORIENTED_EDGE('',*,*,#17810,.F.) ;
#25801 = ORIENTED_EDGE('',*,*,#18200,.T.) ;
#25802 = ORIENTED_EDGE('',*,*,#18201,.T.) ;
#25803 = ORIENTED_EDGE('',*,*,#17814,.F.) ;
#25804 = ORIENTED_EDGE('',*,*,#18202,.T.) ;
#25805 = ORIENTED_EDGE('',*,*,#18203,.F.) ;
#25806 = ORIENTED_EDGE('',*,*,#17815,.F.) ;
#25807 = ORIENTED_EDGE('',*,*,#18204,.F.) ;
#25808 = ORIENTED_EDGE('',*,*,#18202,.F.) ;
#25809 = ORIENTED_EDGE('',*,*,#17813,.F.) ;
#25810 = ORIENTED_EDGE('',*,*,#18203,.T.) ;
#25811 = ORIENTED_EDGE('',*,*,#18204,.T.) ;
#25812 = ORIENTED_EDGE('',*,*,#17817,.F.) ;
#25813 = ORIENTED_EDGE('',*,*,#18205,.T.) ;
#25814 = ORIENTED_EDGE('',*,*,#18206,.F.) ;
#25815 = ORIENTED_EDGE('',*,*,#17818,.F.) ;
#25816 = ORIENTED_EDGE('',*,*,#18207,.F.) ;
#25817 = ORIENTED_EDGE('',*,*,#18205,.F.) ;
#25818 = ORIENTED_EDGE('',*,*,#17816,.F.) ;
#25819 = ORIENTED_EDGE('',*,*,#18206,.T.) ;
#25820 = ORIENTED_EDGE('',*,*,#18207,.T.) ;
#25821 = ORIENTED_EDGE('',*,*,#17822,.F.) ;
#25822 = ORIENTED_EDGE('',*,*,#18208,.T.) ;
#25823 = ORIENTED_EDGE('',*,*,#18209,.F.) ;
#25824 = ORIENTED_EDGE('',*,*,#17823,.F.) ;
#25825 = ORIENTED_EDGE('',*,*,#18210,.F.) ;
#25826 = ORIENTED_EDGE('',*,*,#18208,.F.) ;
#25827 = ORIENTED_EDGE('',*,*,#17821,.F.) ;
#25828 = ORIENTED_EDGE('',*,*,#17819,.F.) ;
#25829 = ORIENTED_EDGE('',*,*,#18209,.T.) ;
#25830 = ORIENTED_EDGE('',*,*,#18210,.T.) ;
#25831 = ORIENTED_EDGE('',*,*,#17825,.F.) ;
#25832 = ORIENTED_EDGE('',*,*,#18211,.T.) ;
#25833 = ORIENTED_EDGE('',*,*,#18212,.F.) ;
#25834 = ORIENTED_EDGE('',*,*,#17826,.F.) ;
#25835 = ORIENTED_EDGE('',*,*,#18213,.F.) ;
#25836 = ORIENTED_EDGE('',*,*,#18211,.F.) ;
#25837 = ORIENTED_EDGE('',*,*,#17824,.F.) ;
#25838 = ORIENTED_EDGE('',*,*,#18212,.T.) ;
#25839 = ORIENTED_EDGE('',*,*,#18213,.T.) ;
#25840 = ORIENTED_EDGE('',*,*,#17828,.F.) ;
#25841 = ORIENTED_EDGE('',*,*,#18214,.T.) ;
#25842 = ORIENTED_EDGE('',*,*,#18215,.F.) ;
#25843 = ORIENTED_EDGE('',*,*,#17829,.F.) ;
#25844 = ORIENTED_EDGE('',*,*,#18216,.F.) ;
#25845 = ORIENTED_EDGE('',*,*,#18214,.F.) ;
#25846 = ORIENTED_EDGE('',*,*,#17827,.F.) ;
#25847 = ORIENTED_EDGE('',*,*,#18215,.T.) ;
#25848 = ORIENTED_EDGE('',*,*,#18216,.T.) ;
#25849 = ORIENTED_EDGE('',*,*,#17831,.F.) ;
#25850 = ORIENTED_EDGE('',*,*,#18217,.T.) ;
#25851 = ORIENTED_EDGE('',*,*,#18218,.F.) ;
#25852 = ORIENTED_EDGE('',*,*,#17832,.F.) ;
#25853 = ORIENTED_EDGE('',*,*,#18219,.F.) ;
#25854 = ORIENTED_EDGE('',*,*,#18217,.F.) ;
#25855 = ORIENTED_EDGE('',*,*,#17830,.F.) ;
#25856 = ORIENTED_EDGE('',*,*,#18218,.T.) ;
#25857 = ORIENTED_EDGE('',*,*,#18219,.T.) ;
#25858 = ORIENTED_EDGE('',*,*,#17836,.F.) ;
#25859 = ORIENTED_EDGE('',*,*,#18220,.T.) ;
#25860 = ORIENTED_EDGE('',*,*,#18221,.F.) ;
#25861 = ORIENTED_EDGE('',*,*,#17837,.F.) ;
#25862 = ORIENTED_EDGE('',*,*,#18222,.F.) ;
#25863 = ORIENTED_EDGE('',*,*,#18220,.F.) ;
#25864 = ORIENTED_EDGE('',*,*,#17835,.F.) ;
#25865 = ORIENTED_EDGE('',*,*,#17833,.F.) ;
#25866 = ORIENTED_EDGE('',*,*,#18221,.T.) ;
#25867 = ORIENTED_EDGE('',*,*,#18222,.T.) ;
#25868 = ORIENTED_EDGE('',*,*,#17839,.F.) ;
#25869 = ORIENTED_EDGE('',*,*,#18223,.T.) ;
#25870 = ORIENTED_EDGE('',*,*,#18224,.F.) ;
#25871 = ORIENTED_EDGE('',*,*,#17840,.F.) ;
#25872 = ORIENTED_EDGE('',*,*,#18225,.F.) ;
#25873 = ORIENTED_EDGE('',*,*,#18223,.F.) ;
#25874 = ORIENTED_EDGE('',*,*,#17838,.F.) ;
#25875 = ORIENTED_EDGE('',*,*,#18224,.T.) ;
#25876 = ORIENTED_EDGE('',*,*,#18225,.T.) ;
#25877 = ORIENTED_EDGE('',*,*,#17842,.F.) ;
#25878 = ORIENTED_EDGE('',*,*,#18226,.T.) ;
#25879 = ORIENTED_EDGE('',*,*,#18227,.F.) ;
#25880 = ORIENTED_EDGE('',*,*,#17843,.F.) ;
#25881 = ORIENTED_EDGE('',*,*,#18228,.F.) ;
#25882 = ORIENTED_EDGE('',*,*,#18226,.F.) ;
#25883 = ORIENTED_EDGE('',*,*,#17841,.F.) ;
#25884 = ORIENTED_EDGE('',*,*,#18227,.T.) ;
#25885 = ORIENTED_EDGE('',*,*,#18228,.T.) ;
#25886 = ORIENTED_EDGE('',*,*,#17845,.F.) ;
#25887 = ORIENTED_EDGE('',*,*,#18229,.T.) ;
#25888 = ORIENTED_EDGE('',*,*,#18230,.F.) ;
#25889 = ORIENTED_EDGE('',*,*,#17846,.F.) ;
#25890 = ORIENTED_EDGE('',*,*,#18231,.F.) ;
#25891 = ORIENTED_EDGE('',*,*,#18229,.F.) ;
#25892 = ORIENTED_EDGE('',*,*,#17844,.F.) ;
#25893 = ORIENTED_EDGE('',*,*,#18230,.T.) ;
#25894 = ORIENTED_EDGE('',*,*,#18231,.T.) ;
#25895 = ORIENTED_EDGE('',*,*,#17850,.F.) ;
#25896 = ORIENTED_EDGE('',*,*,#18232,.T.) ;
#25897 = ORIENTED_EDGE('',*,*,#18233,.F.) ;
#25898 = ORIENTED_EDGE('',*,*,#17851,.F.) ;
#25899 = ORIENTED_EDGE('',*,*,#18234,.F.) ;
#25900 = ORIENTED_EDGE('',*,*,#18232,.F.) ;
#25901 = ORIENTED_EDGE('',*,*,#17849,.F.) ;
#25902 = ORIENTED_EDGE('',*,*,#17847,.F.) ;
#25903 = ORIENTED_EDGE('',*,*,#18233,.T.) ;
#25904 = ORIENTED_EDGE('',*,*,#18234,.T.) ;
#25905 = ORIENTED_EDGE('',*,*,#17853,.F.) ;
#25906 = ORIENTED_EDGE('',*,*,#18235,.T.) ;
#25907 = ORIENTED_EDGE('',*,*,#18236,.F.) ;
#25908 = ORIENTED_EDGE('',*,*,#17854,.F.) ;
#25909 = ORIENTED_EDGE('',*,*,#18237,.F.) ;
#25910 = ORIENTED_EDGE('',*,*,#18235,.F.) ;
#25911 = ORIENTED_EDGE('',*,*,#17852,.F.) ;
#25912 = ORIENTED_EDGE('',*,*,#18236,.T.) ;
#25913 = ORIENTED_EDGE('',*,*,#18237,.T.) ;
#25914 = ORIENTED_EDGE('',*,*,#17856,.F.) ;
#25915 = ORIENTED_EDGE('',*,*,#18238,.T.) ;
#25916 = ORIENTED_EDGE('',*,*,#18239,.F.) ;
#25917 = ORIENTED_EDGE('',*,*,#17857,.F.) ;
#25918 = ORIENTED_EDGE('',*,*,#18240,.F.) ;
#25919 = ORIENTED_EDGE('',*,*,#18238,.F.) ;
#25920 = ORIENTED_EDGE('',*,*,#17855,.F.) ;
#25921 = ORIENTED_EDGE('',*,*,#18239,.T.) ;
#25922 = ORIENTED_EDGE('',*,*,#18240,.T.) ;
#25923 = ORIENTED_EDGE('',*,*,#17859,.F.) ;
#25924 = ORIENTED_EDGE('',*,*,#18241,.T.) ;
#25925 = ORIENTED_EDGE('',*,*,#18242,.F.) ;
#25926 = ORIENTED_EDGE('',*,*,#17860,.F.) ;
#25927 = ORIENTED_EDGE('',*,*,#18243,.F.) ;
#25928 = ORIENTED_EDGE('',*,*,#18241,.F.) ;
#25929 = ORIENTED_EDGE('',*,*,#17858,.F.) ;
#25930 = ORIENTED_EDGE('',*,*,#18242,.T.) ;
#25931 = ORIENTED_EDGE('',*,*,#18243,.T.) ;
#25932 = ORIENTED_EDGE('',*,*,#17864,.F.) ;
#25933 = ORIENTED_EDGE('',*,*,#18244,.T.) ;
#25934 = ORIENTED_EDGE('',*,*,#18245,.F.) ;
#25935 = ORIENTED_EDGE('',*,*,#17865,.F.) ;
#25936 = ORIENTED_EDGE('',*,*,#18246,.F.) ;
#25937 = ORIENTED_EDGE('',*,*,#18244,.F.) ;
#25938 = ORIENTED_EDGE('',*,*,#17863,.F.) ;
#25939 = ORIENTED_EDGE('',*,*,#17861,.F.) ;
#25940 = ORIENTED_EDGE('',*,*,#18245,.T.) ;
#25941 = ORIENTED_EDGE('',*,*,#18246,.T.) ;
#25942 = ORIENTED_EDGE('',*,*,#17867,.F.) ;
#25943 = ORIENTED_EDGE('',*,*,#18247,.T.) ;
#25944 = ORIENTED_EDGE('',*,*,#18248,.F.) ;
#25945 = ORIENTED_EDGE('',*,*,#17868,.F.) ;
#25946 = ORIENTED_EDGE('',*,*,#18249,.F.) ;
#25947 = ORIENTED_EDGE('',*,*,#18247,.F.) ;
#25948 = ORIENTED_EDGE('',*,*,#17866,.F.) ;
#25949 = ORIENTED_EDGE('',*,*,#18248,.T.) ;
#25950 = ORIENTED_EDGE('',*,*,#18249,.T.) ;
#25951 = ORIENTED_EDGE('',*,*,#17870,.F.) ;
#25952 = ORIENTED_EDGE('',*,*,#18250,.T.) ;
#25953 = ORIENTED_EDGE('',*,*,#18251,.F.) ;
#25954 = ORIENTED_EDGE('',*,*,#17871,.F.) ;
#25955 = ORIENTED_EDGE('',*,*,#18252,.F.) ;
#25956 = ORIENTED_EDGE('',*,*,#18250,.F.) ;
#25957 = ORIENTED_EDGE('',*,*,#17869,.F.) ;
#25958 = ORIENTED_EDGE('',*,*,#18251,.T.) ;
#25959 = ORIENTED_EDGE('',*,*,#18252,.T.) ;
#25960 = ORIENTED_EDGE('',*,*,#17873,.F.) ;
#25961 = ORIENTED_EDGE('',*,*,#18253,.T.) ;
#25962 = ORIENTED_EDGE('',*,*,#18254,.F.) ;
#25963 = ORIENTED_EDGE('',*,*,#17874,.F.) ;
#25964 = ORIENTED_EDGE('',*,*,#18255,.F.) ;
#25965 = ORIENTED_EDGE('',*,*,#18253,.F.) ;
#25966 = ORIENTED_EDGE('',*,*,#17872,.F.) ;
#25967 = ORIENTED_EDGE('',*,*,#18254,.T.) ;
#25968 = ORIENTED_EDGE('',*,*,#18255,.T.) ;
#25969 = ORIENTED_EDGE('',*,*,#17878,.F.) ;
#25970 = ORIENTED_EDGE('',*,*,#18256,.T.) ;
#25971 = ORIENTED_EDGE('',*,*,#18257,.F.) ;
#25972 = ORIENTED_EDGE('',*,*,#17879,.F.) ;
#25973 = ORIENTED_EDGE('',*,*,#18258,.F.) ;
#25974 = ORIENTED_EDGE('',*,*,#18256,.F.) ;
#25975 = ORIENTED_EDGE('',*,*,#17877,.F.) ;
#25976 = ORIENTED_EDGE('',*,*,#17875,.F.) ;
#25977 = ORIENTED_EDGE('',*,*,#18257,.T.) ;
#25978 = ORIENTED_EDGE('',*,*,#18258,.T.) ;
#25979 = ORIENTED_EDGE('',*,*,#17881,.F.) ;
#25980 = ORIENTED_EDGE('',*,*,#18259,.T.) ;
#25981 = ORIENTED_EDGE('',*,*,#18260,.F.) ;
#25982 = ORIENTED_EDGE('',*,*,#17882,.F.) ;
#25983 = ORIENTED_EDGE('',*,*,#18261,.F.) ;
#25984 = ORIENTED_EDGE('',*,*,#18259,.F.) ;
#25985 = ORIENTED_EDGE('',*,*,#17880,.F.) ;
#25986 = ORIENTED_EDGE('',*,*,#18260,.T.) ;
#25987 = ORIENTED_EDGE('',*,*,#18261,.T.) ;
#25988 = ORIENTED_EDGE('',*,*,#17884,.F.) ;
#25989 = ORIENTED_EDGE('',*,*,#18262,.T.) ;
#25990 = ORIENTED_EDGE('',*,*,#18263,.F.) ;
#25991 = ORIENTED_EDGE('',*,*,#17885,.F.) ;
#25992 = ORIENTED_EDGE('',*,*,#18264,.F.) ;
#25993 = ORIENTED_EDGE('',*,*,#18262,.F.) ;
#25994 = ORIENTED_EDGE('',*,*,#17883,.F.) ;
#25995 = ORIENTED_EDGE('',*,*,#18263,.T.) ;
#25996 = ORIENTED_EDGE('',*,*,#18264,.T.) ;
#25997 = ORIENTED_EDGE('',*,*,#17887,.F.) ;
#25998 = ORIENTED_EDGE('',*,*,#18265,.T.) ;
#25999 = ORIENTED_EDGE('',*,*,#18266,.F.) ;
#26000 = ORIENTED_EDGE('',*,*,#18265,.F.) ;
#26001 = ORIENTED_EDGE('',*,*,#17886,.F.) ;
#26002 = ORIENTED_EDGE('',*,*,#18266,.T.) ;
#26003 = ORIENTED_EDGE('',*,*,#18267,.F.) ;
#26004 = ORIENTED_EDGE('',*,*,#18268,.T.) ;
#26005 = ORIENTED_EDGE('',*,*,#18269,.F.) ;
#26006 = ORIENTED_EDGE('',*,*,#18270,.T.) ;
#26007 = ORIENTED_EDGE('',*,*,#18271,.F.) ;
#26008 = ORIENTED_EDGE('',*,*,#18270,.F.) ;
#26009 = ORIENTED_EDGE('',*,*,#18272,.F.) ;
#26010 = ORIENTED_EDGE('',*,*,#18273,.F.) ;
#26011 = ORIENTED_EDGE('',*,*,#18268,.F.) ;
#26012 = ORIENTED_EDGE('',*,*,#18274,.F.) ;
#26013 = ORIENTED_EDGE('',*,*,#18275,.T.) ;
#26014 = ORIENTED_EDGE('',*,*,#18276,.F.) ;
#26015 = ORIENTED_EDGE('',*,*,#18275,.F.) ;
#26016 = ORIENTED_EDGE('',*,*,#18271,.T.) ;
#26017 = ORIENTED_EDGE('',*,*,#18274,.T.) ;
#26018 = ORIENTED_EDGE('',*,*,#18267,.T.) ;
#26019 = ORIENTED_EDGE('',*,*,#18276,.T.) ;
#26020 = ORIENTED_EDGE('',*,*,#18272,.T.) ;
#26021 = ORIENTED_EDGE('',*,*,#18277,.T.) ;
#26022 = ORIENTED_EDGE('',*,*,#18278,.F.) ;
#26023 = ORIENTED_EDGE('',*,*,#18277,.F.) ;
#26024 = ORIENTED_EDGE('',*,*,#18269,.T.) ;
#26025 = ORIENTED_EDGE('',*,*,#18273,.T.) ;
#26026 = ORIENTED_EDGE('',*,*,#18278,.T.) ;
#26027 = ORIENTED_EDGE('',*,*,#18279,.T.) ;
#26028 = ORIENTED_EDGE('',*,*,#18279,.F.) ;
#26029 = ORIENTED_EDGE('',*,*,#18280,.F.) ;
#26030 = ORIENTED_EDGE('',*,*,#18281,.F.) ;
#26031 = ORIENTED_EDGE('',*,*,#18281,.T.) ;
#26032 = ORIENTED_EDGE('',*,*,#18282,.T.) ;
#26033 = ORIENTED_EDGE('',*,*,#18280,.T.) ;
#26034 = ORIENTED_EDGE('',*,*,#18282,.F.) ;
#26035 = ORIENTED_EDGE('',*,*,#18283,.T.) ;
#26036 = ORIENTED_EDGE('',*,*,#18284,.T.) ;
#26037 = ORIENTED_EDGE('',*,*,#18285,.T.) ;
#26038 = ORIENTED_EDGE('',*,*,#18286,.F.) ;
#26039 = ORIENTED_EDGE('',*,*,#18287,.T.) ;
#26040 = ORIENTED_EDGE('',*,*,#18288,.F.) ;
#26041 = ORIENTED_EDGE('',*,*,#18289,.T.) ;
#26042 = ORIENTED_EDGE('',*,*,#18283,.F.) ;
#26043 = ORIENTED_EDGE('',*,*,#18289,.F.) ;
#26044 = ORIENTED_EDGE('',*,*,#18290,.F.) ;
#26045 = ORIENTED_EDGE('',*,*,#18291,.T.) ;
#26046 = ORIENTED_EDGE('',*,*,#18292,.T.) ;
#26047 = ORIENTED_EDGE('',*,*,#18293,.F.) ;
#26048 = ORIENTED_EDGE('',*,*,#18294,.F.) ;
#26049 = ORIENTED_EDGE('',*,*,#18291,.F.) ;
#26050 = ORIENTED_EDGE('',*,*,#18295,.T.) ;
#26051 = ORIENTED_EDGE('',*,*,#18296,.F.) ;
#26052 = ORIENTED_EDGE('',*,*,#18287,.F.) ;
#26053 = ORIENTED_EDGE('',*,*,#18297,.F.) ;
#26054 = ORIENTED_EDGE('',*,*,#18295,.F.) ;
#26055 = ORIENTED_EDGE('',*,*,#18298,.T.) ;
#26056 = ORIENTED_EDGE('',*,*,#18299,.T.) ;
#26057 = ORIENTED_EDGE('',*,*,#18292,.F.) ;
#26058 = ORIENTED_EDGE('',*,*,#18299,.F.) ;
#26059 = ORIENTED_EDGE('',*,*,#18300,.T.) ;
#26060 = ORIENTED_EDGE('',*,*,#18285,.F.) ;
#26061 = ORIENTED_EDGE('',*,*,#18284,.F.) ;
#26062 = ORIENTED_EDGE('',*,*,#18301,.T.) ;
#26063 = ORIENTED_EDGE('',*,*,#18302,.T.) ;
#26064 = ORIENTED_EDGE('',*,*,#18293,.T.) ;
#26065 = ORIENTED_EDGE('',*,*,#18303,.T.) ;
#26066 = ORIENTED_EDGE('',*,*,#18301,.F.) ;
#26067 = ORIENTED_EDGE('',*,*,#18298,.F.) ;
#26068 = ORIENTED_EDGE('',*,*,#18286,.T.) ;
#26069 = ORIENTED_EDGE('',*,*,#18300,.F.) ;
#26070 = ORIENTED_EDGE('',*,*,#18296,.T.) ;
#26071 = ORIENTED_EDGE('',*,*,#18297,.T.) ;
#26072 = ORIENTED_EDGE('',*,*,#18290,.T.) ;
#26073 = ORIENTED_EDGE('',*,*,#18288,.T.) ;
#26074 = ORIENTED_EDGE('',*,*,#18294,.T.) ;
#26075 = ORIENTED_EDGE('',*,*,#18302,.F.) ;
#26076 = ORIENTED_EDGE('',*,*,#18304,.F.) ;
#26077 = ORIENTED_EDGE('',*,*,#18304,.T.) ;
#26078 = ORIENTED_EDGE('',*,*,#18303,.F.) ;
#26079 = ORIENTED_EDGE('',*,*,#18305,.F.) ;
#26080 = ORIENTED_EDGE('',*,*,#18306,.T.) ;
#26081 = ORIENTED_EDGE('',*,*,#18307,.F.) ;
#26082 = ORIENTED_EDGE('',*,*,#18306,.F.) ;
#26083 = ORIENTED_EDGE('',*,*,#18307,.T.) ;
#26084 = ORIENTED_EDGE('',*,*,#18308,.F.) ;
#26085 = ORIENTED_EDGE('',*,*,#18309,.F.) ;
#26086 = ORIENTED_EDGE('',*,*,#18310,.F.) ;
#26087 = ORIENTED_EDGE('',*,*,#18311,.F.) ;
#26088 = ORIENTED_EDGE('',*,*,#18312,.T.) ;
#26089 = ORIENTED_EDGE('',*,*,#18313,.T.) ;
#26090 = ORIENTED_EDGE('',*,*,#18311,.T.) ;
#26091 = ORIENTED_EDGE('',*,*,#18314,.T.) ;
#26092 = ORIENTED_EDGE('',*,*,#18315,.T.) ;
#26093 = ORIENTED_EDGE('',*,*,#18316,.T.) ;
#26094 = ORIENTED_EDGE('',*,*,#18317,.T.) ;
#26095 = ORIENTED_EDGE('',*,*,#18318,.T.) ;
#26096 = ORIENTED_EDGE('',*,*,#18309,.T.) ;
#26097 = ORIENTED_EDGE('',*,*,#18319,.T.) ;
#26098 = ORIENTED_EDGE('',*,*,#18320,.T.) ;
#26099 = ORIENTED_EDGE('',*,*,#18317,.F.) ;
#26100 = ORIENTED_EDGE('',*,*,#18321,.F.) ;
#26101 = ORIENTED_EDGE('',*,*,#18315,.F.) ;
#26102 = ORIENTED_EDGE('',*,*,#18305,.T.) ;
#26103 = ORIENTED_EDGE('',*,*,#18310,.T.) ;
#26104 = ORIENTED_EDGE('',*,*,#18318,.F.) ;
#26105 = ORIENTED_EDGE('',*,*,#18320,.F.) ;
#26106 = ORIENTED_EDGE('',*,*,#18314,.F.) ;
#26107 = ORIENTED_EDGE('',*,*,#18308,.T.) ;
#26108 = ORIENTED_EDGE('',*,*,#18313,.F.) ;
#26109 = ORIENTED_EDGE('',*,*,#18322,.T.) ;
#26110 = ORIENTED_EDGE('',*,*,#18319,.F.) ;
#26111 = ORIENTED_EDGE('',*,*,#18321,.T.) ;
#26112 = ORIENTED_EDGE('',*,*,#18316,.F.) ;
#26113 = ORIENTED_EDGE('',*,*,#18322,.F.) ;
#26114 = ORIENTED_EDGE('',*,*,#18312,.F.) ;
#26115 = ORIENTED_EDGE('',*,*,#18323,.T.) ;
#26116 = ORIENTED_EDGE('',*,*,#18324,.T.) ;
#26117 = ORIENTED_EDGE('',*,*,#18325,.T.) ;
#26118 = ORIENTED_EDGE('',*,*,#18323,.F.) ;
#26119 = ORIENTED_EDGE('',*,*,#18326,.T.) ;
#26120 = ORIENTED_EDGE('',*,*,#18327,.T.) ;
#26121 = ORIENTED_EDGE('',*,*,#18328,.T.) ;
#26122 = ORIENTED_EDGE('',*,*,#18329,.F.) ;
#26123 = ORIENTED_EDGE('',*,*,#18325,.F.) ;
#26124 = ORIENTED_EDGE('',*,*,#18328,.F.) ;
#26125 = ORIENTED_EDGE('',*,*,#18330,.T.) ;
#26126 = ORIENTED_EDGE('',*,*,#18326,.F.) ;
#26127 = ORIENTED_EDGE('',*,*,#18331,.T.) ;
#26128 = ORIENTED_EDGE('',*,*,#18332,.T.) ;
#26129 = ORIENTED_EDGE('',*,*,#18324,.F.) ;
#26130 = ORIENTED_EDGE('',*,*,#18329,.T.) ;
#26131 = ORIENTED_EDGE('',*,*,#18331,.F.) ;
#26132 = ORIENTED_EDGE('',*,*,#18332,.F.) ;
#26133 = ORIENTED_EDGE('',*,*,#18333,.T.) ;
#26134 = ORIENTED_EDGE('',*,*,#18327,.F.) ;
#26135 = ORIENTED_EDGE('',*,*,#18330,.F.) ;
#26136 = ORIENTED_EDGE('',*,*,#18333,.F.) ;
#26137 = ORIENTED_EDGE('',*,*,#18334,.F.) ;
#26138 = ORIENTED_EDGE('',*,*,#18335,.F.) ;
#26139 = ORIENTED_EDGE('',*,*,#18336,.T.) ;
#26140 = ORIENTED_EDGE('',*,*,#18337,.F.) ;
#26141 = ORIENTED_EDGE('',*,*,#18338,.F.) ;
#26142 = ORIENTED_EDGE('',*,*,#18336,.F.) ;
#26143 = ORIENTED_EDGE('',*,*,#18339,.F.) ;
#26144 = ORIENTED_EDGE('',*,*,#18340,.T.) ;
#26145 = ORIENTED_EDGE('',*,*,#18340,.F.) ;
#26146 = ORIENTED_EDGE('',*,*,#18341,.F.) ;
#26147 = ORIENTED_EDGE('',*,*,#18342,.T.) ;
#26148 = ORIENTED_EDGE('',*,*,#18337,.T.) ;
#26149 = ORIENTED_EDGE('',*,*,#18343,.T.) ;
#26150 = ORIENTED_EDGE('',*,*,#18344,.F.) ;
#26151 = ORIENTED_EDGE('',*,*,#18343,.F.) ;
#26152 = ORIENTED_EDGE('',*,*,#18338,.T.) ;
#26153 = ORIENTED_EDGE('',*,*,#18342,.F.) ;
#26154 = ORIENTED_EDGE('',*,*,#18334,.T.) ;
#26155 = ORIENTED_EDGE('',*,*,#18335,.T.) ;
#26156 = ORIENTED_EDGE('',*,*,#18344,.T.) ;
#26157 = ORIENTED_EDGE('',*,*,#18339,.T.) ;
#26158 = ORIENTED_EDGE('',*,*,#18341,.T.) ;
#26159 = ORIENTED_EDGE('',*,*,#18345,.F.) ;
#26160 = ORIENTED_EDGE('',*,*,#18346,.F.) ;
#26161 = ORIENTED_EDGE('',*,*,#18347,.F.) ;
#26162 = ORIENTED_EDGE('',*,*,#18348,.F.) ;
#26163 = ORIENTED_EDGE('',*,*,#18349,.F.) ;
#26164 = ORIENTED_EDGE('',*,*,#18350,.T.) ;
#26165 = ORIENTED_EDGE('',*,*,#18351,.F.) ;
#26166 = ORIENTED_EDGE('',*,*,#18352,.F.) ;
#26167 = ORIENTED_EDGE('',*,*,#18353,.T.) ;
#26168 = ORIENTED_EDGE('',*,*,#18353,.F.) ;
#26169 = ORIENTED_EDGE('',*,*,#18354,.T.) ;
#26170 = ORIENTED_EDGE('',*,*,#18352,.T.) ;
#26171 = ORIENTED_EDGE('',*,*,#18355,.T.) ;
#26172 = ORIENTED_EDGE('',*,*,#18348,.T.) ;
#26173 = ORIENTED_EDGE('',*,*,#18356,.T.) ;
#26174 = ORIENTED_EDGE('',*,*,#18357,.T.) ;
#26175 = ORIENTED_EDGE('',*,*,#18345,.T.) ;
#26176 = ORIENTED_EDGE('',*,*,#18354,.F.) ;
#26177 = ORIENTED_EDGE('',*,*,#18351,.T.) ;
#26178 = ORIENTED_EDGE('',*,*,#18350,.F.) ;
#26179 = ORIENTED_EDGE('',*,*,#18349,.T.) ;
#26180 = ORIENTED_EDGE('',*,*,#18356,.F.) ;
#26181 = ORIENTED_EDGE('',*,*,#18347,.T.) ;
#26182 = ORIENTED_EDGE('',*,*,#18346,.T.) ;
#26183 = ORIENTED_EDGE('',*,*,#18357,.F.) ;
#26184 = ORIENTED_EDGE('',*,*,#18358,.T.) ;
#26185 = ORIENTED_EDGE('',*,*,#18355,.F.) ;
#26186 = ORIENTED_EDGE('',*,*,#18358,.F.) ;
#26187 = ORIENTED_EDGE('',*,*,#18359,.F.) ;
#26188 = ORIENTED_EDGE('',*,*,#18360,.T.) ;
#26189 = ORIENTED_EDGE('',*,*,#18361,.F.) ;
#26190 = ORIENTED_EDGE('',*,*,#18360,.F.) ;
#26191 = ORIENTED_EDGE('',*,*,#18362,.F.) ;
#26192 = ORIENTED_EDGE('',*,*,#18363,.T.) ;
#26193 = ORIENTED_EDGE('',*,*,#18364,.F.) ;
#26194 = ORIENTED_EDGE('',*,*,#18363,.F.) ;
#26195 = ORIENTED_EDGE('',*,*,#18364,.T.) ;
#26196 = ORIENTED_EDGE('',*,*,#18359,.T.) ;
#26197 = ORIENTED_EDGE('',*,*,#18362,.T.) ;
#26198 = ORIENTED_EDGE('',*,*,#18361,.T.) ;
#26199 = ORIENTED_EDGE('',*,*,#18365,.F.) ;
#26200 = ORIENTED_EDGE('',*,*,#18366,.F.) ;
#26201 = ORIENTED_EDGE('',*,*,#18367,.F.) ;
#26202 = ORIENTED_EDGE('',*,*,#18368,.F.) ;
#26203 = ORIENTED_EDGE('',*,*,#18366,.T.) ;
#26204 = ORIENTED_EDGE('',*,*,#18369,.F.) ;
#26205 = ORIENTED_EDGE('',*,*,#18370,.T.) ;
#26206 = ORIENTED_EDGE('',*,*,#18371,.F.) ;
#26207 = ORIENTED_EDGE('',*,*,#18372,.F.) ;
#26208 = ORIENTED_EDGE('',*,*,#18373,.F.) ;
#26209 = ORIENTED_EDGE('',*,*,#18365,.T.) ;
#26210 = ORIENTED_EDGE('',*,*,#18374,.T.) ;
#26211 = ORIENTED_EDGE('',*,*,#18375,.T.) ;
#26212 = ORIENTED_EDGE('',*,*,#18369,.T.) ;
#26213 = ORIENTED_EDGE('',*,*,#18367,.T.) ;
#26214 = ORIENTED_EDGE('',*,*,#18373,.T.) ;
#26215 = ORIENTED_EDGE('',*,*,#18376,.T.) ;
#26216 = ORIENTED_EDGE('',*,*,#18377,.T.) ;
#26217 = ORIENTED_EDGE('',*,*,#18378,.T.) ;
#26218 = ORIENTED_EDGE('',*,*,#18379,.T.) ;
#26219 = ORIENTED_EDGE('',*,*,#18371,.T.) ;
#26220 = ORIENTED_EDGE('',*,*,#18380,.T.) ;
#26221 = ORIENTED_EDGE('',*,*,#18372,.T.) ;
#26222 = ORIENTED_EDGE('',*,*,#18379,.F.) ;
#26223 = ORIENTED_EDGE('',*,*,#18381,.F.) ;
#26224 = ORIENTED_EDGE('',*,*,#18376,.F.) ;
#26225 = ORIENTED_EDGE('',*,*,#18382,.T.) ;
#26226 = ORIENTED_EDGE('',*,*,#18380,.F.) ;
#26227 = ORIENTED_EDGE('',*,*,#18370,.F.) ;
#26228 = ORIENTED_EDGE('',*,*,#18375,.F.) ;
#26229 = ORIENTED_EDGE('',*,*,#18368,.T.) ;
#26230 = ORIENTED_EDGE('',*,*,#18377,.F.) ;
#26231 = ORIENTED_EDGE('',*,*,#18381,.T.) ;
#26232 = ORIENTED_EDGE('',*,*,#18378,.F.) ;
#26233 = ORIENTED_EDGE('',*,*,#18382,.F.) ;
#26234 = ORIENTED_EDGE('',*,*,#18374,.F.) ;
#26235 = ORIENTED_EDGE('',*,*,#18383,.T.) ;
#26236 = ORIENTED_EDGE('',*,*,#18384,.T.) ;
#26237 = ORIENTED_EDGE('',*,*,#18385,.T.) ;
#26238 = ORIENTED_EDGE('',*,*,#18386,.T.) ;
#26239 = ORIENTED_EDGE('',*,*,#18387,.T.) ;
#26240 = ORIENTED_EDGE('',*,*,#18388,.T.) ;
#26241 = ORIENTED_EDGE('',*,*,#18389,.T.) ;
#26242 = ORIENTED_EDGE('',*,*,#18390,.T.) ;
#26243 = ORIENTED_EDGE('',*,*,#18391,.T.) ;
#26244 = ORIENTED_EDGE('',*,*,#18388,.F.) ;
#26245 = ORIENTED_EDGE('',*,*,#18392,.F.) ;
#26246 = ORIENTED_EDGE('',*,*,#18386,.F.) ;
#26247 = ORIENTED_EDGE('',*,*,#18393,.T.) ;
#26248 = ORIENTED_EDGE('',*,*,#18389,.F.) ;
#26249 = ORIENTED_EDGE('',*,*,#18391,.F.) ;
#26250 = ORIENTED_EDGE('',*,*,#18385,.F.) ;
#26251 = ORIENTED_EDGE('',*,*,#18394,.T.) ;
#26252 = ORIENTED_EDGE('',*,*,#18390,.F.) ;
#26253 = ORIENTED_EDGE('',*,*,#18393,.F.) ;
#26254 = ORIENTED_EDGE('',*,*,#18384,.F.) ;
#26255 = ORIENTED_EDGE('',*,*,#18392,.T.) ;
#26256 = ORIENTED_EDGE('',*,*,#18387,.F.) ;
#26257 = ORIENTED_EDGE('',*,*,#18394,.F.) ;
#26258 = ORIENTED_EDGE('',*,*,#18383,.F.) ;
#26259 = ORIENTED_EDGE('',*,*,#18395,.F.) ;
#26260 = ORIENTED_EDGE('',*,*,#18396,.F.) ;
#26261 = ORIENTED_EDGE('',*,*,#18397,.F.) ;
#26262 = ORIENTED_EDGE('',*,*,#18398,.F.) ;
#26263 = ORIENTED_EDGE('',*,*,#18399,.T.) ;
#26264 = ORIENTED_EDGE('',*,*,#18400,.F.) ;
#26265 = ORIENTED_EDGE('',*,*,#18401,.F.) ;
#26266 = ORIENTED_EDGE('',*,*,#18402,.F.) ;
#26267 = ORIENTED_EDGE('',*,*,#18403,.F.) ;
#26268 = ORIENTED_EDGE('',*,*,#18397,.T.) ;
#26269 = ORIENTED_EDGE('',*,*,#18403,.T.) ;
#26270 = ORIENTED_EDGE('',*,*,#18404,.T.) ;
#26271 = ORIENTED_EDGE('',*,*,#18405,.T.) ;
#26272 = ORIENTED_EDGE('',*,*,#18398,.T.) ;
#26273 = ORIENTED_EDGE('',*,*,#18406,.F.) ;
#26274 = ORIENTED_EDGE('',*,*,#18400,.T.) ;
#26275 = ORIENTED_EDGE('',*,*,#18407,.T.) ;
#26276 = ORIENTED_EDGE('',*,*,#18408,.T.) ;
#26277 = ORIENTED_EDGE('',*,*,#18409,.T.) ;
#26278 = ORIENTED_EDGE('',*,*,#18407,.F.) ;
#26279 = ORIENTED_EDGE('',*,*,#18399,.F.) ;
#26280 = ORIENTED_EDGE('',*,*,#18405,.F.) ;
#26281 = ORIENTED_EDGE('',*,*,#18410,.F.) ;
#26282 = ORIENTED_EDGE('',*,*,#18408,.F.) ;
#26283 = ORIENTED_EDGE('',*,*,#18409,.F.) ;
#26284 = ORIENTED_EDGE('',*,*,#18404,.F.) ;
#26285 = ORIENTED_EDGE('',*,*,#18402,.T.) ;
#26286 = ORIENTED_EDGE('',*,*,#18411,.F.) ;
#26287 = ORIENTED_EDGE('',*,*,#18395,.T.) ;
#26288 = ORIENTED_EDGE('',*,*,#18406,.T.) ;
#26289 = ORIENTED_EDGE('',*,*,#18410,.T.) ;
#26290 = ORIENTED_EDGE('',*,*,#18412,.T.) ;
#26291 = ORIENTED_EDGE('',*,*,#18413,.T.) ;
#26292 = ORIENTED_EDGE('',*,*,#18414,.T.) ;
#26293 = ORIENTED_EDGE('',*,*,#18414,.F.) ;
#26294 = ORIENTED_EDGE('',*,*,#18415,.T.) ;
#26295 = ORIENTED_EDGE('',*,*,#18416,.F.) ;
#26296 = ORIENTED_EDGE('',*,*,#18415,.F.) ;
#26297 = ORIENTED_EDGE('',*,*,#18417,.F.) ;
#26298 = ORIENTED_EDGE('',*,*,#18418,.T.) ;
#26299 = ORIENTED_EDGE('',*,*,#18412,.F.) ;
#26300 = ORIENTED_EDGE('',*,*,#18411,.T.) ;
#26301 = ORIENTED_EDGE('',*,*,#18401,.T.) ;
#26302 = ORIENTED_EDGE('',*,*,#18396,.T.) ;
#26303 = ORIENTED_EDGE('',*,*,#18413,.F.) ;
#26304 = ORIENTED_EDGE('',*,*,#18418,.F.) ;
#26305 = ORIENTED_EDGE('',*,*,#18417,.T.) ;
#26306 = ORIENTED_EDGE('',*,*,#18416,.T.) ;
#26307 = ORIENTED_EDGE('',*,*,#18419,.F.) ;
#26308 = ORIENTED_EDGE('',*,*,#18420,.T.) ;
#26309 = ORIENTED_EDGE('',*,*,#18421,.F.) ;
#26310 = ORIENTED_EDGE('',*,*,#18420,.F.) ;
#26311 = ORIENTED_EDGE('',*,*,#18419,.T.) ;
#26312 = ORIENTED_EDGE('',*,*,#18422,.F.) ;
#26313 = ORIENTED_EDGE('',*,*,#18423,.T.) ;
#26314 = ORIENTED_EDGE('',*,*,#18424,.F.) ;
#26315 = ORIENTED_EDGE('',*,*,#18425,.T.) ;
#26316 = ORIENTED_EDGE('',*,*,#18426,.F.) ;
#26317 = ORIENTED_EDGE('',*,*,#18427,.T.) ;
#26318 = ORIENTED_EDGE('',*,*,#18428,.F.) ;
#26319 = ORIENTED_EDGE('',*,*,#18429,.T.) ;
#26320 = ORIENTED_EDGE('',*,*,#18423,.F.) ;
#26321 = ORIENTED_EDGE('',*,*,#18430,.F.) ;
#26322 = ORIENTED_EDGE('',*,*,#18431,.F.) ;
#26323 = ORIENTED_EDGE('',*,*,#18427,.F.) ;
#26324 = ORIENTED_EDGE('',*,*,#18432,.F.) ;
#26325 = ORIENTED_EDGE('',*,*,#18433,.F.) ;
#26326 = ORIENTED_EDGE('',*,*,#18434,.F.) ;
#26327 = ORIENTED_EDGE('',*,*,#18430,.T.) ;
#26328 = ORIENTED_EDGE('',*,*,#18422,.T.) ;
#26329 = ORIENTED_EDGE('',*,*,#18435,.T.) ;
#26330 = ORIENTED_EDGE('',*,*,#18436,.F.) ;
#26331 = ORIENTED_EDGE('',*,*,#18432,.T.) ;
#26332 = ORIENTED_EDGE('',*,*,#18426,.T.) ;
#26333 = ORIENTED_EDGE('',*,*,#18437,.T.) ;
#26334 = ORIENTED_EDGE('',*,*,#18434,.T.) ;
#26335 = ORIENTED_EDGE('',*,*,#18438,.T.) ;
#26336 = ORIENTED_EDGE('',*,*,#18428,.T.) ;
#26337 = ORIENTED_EDGE('',*,*,#18431,.T.) ;
#26338 = ORIENTED_EDGE('',*,*,#18424,.T.) ;
#26339 = ORIENTED_EDGE('',*,*,#18433,.T.) ;
#26340 = ORIENTED_EDGE('',*,*,#18436,.T.) ;
#26341 = ORIENTED_EDGE('',*,*,#18439,.T.) ;
#26342 = ORIENTED_EDGE('',*,*,#18425,.F.) ;
#26343 = ORIENTED_EDGE('',*,*,#18439,.F.) ;
#26344 = ORIENTED_EDGE('',*,*,#18437,.F.) ;
#26345 = ORIENTED_EDGE('',*,*,#18429,.F.) ;
#26346 = ORIENTED_EDGE('',*,*,#18438,.F.) ;
#26347 = ORIENTED_EDGE('',*,*,#18435,.F.) ;
#26348 = ORIENTED_EDGE('',*,*,#18421,.T.) ;
#26349 = ORIENTED_EDGE('',*,*,#18440,.F.) ;
#26350 = ORIENTED_EDGE('',*,*,#18441,.T.) ;
#26351 = ORIENTED_EDGE('',*,*,#18442,.F.) ;
#26352 = ORIENTED_EDGE('',*,*,#18441,.F.) ;
#26353 = ORIENTED_EDGE('',*,*,#18443,.F.) ;
#26354 = ORIENTED_EDGE('',*,*,#18444,.T.) ;
#26355 = ORIENTED_EDGE('',*,*,#18445,.F.) ;
#26356 = ORIENTED_EDGE('',*,*,#18446,.T.) ;
#26357 = ORIENTED_EDGE('',*,*,#18447,.F.) ;
#26358 = ORIENTED_EDGE('',*,*,#18448,.T.) ;
#26359 = ORIENTED_EDGE('',*,*,#18449,.F.) ;
#26360 = ORIENTED_EDGE('',*,*,#18450,.T.) ;
#26361 = ORIENTED_EDGE('',*,*,#18444,.F.) ;
#26362 = ORIENTED_EDGE('',*,*,#18451,.F.) ;
#26363 = ORIENTED_EDGE('',*,*,#18452,.F.) ;
#26364 = ORIENTED_EDGE('',*,*,#18448,.F.) ;
#26365 = ORIENTED_EDGE('',*,*,#18453,.F.) ;
#26366 = ORIENTED_EDGE('',*,*,#18454,.F.) ;
#26367 = ORIENTED_EDGE('',*,*,#18440,.T.) ;
#26368 = ORIENTED_EDGE('',*,*,#18455,.F.) ;
#26369 = ORIENTED_EDGE('',*,*,#18451,.T.) ;
#26370 = ORIENTED_EDGE('',*,*,#18443,.T.) ;
#26371 = ORIENTED_EDGE('',*,*,#18456,.T.) ;
#26372 = ORIENTED_EDGE('',*,*,#18457,.F.) ;
#26373 = ORIENTED_EDGE('',*,*,#18453,.T.) ;
#26374 = ORIENTED_EDGE('',*,*,#18447,.T.) ;
#26375 = ORIENTED_EDGE('',*,*,#18458,.T.) ;
#26376 = ORIENTED_EDGE('',*,*,#18455,.T.) ;
#26377 = ORIENTED_EDGE('',*,*,#18459,.T.) ;
#26378 = ORIENTED_EDGE('',*,*,#18449,.T.) ;
#26379 = ORIENTED_EDGE('',*,*,#18452,.T.) ;
#26380 = ORIENTED_EDGE('',*,*,#18445,.T.) ;
#26381 = ORIENTED_EDGE('',*,*,#18454,.T.) ;
#26382 = ORIENTED_EDGE('',*,*,#18457,.T.) ;
#26383 = ORIENTED_EDGE('',*,*,#18460,.T.) ;
#26384 = ORIENTED_EDGE('',*,*,#18446,.F.) ;
#26385 = ORIENTED_EDGE('',*,*,#18460,.F.) ;
#26386 = ORIENTED_EDGE('',*,*,#18458,.F.) ;
#26387 = ORIENTED_EDGE('',*,*,#18450,.F.) ;
#26388 = ORIENTED_EDGE('',*,*,#18459,.F.) ;
#26389 = ORIENTED_EDGE('',*,*,#18456,.F.) ;
#26390 = ORIENTED_EDGE('',*,*,#18442,.T.) ;
#26391 = ORIENTED_EDGE('',*,*,#18461,.F.) ;
#26392 = ORIENTED_EDGE('',*,*,#18462,.T.) ;
#26393 = ORIENTED_EDGE('',*,*,#18463,.F.) ;
#26394 = ORIENTED_EDGE('',*,*,#18462,.F.) ;
#26395 = ORIENTED_EDGE('',*,*,#18461,.T.) ;
#26396 = ORIENTED_EDGE('',*,*,#18464,.F.) ;
#26397 = ORIENTED_EDGE('',*,*,#18465,.T.) ;
#26398 = ORIENTED_EDGE('',*,*,#18466,.F.) ;
#26399 = ORIENTED_EDGE('',*,*,#18467,.T.) ;
#26400 = ORIENTED_EDGE('',*,*,#18468,.F.) ;
#26401 = ORIENTED_EDGE('',*,*,#18469,.T.) ;
#26402 = ORIENTED_EDGE('',*,*,#18470,.F.) ;
#26403 = ORIENTED_EDGE('',*,*,#18471,.T.) ;
#26404 = ORIENTED_EDGE('',*,*,#18465,.F.) ;
#26405 = ORIENTED_EDGE('',*,*,#18472,.F.) ;
#26406 = ORIENTED_EDGE('',*,*,#18473,.F.) ;
#26407 = ORIENTED_EDGE('',*,*,#18469,.F.) ;
#26408 = ORIENTED_EDGE('',*,*,#18474,.F.) ;
#26409 = ORIENTED_EDGE('',*,*,#18475,.F.) ;
#26410 = ORIENTED_EDGE('',*,*,#18476,.F.) ;
#26411 = ORIENTED_EDGE('',*,*,#18472,.T.) ;
#26412 = ORIENTED_EDGE('',*,*,#18464,.T.) ;
#26413 = ORIENTED_EDGE('',*,*,#18477,.T.) ;
#26414 = ORIENTED_EDGE('',*,*,#18478,.F.) ;
#26415 = ORIENTED_EDGE('',*,*,#18474,.T.) ;
#26416 = ORIENTED_EDGE('',*,*,#18468,.T.) ;
#26417 = ORIENTED_EDGE('',*,*,#18479,.T.) ;
#26418 = ORIENTED_EDGE('',*,*,#18476,.T.) ;
#26419 = ORIENTED_EDGE('',*,*,#18480,.T.) ;
#26420 = ORIENTED_EDGE('',*,*,#18470,.T.) ;
#26421 = ORIENTED_EDGE('',*,*,#18473,.T.) ;
#26422 = ORIENTED_EDGE('',*,*,#18466,.T.) ;
#26423 = ORIENTED_EDGE('',*,*,#18475,.T.) ;
#26424 = ORIENTED_EDGE('',*,*,#18478,.T.) ;
#26425 = ORIENTED_EDGE('',*,*,#18481,.T.) ;
#26426 = ORIENTED_EDGE('',*,*,#18467,.F.) ;
#26427 = ORIENTED_EDGE('',*,*,#18481,.F.) ;
#26428 = ORIENTED_EDGE('',*,*,#18479,.F.) ;
#26429 = ORIENTED_EDGE('',*,*,#18471,.F.) ;
#26430 = ORIENTED_EDGE('',*,*,#18480,.F.) ;
#26431 = ORIENTED_EDGE('',*,*,#18477,.F.) ;
#26432 = ORIENTED_EDGE('',*,*,#18463,.T.) ;
#26433 = ORIENTED_EDGE('',*,*,#18482,.F.) ;
#26434 = ORIENTED_EDGE('',*,*,#18483,.T.) ;
#26435 = ORIENTED_EDGE('',*,*,#18484,.F.) ;
#26436 = ORIENTED_EDGE('',*,*,#18483,.F.) ;
#26437 = ORIENTED_EDGE('',*,*,#18485,.F.) ;
#26438 = ORIENTED_EDGE('',*,*,#18486,.T.) ;
#26439 = ORIENTED_EDGE('',*,*,#18487,.F.) ;
#26440 = ORIENTED_EDGE('',*,*,#18488,.T.) ;
#26441 = ORIENTED_EDGE('',*,*,#18489,.F.) ;
#26442 = ORIENTED_EDGE('',*,*,#18490,.T.) ;
#26443 = ORIENTED_EDGE('',*,*,#18491,.F.) ;
#26444 = ORIENTED_EDGE('',*,*,#18492,.T.) ;
#26445 = ORIENTED_EDGE('',*,*,#18486,.F.) ;
#26446 = ORIENTED_EDGE('',*,*,#18493,.F.) ;
#26447 = ORIENTED_EDGE('',*,*,#18494,.F.) ;
#26448 = ORIENTED_EDGE('',*,*,#18490,.F.) ;
#26449 = ORIENTED_EDGE('',*,*,#18495,.F.) ;
#26450 = ORIENTED_EDGE('',*,*,#18496,.F.) ;
#26451 = ORIENTED_EDGE('',*,*,#18482,.T.) ;
#26452 = ORIENTED_EDGE('',*,*,#18497,.F.) ;
#26453 = ORIENTED_EDGE('',*,*,#18493,.T.) ;
#26454 = ORIENTED_EDGE('',*,*,#18485,.T.) ;
#26455 = ORIENTED_EDGE('',*,*,#18498,.T.) ;
#26456 = ORIENTED_EDGE('',*,*,#18499,.F.) ;
#26457 = ORIENTED_EDGE('',*,*,#18495,.T.) ;
#26458 = ORIENTED_EDGE('',*,*,#18489,.T.) ;
#26459 = ORIENTED_EDGE('',*,*,#18500,.T.) ;
#26460 = ORIENTED_EDGE('',*,*,#18497,.T.) ;
#26461 = ORIENTED_EDGE('',*,*,#18501,.T.) ;
#26462 = ORIENTED_EDGE('',*,*,#18491,.T.) ;
#26463 = ORIENTED_EDGE('',*,*,#18494,.T.) ;
#26464 = ORIENTED_EDGE('',*,*,#18487,.T.) ;
#26465 = ORIENTED_EDGE('',*,*,#18496,.T.) ;
#26466 = ORIENTED_EDGE('',*,*,#18499,.T.) ;
#26467 = ORIENTED_EDGE('',*,*,#18502,.T.) ;
#26468 = ORIENTED_EDGE('',*,*,#18488,.F.) ;
#26469 = ORIENTED_EDGE('',*,*,#18502,.F.) ;
#26470 = ORIENTED_EDGE('',*,*,#18500,.F.) ;
#26471 = ORIENTED_EDGE('',*,*,#18492,.F.) ;
#26472 = ORIENTED_EDGE('',*,*,#18501,.F.) ;
#26473 = ORIENTED_EDGE('',*,*,#18498,.F.) ;
#26474 = ORIENTED_EDGE('',*,*,#18484,.T.) ;
#26475 = ORIENTED_EDGE('',*,*,#18503,.T.) ;
#26476 = ORIENTED_EDGE('',*,*,#18504,.T.) ;
#26477 = ORIENTED_EDGE('',*,*,#18505,.F.) ;
#26478 = ORIENTED_EDGE('',*,*,#18506,.T.) ;
#26479 = ORIENTED_EDGE('',*,*,#18503,.F.) ;
#26480 = ORIENTED_EDGE('',*,*,#18506,.F.) ;
#26481 = ORIENTED_EDGE('',*,*,#18505,.T.) ;
#26482 = ORIENTED_EDGE('',*,*,#18504,.F.) ;
#26483 = ORIENTED_EDGE('',*,*,#18507,.T.) ;
#26484 = ORIENTED_EDGE('',*,*,#18508,.F.) ;
#26485 = ORIENTED_EDGE('',*,*,#18507,.F.) ;
#26486 = ORIENTED_EDGE('',*,*,#18508,.T.) ;
#26487 = ORIENTED_EDGE('',*,*,#18509,.T.) ;
#26488 = ORIENTED_EDGE('',*,*,#18510,.T.) ;
#26489 = ORIENTED_EDGE('',*,*,#18511,.F.) ;
#26490 = ORIENTED_EDGE('',*,*,#18512,.T.) ;
#26491 = ORIENTED_EDGE('',*,*,#18509,.F.) ;
#26492 = ORIENTED_EDGE('',*,*,#18512,.F.) ;
#26493 = ORIENTED_EDGE('',*,*,#18511,.T.) ;
#26494 = ORIENTED_EDGE('',*,*,#18510,.F.) ;
#26495 = ORIENTED_EDGE('',*,*,#18513,.T.) ;
#26496 = ORIENTED_EDGE('',*,*,#18514,.F.) ;
#26497 = ORIENTED_EDGE('',*,*,#18513,.F.) ;
#26498 = ORIENTED_EDGE('',*,*,#18514,.T.) ;
#26499 = ORIENTED_EDGE('',*,*,#18515,.F.) ;
#26500 = ORIENTED_EDGE('',*,*,#18516,.F.) ;
#26501 = ORIENTED_EDGE('',*,*,#18517,.F.) ;
#26502 = ORIENTED_EDGE('',*,*,#18518,.T.) ;
#26503 = ORIENTED_EDGE('',*,*,#18519,.T.) ;
#26504 = ORIENTED_EDGE('',*,*,#18520,.F.) ;
#26505 = ORIENTED_EDGE('',*,*,#18521,.F.) ;
#26506 = ORIENTED_EDGE('',*,*,#18522,.F.) ;
#26507 = ORIENTED_EDGE('',*,*,#18519,.F.) ;
#26508 = ORIENTED_EDGE('',*,*,#18523,.T.) ;
#26509 = ORIENTED_EDGE('',*,*,#18524,.T.) ;
#26510 = ORIENTED_EDGE('',*,*,#18525,.T.) ;
#26511 = ORIENTED_EDGE('',*,*,#18526,.T.) ;
#26512 = ORIENTED_EDGE('',*,*,#18527,.T.) ;
#26513 = ORIENTED_EDGE('',*,*,#18528,.T.) ;
#26514 = ORIENTED_EDGE('',*,*,#18529,.T.) ;
#26515 = ORIENTED_EDGE('',*,*,#18530,.T.) ;
#26516 = ORIENTED_EDGE('',*,*,#18531,.T.) ;
#26517 = ORIENTED_EDGE('',*,*,#18532,.F.) ;
#26518 = ORIENTED_EDGE('',*,*,#18532,.T.) ;
#26519 = ORIENTED_EDGE('',*,*,#18533,.T.) ;
#26520 = ORIENTED_EDGE('',*,*,#18534,.T.) ;
#26521 = ORIENTED_EDGE('',*,*,#18535,.T.) ;
#26522 = ORIENTED_EDGE('',*,*,#18536,.T.) ;
#26523 = ORIENTED_EDGE('',*,*,#18537,.T.) ;
#26524 = ORIENTED_EDGE('',*,*,#18538,.T.) ;
#26525 = ORIENTED_EDGE('',*,*,#18539,.T.) ;
#26526 = ORIENTED_EDGE('',*,*,#18540,.T.) ;
#26527 = ORIENTED_EDGE('',*,*,#18541,.T.) ;
#26528 = ORIENTED_EDGE('',*,*,#18542,.T.) ;
#26529 = ORIENTED_EDGE('',*,*,#18543,.T.) ;
#26530 = ORIENTED_EDGE('',*,*,#18544,.T.) ;
#26531 = ORIENTED_EDGE('',*,*,#18545,.T.) ;
#26532 = ORIENTED_EDGE('',*,*,#18546,.T.) ;
#26533 = ORIENTED_EDGE('',*,*,#18547,.T.) ;
#26534 = ORIENTED_EDGE('',*,*,#18548,.T.) ;
#26535 = ORIENTED_EDGE('',*,*,#18549,.T.) ;
#26536 = ORIENTED_EDGE('',*,*,#18550,.T.) ;
#26537 = ORIENTED_EDGE('',*,*,#18551,.T.) ;
#26538 = ORIENTED_EDGE('',*,*,#18552,.T.) ;
#26539 = ORIENTED_EDGE('',*,*,#18553,.T.) ;
#26540 = ORIENTED_EDGE('',*,*,#18521,.T.) ;
#26541 = ORIENTED_EDGE('',*,*,#18554,.T.) ;
#26542 = ORIENTED_EDGE('',*,*,#18555,.T.) ;
#26543 = ORIENTED_EDGE('',*,*,#18556,.T.) ;
#26544 = ORIENTED_EDGE('',*,*,#18557,.F.) ;
#26545 = ORIENTED_EDGE('',*,*,#18524,.F.) ;
#26546 = ORIENTED_EDGE('',*,*,#18558,.F.) ;
#26547 = ORIENTED_EDGE('',*,*,#18559,.T.) ;
#26548 = ORIENTED_EDGE('',*,*,#18560,.F.) ;
#26549 = ORIENTED_EDGE('',*,*,#18526,.F.) ;
#26550 = ORIENTED_EDGE('',*,*,#18561,.F.) ;
#26551 = ORIENTED_EDGE('',*,*,#18559,.F.) ;
#26552 = ORIENTED_EDGE('',*,*,#18560,.T.) ;
#26553 = ORIENTED_EDGE('',*,*,#18562,.T.) ;
#26554 = ORIENTED_EDGE('',*,*,#18563,.F.) ;
#26555 = ORIENTED_EDGE('',*,*,#18528,.F.) ;
#26556 = ORIENTED_EDGE('',*,*,#18564,.F.) ;
#26557 = ORIENTED_EDGE('',*,*,#18562,.F.) ;
#26558 = ORIENTED_EDGE('',*,*,#18561,.T.) ;
#26559 = ORIENTED_EDGE('',*,*,#18527,.F.) ;
#26560 = ORIENTED_EDGE('',*,*,#18563,.T.) ;
#26561 = ORIENTED_EDGE('',*,*,#18565,.T.) ;
#26562 = ORIENTED_EDGE('',*,*,#18566,.F.) ;
#26563 = ORIENTED_EDGE('',*,*,#18530,.F.) ;
#26564 = ORIENTED_EDGE('',*,*,#18567,.F.) ;
#26565 = ORIENTED_EDGE('',*,*,#18565,.F.) ;
#26566 = ORIENTED_EDGE('',*,*,#18564,.T.) ;
#26567 = ORIENTED_EDGE('',*,*,#18529,.F.) ;
#26568 = ORIENTED_EDGE('',*,*,#18566,.T.) ;
#26569 = ORIENTED_EDGE('',*,*,#18567,.T.) ;
#26570 = ORIENTED_EDGE('',*,*,#18533,.F.) ;
#26571 = ORIENTED_EDGE('',*,*,#18568,.T.) ;
#26572 = ORIENTED_EDGE('',*,*,#18534,.F.) ;
#26573 = ORIENTED_EDGE('',*,*,#18569,.F.) ;
#26574 = ORIENTED_EDGE('',*,*,#18535,.F.) ;
#26575 = ORIENTED_EDGE('',*,*,#18568,.F.) ;
#26576 = ORIENTED_EDGE('',*,*,#18531,.F.) ;
#26577 = ORIENTED_EDGE('',*,*,#18569,.T.) ;
#26578 = ORIENTED_EDGE('',*,*,#18537,.F.) ;
#26579 = ORIENTED_EDGE('',*,*,#18570,.T.) ;
#26580 = ORIENTED_EDGE('',*,*,#18538,.F.) ;
#26581 = ORIENTED_EDGE('',*,*,#18571,.F.) ;
#26582 = ORIENTED_EDGE('',*,*,#18539,.F.) ;
#26583 = ORIENTED_EDGE('',*,*,#18570,.F.) ;
#26584 = ORIENTED_EDGE('',*,*,#18536,.F.) ;
#26585 = ORIENTED_EDGE('',*,*,#18571,.T.) ;
#26586 = ORIENTED_EDGE('',*,*,#18541,.F.) ;
#26587 = ORIENTED_EDGE('',*,*,#18572,.T.) ;
#26588 = ORIENTED_EDGE('',*,*,#18542,.F.) ;
#26589 = ORIENTED_EDGE('',*,*,#18573,.F.) ;
#26590 = ORIENTED_EDGE('',*,*,#18543,.F.) ;
#26591 = ORIENTED_EDGE('',*,*,#18572,.F.) ;
#26592 = ORIENTED_EDGE('',*,*,#18540,.F.) ;
#26593 = ORIENTED_EDGE('',*,*,#18573,.T.) ;
#26594 = ORIENTED_EDGE('',*,*,#18545,.F.) ;
#26595 = ORIENTED_EDGE('',*,*,#18574,.T.) ;
#26596 = ORIENTED_EDGE('',*,*,#18546,.F.) ;
#26597 = ORIENTED_EDGE('',*,*,#18575,.F.) ;
#26598 = ORIENTED_EDGE('',*,*,#18547,.F.) ;
#26599 = ORIENTED_EDGE('',*,*,#18574,.F.) ;
#26600 = ORIENTED_EDGE('',*,*,#18544,.F.) ;
#26601 = ORIENTED_EDGE('',*,*,#18575,.T.) ;
#26602 = ORIENTED_EDGE('',*,*,#18549,.F.) ;
#26603 = ORIENTED_EDGE('',*,*,#18576,.T.) ;
#26604 = ORIENTED_EDGE('',*,*,#18550,.F.) ;
#26605 = ORIENTED_EDGE('',*,*,#18577,.F.) ;
#26606 = ORIENTED_EDGE('',*,*,#18551,.F.) ;
#26607 = ORIENTED_EDGE('',*,*,#18576,.F.) ;
#26608 = ORIENTED_EDGE('',*,*,#18548,.F.) ;
#26609 = ORIENTED_EDGE('',*,*,#18577,.T.) ;
#26610 = ORIENTED_EDGE('',*,*,#18553,.F.) ;
#26611 = ORIENTED_EDGE('',*,*,#18578,.T.) ;
#26612 = ORIENTED_EDGE('',*,*,#18579,.F.) ;
#26613 = ORIENTED_EDGE('',*,*,#18580,.F.) ;
#26614 = ORIENTED_EDGE('',*,*,#18523,.F.) ;
#26615 = ORIENTED_EDGE('',*,*,#18518,.F.) ;
#26616 = ORIENTED_EDGE('',*,*,#18581,.F.) ;
#26617 = ORIENTED_EDGE('',*,*,#18582,.F.) ;
#26618 = ORIENTED_EDGE('',*,*,#18578,.F.) ;
#26619 = ORIENTED_EDGE('',*,*,#18552,.F.) ;
#26620 = ORIENTED_EDGE('',*,*,#18520,.T.) ;
#26621 = ORIENTED_EDGE('',*,*,#18583,.T.) ;
#26622 = ORIENTED_EDGE('',*,*,#18584,.F.) ;
#26623 = ORIENTED_EDGE('',*,*,#18555,.F.) ;
#26624 = ORIENTED_EDGE('',*,*,#18585,.F.) ;
#26625 = ORIENTED_EDGE('',*,*,#18583,.F.) ;
#26626 = ORIENTED_EDGE('',*,*,#18522,.T.) ;
#26627 = ORIENTED_EDGE('',*,*,#18554,.F.) ;
#26628 = ORIENTED_EDGE('',*,*,#18584,.T.) ;
#26629 = ORIENTED_EDGE('',*,*,#18586,.T.) ;
#26630 = ORIENTED_EDGE('',*,*,#18558,.T.) ;
#26631 = ORIENTED_EDGE('',*,*,#18525,.F.) ;
#26632 = ORIENTED_EDGE('',*,*,#18557,.T.) ;
#26633 = ORIENTED_EDGE('',*,*,#18586,.F.) ;
#26634 = ORIENTED_EDGE('',*,*,#18585,.T.) ;
#26635 = ORIENTED_EDGE('',*,*,#18556,.F.) ;
#26636 = ORIENTED_EDGE('',*,*,#18581,.T.) ;
#26637 = ORIENTED_EDGE('',*,*,#18517,.T.) ;
#26638 = ORIENTED_EDGE('',*,*,#18587,.T.) ;
#26639 = ORIENTED_EDGE('',*,*,#18579,.T.) ;
#26640 = ORIENTED_EDGE('',*,*,#18588,.T.) ;
#26641 = ORIENTED_EDGE('',*,*,#18589,.F.) ;
#26642 = ORIENTED_EDGE('',*,*,#18588,.F.) ;
#26643 = ORIENTED_EDGE('',*,*,#18582,.T.) ;
#26644 = ORIENTED_EDGE('',*,*,#18587,.F.) ;
#26645 = ORIENTED_EDGE('',*,*,#18516,.T.) ;
#26646 = ORIENTED_EDGE('',*,*,#18590,.F.) ;
#26647 = ORIENTED_EDGE('',*,*,#18589,.T.) ;
#26648 = ORIENTED_EDGE('',*,*,#18580,.T.) ;
#26649 = ORIENTED_EDGE('',*,*,#18590,.T.) ;
#26650 = ORIENTED_EDGE('',*,*,#18515,.T.) ;
#26651 = CYLINDRICAL_SURFACE('',#29214,0.62) ;
#26652 = CYLINDRICAL_SURFACE('',#29226,55.) ;
#26653 = CYLINDRICAL_SURFACE('',#29232,0.62) ;
#26654 = CYLINDRICAL_SURFACE('',#29299,53.4) ;
#26655 = CYLINDRICAL_SURFACE('',#29302,53.4) ;
#26656 = CYLINDRICAL_SURFACE('',#29321,55.05) ;
#26657 = CYLINDRICAL_SURFACE('',#29326,55.5) ;
#26658 = CYLINDRICAL_SURFACE('',#29336,0.6) ;
#26659 = CYLINDRICAL_SURFACE('',#29354,51.5) ;
#26660 = CYLINDRICAL_SURFACE('',#29357,51.5) ;
#26661 = CYLINDRICAL_SURFACE('',#29360,50.5) ;
#26662 = CYLINDRICAL_SURFACE('',#29417,50.5) ;
#26663 = CYLINDRICAL_SURFACE('',#29464,51.5) ;
#26664 = CYLINDRICAL_SURFACE('',#29465,51.5) ;
#26665 = CYLINDRICAL_SURFACE('',#29483,50.5) ;
#26666 = CYLINDRICAL_SURFACE('',#29484,51.5) ;
#26667 = CYLINDRICAL_SURFACE('',#29490,50.5) ;
#26668 = CYLINDRICAL_SURFACE('',#29491,51.5) ;
#26669 = CYLINDRICAL_SURFACE('',#29492,51.5) ;
#26670 = CYLINDRICAL_SURFACE('',#29510,51.5) ;
#26671 = CYLINDRICAL_SURFACE('',#29519,51.5) ;
#26672 = CYLINDRICAL_SURFACE('',#29539,50.5) ;
#26673 = CYLINDRICAL_SURFACE('',#29540,51.5) ;
#26674 = CYLINDRICAL_SURFACE('',#29542,51.5) ;
#26675 = CYLINDRICAL_SURFACE('',#29543,51.5) ;
#26676 = CYLINDRICAL_SURFACE('',#29566,51.5) ;
#26677 = CYLINDRICAL_SURFACE('',#29567,51.5) ;
#26678 = CYLINDRICAL_SURFACE('',#29568,50.5) ;
#26679 = CYLINDRICAL_SURFACE('',#29569,50.5) ;
#26680 = CYLINDRICAL_SURFACE('',#29594,50.5) ;
#26681 = CYLINDRICAL_SURFACE('',#29595,50.5) ;
#26682 = CYLINDRICAL_SURFACE('',#29596,51.5) ;
#26683 = CYLINDRICAL_SURFACE('',#29603,50.5) ;
#26684 = CYLINDRICAL_SURFACE('',#29604,51.5) ;
#26685 = CYLINDRICAL_SURFACE('',#29623,50.5) ;
#26686 = CYLINDRICAL_SURFACE('',#29624,51.5) ;
#26687 = CYLINDRICAL_SURFACE('',#29627,51.5) ;
#26688 = CYLINDRICAL_SURFACE('',#29628,51.5) ;
#26689 = CYLINDRICAL_SURFACE('',#29629,50.5) ;
#26690 = CYLINDRICAL_SURFACE('',#29652,50.5) ;
#26691 = CYLINDRICAL_SURFACE('',#29655,50.5) ;
#26692 = CYLINDRICAL_SURFACE('',#29656,50.5) ;
#26693 = CYLINDRICAL_SURFACE('',#29657,51.5) ;
#26694 = CYLINDRICAL_SURFACE('',#29674,51.5) ;
#26695 = CYLINDRICAL_SURFACE('',#29677,51.5) ;
#26696 = CYLINDRICAL_SURFACE('',#29678,50.5) ;
#26697 = CYLINDRICAL_SURFACE('',#29690,50.5) ;
#26698 = CYLINDRICAL_SURFACE('',#29691,51.5) ;
#26699 = CYLINDRICAL_SURFACE('',#29692,51.5) ;
#26700 = CYLINDRICAL_SURFACE('',#29695,51.5) ;
#26701 = CYLINDRICAL_SURFACE('',#29696,50.5) ;
#26702 = CYLINDRICAL_SURFACE('',#29706,50.5) ;
#26703 = CYLINDRICAL_SURFACE('',#29708,51.5) ;
#26704 = CYLINDRICAL_SURFACE('',#29716,51.5) ;
#26705 = CYLINDRICAL_SURFACE('',#29722,51.5) ;
#26706 = CYLINDRICAL_SURFACE('',#29723,50.5) ;
#26707 = CYLINDRICAL_SURFACE('',#29843,2.) ;
#26708 = CYLINDRICAL_SURFACE('',#29848,2.) ;
#26709 = CYLINDRICAL_SURFACE('',#29851,2.) ;
#26710 = CYLINDRICAL_SURFACE('',#29854,2.) ;
#26711 = CYLINDRICAL_SURFACE('',#29857,2.) ;
#26712 = CYLINDRICAL_SURFACE('',#29860,2.) ;
#26713 = CYLINDRICAL_SURFACE('',#29863,2.) ;
#26714 = CYLINDRICAL_SURFACE('',#29866,2.) ;
#26715 = CYLINDRICAL_SURFACE('',#29868,2.) ;
#26716 = CYLINDRICAL_SURFACE('',#29870,2.) ;
#26717 = CYLINDRICAL_SURFACE('',#29872,2.) ;
#26718 = CYLINDRICAL_SURFACE('',#29874,2.) ;
#26719 = CYLINDRICAL_SURFACE('',#29876,2.) ;
#26720 = CYLINDRICAL_SURFACE('',#29878,2.) ;
#26721 = CYLINDRICAL_SURFACE('',#29880,2.) ;
#26722 = CYLINDRICAL_SURFACE('',#29882,2.) ;
#26723 = CYLINDRICAL_SURFACE('',#29884,2.) ;
#26724 = CYLINDRICAL_SURFACE('',#29886,2.) ;
#26725 = CYLINDRICAL_SURFACE('',#29888,2.) ;
#26726 = CYLINDRICAL_SURFACE('',#29890,2.) ;
#26727 = CYLINDRICAL_SURFACE('',#29892,2.) ;
#26728 = CYLINDRICAL_SURFACE('',#29895,2.) ;
#26729 = CYLINDRICAL_SURFACE('',#29898,2.) ;
#26730 = CYLINDRICAL_SURFACE('',#29901,2.) ;
#26731 = CYLINDRICAL_SURFACE('',#29904,2.) ;
#26732 = CYLINDRICAL_SURFACE('',#29907,2.) ;
#26733 = CYLINDRICAL_SURFACE('',#29910,2.) ;
#26734 = CYLINDRICAL_SURFACE('',#29913,2.) ;
#26735 = CYLINDRICAL_SURFACE('',#29922,0.65) ;
#26736 = CYLINDRICAL_SURFACE('',#29925,0.65) ;
#26737 = CYLINDRICAL_SURFACE('',#29928,0.65) ;
#26738 = CYLINDRICAL_SURFACE('',#29931,0.65) ;
#26739 = CYLINDRICAL_SURFACE('',#29934,0.65) ;
#26740 = CYLINDRICAL_SURFACE('',#29937,0.65) ;
#26741 = CYLINDRICAL_SURFACE('',#29940,3.) ;
#26742 = CYLINDRICAL_SURFACE('',#29950,0.65) ;
#26743 = CYLINDRICAL_SURFACE('',#29953,0.65) ;
#26744 = CYLINDRICAL_SURFACE('',#29956,3.) ;
#26745 = CYLINDRICAL_SURFACE('',#29966,1.28) ;
#26746 = CYLINDRICAL_SURFACE('',#29969,1.28) ;
#26747 = CYLINDRICAL_SURFACE('',#29972,1.2) ;
#26748 = CYLINDRICAL_SURFACE('',#29975,1.5) ;
#26749 = CYLINDRICAL_SURFACE('',#29981,1.2) ;
#26750 = CYLINDRICAL_SURFACE('',#29984,1.5) ;
#26751 = CYLINDRICAL_SURFACE('',#30048,3.) ;
#26752 = CYLINDRICAL_SURFACE('',#30049,3.) ;
#26753 = CYLINDRICAL_SURFACE('',#30050,2.6) ;
#26754 = CYLINDRICAL_SURFACE('',#30051,2.6) ;
#26755 = CYLINDRICAL_SURFACE('',#30074,1.5) ;
#26756 = CYLINDRICAL_SURFACE('',#30076,1.2) ;
#26757 = CYLINDRICAL_SURFACE('',#30082,1.5) ;
#26758 = CYLINDRICAL_SURFACE('',#30083,1.2) ;
#26759 = CYLINDRICAL_SURFACE('',#30084,3.) ;
#26760 = CYLINDRICAL_SURFACE('',#30106,3.) ;
#26761 = CYLINDRICAL_SURFACE('',#30121,3.) ;
#26762 = CYLINDRICAL_SURFACE('',#30127,2.6) ;
#26763 = CYLINDRICAL_SURFACE('',#30134,3.) ;
#26764 = CYLINDRICAL_SURFACE('',#30140,3.) ;
#26765 = CYLINDRICAL_SURFACE('',#30148,3.) ;
#26766 = CYLINDRICAL_SURFACE('',#30153,3.) ;
#26767 = CYLINDRICAL_SURFACE('',#30157,3.) ;
#26768 = CYLINDRICAL_SURFACE('',#30167,3.) ;
#26769 = CYLINDRICAL_SURFACE('',#30175,2.6) ;
#26770 = CYLINDRICAL_SURFACE('',#30176,2.6) ;
#26771 = CYLINDRICAL_SURFACE('',#30187,2.6) ;
#26772 = CYLINDRICAL_SURFACE('',#30188,2.6) ;
#26773 = CYLINDRICAL_SURFACE('',#30197,2.6) ;
#26774 = CYLINDRICAL_SURFACE('',#30226,2.6) ;
#26775 = CYLINDRICAL_SURFACE('',#30235,2.6) ;
#26776 = CYLINDRICAL_SURFACE('',#30254,0.35) ;
#26777 = CYLINDRICAL_SURFACE('',#30258,2.25) ;
#26778 = CYLINDRICAL_SURFACE('',#30261,1.4) ;
#26779 = CYLINDRICAL_SURFACE('',#30265,0.35) ;
#26780 = CYLINDRICAL_SURFACE('',#30269,2.) ;
#26781 = CYLINDRICAL_SURFACE('',#30272,1.25) ;
#26782 = CYLINDRICAL_SURFACE('',#30285,0.65) ;
#26783 = CYLINDRICAL_SURFACE('',#30288,0.65) ;
#26784 = CYLINDRICAL_SURFACE('',#30291,0.65) ;
#26785 = CYLINDRICAL_SURFACE('',#30294,0.65) ;
#26786 = CYLINDRICAL_SURFACE('',#30297,0.425) ;
#26787 = CYLINDRICAL_SURFACE('',#30312,0.425) ;
#26788 = CYLINDRICAL_SURFACE('',#30317,0.425) ;
#26789 = CYLINDRICAL_SURFACE('',#30322,0.425) ;
#26790 = CYLINDRICAL_SURFACE('',#30323,0.5) ;
#26791 = CYLINDRICAL_SURFACE('',#30327,1.) ;
#26792 = CYLINDRICAL_SURFACE('',#30330,1.02) ;
#26793 = CYLINDRICAL_SURFACE('',#30333,1.02) ;
#26794 = CYLINDRICAL_SURFACE('',#30351,7.) ;
#26795 = CYLINDRICAL_SURFACE('',#30353,2.5) ;
#26796 = CYLINDRICAL_SURFACE('',#30355,1.02) ;
#26797 = CYLINDRICAL_SURFACE('',#30360,1.51) ;
#26798 = CYLINDRICAL_SURFACE('',#30364,3.) ;
#26799 = CYLINDRICAL_SURFACE('',#30368,1.77) ;
#26800 = CYLINDRICAL_SURFACE('',#30372,3.5) ;
#26801 = CYLINDRICAL_SURFACE('',#30395,0.49) ;
#26802 = CYLINDRICAL_SURFACE('',#30426,1.55) ;
#26803 = CYLINDRICAL_SURFACE('',#30428,1.55) ;
#26804 = CYLINDRICAL_SURFACE('',#30430,1.55) ;
#26805 = CYLINDRICAL_SURFACE('',#30432,1.55) ;
#26806 = CYLINDRICAL_SURFACE('',#30434,1.55) ;
#26807 = CYLINDRICAL_SURFACE('',#30436,1.55) ;
#26808 = CYLINDRICAL_SURFACE('',#30463,1.75) ;
#26809 = CYLINDRICAL_SURFACE('',#30465,1.75) ;
#26810 = CYLINDRICAL_SURFACE('',#30467,1.75) ;
#26811 = CYLINDRICAL_SURFACE('',#30469,1.75) ;
#26812 = CYLINDRICAL_SURFACE('',#30471,1.75) ;
#26813 = CYLINDRICAL_SURFACE('',#30473,1.75) ;
#26814 = CYLINDRICAL_SURFACE('',#30486,1.75) ;
#26815 = CYLINDRICAL_SURFACE('',#30500,1.75) ;
#26816 = CYLINDRICAL_SURFACE('',#30506,2.2) ;
#26817 = CYLINDRICAL_SURFACE('',#30510,1.75) ;
#26818 = CYLINDRICAL_SURFACE('',#30513,2.5) ;
#26819 = CYLINDRICAL_SURFACE('',#30525,4.6) ;
#26820 = CYLINDRICAL_SURFACE('',#30529,4.2) ;
#26821 = CYLINDRICAL_SURFACE('',#30540,1.5) ;
#26822 = CYLINDRICAL_SURFACE('',#30546,0.8) ;
#26823 = CYLINDRICAL_SURFACE('',#30550,1.5) ;
#26824 = CYLINDRICAL_SURFACE('',#30553,4.5) ;
#26825 = CYLINDRICAL_SURFACE('',#30559,0.61) ;
#26826 = CYLINDRICAL_SURFACE('',#30562,1.1) ;
#26827 = CYLINDRICAL_SURFACE('',#30567,0.81) ;
#26828 = CYLINDRICAL_SURFACE('',#30570,1.4) ;
#26829 = CYLINDRICAL_SURFACE('',#30575,0.6) ;
#26830 = CYLINDRICAL_SURFACE('',#30587,1.6) ;
#26831 = CYLINDRICAL_SURFACE('',#30588,1.) ;
#26832 = CYLINDRICAL_SURFACE('',#30650,1.) ;
#26833 = CYLINDRICAL_SURFACE('',#30655,1.) ;
#26834 = CYLINDRICAL_SURFACE('',#30658,1.6) ;
#26835 = CYLINDRICAL_SURFACE('',#30675,0.26) ;
#26836 = CYLINDRICAL_SURFACE('',#30685,0.41) ;
#26837 = CYLINDRICAL_SURFACE('',#30693,0.425) ;
#26838 = CYLINDRICAL_SURFACE('',#30696,0.425) ;
#26839 = CYLINDRICAL_SURFACE('',#30699,0.425) ;
#26840 = CYLINDRICAL_SURFACE('',#30702,0.425) ;
#26841 = CYLINDRICAL_SURFACE('',#30705,1.05) ;
#26842 = CYLINDRICAL_SURFACE('',#30725,2.55) ;
#26843 = CYLINDRICAL_SURFACE('',#30729,6.5) ;
#26844 = CYLINDRICAL_SURFACE('',#30742,0.25) ;
#26845 = CYLINDRICAL_SURFACE('',#30750,0.3) ;
#26846 = CYLINDRICAL_SURFACE('',#30758,4.5) ;
#26847 = CYLINDRICAL_SURFACE('',#30809,0.425) ;
#26848 = CYLINDRICAL_SURFACE('',#30812,0.425) ;
#26849 = CYLINDRICAL_SURFACE('',#30815,0.425) ;
#26850 = CYLINDRICAL_SURFACE('',#30818,0.425) ;
#26851 = CYLINDRICAL_SURFACE('',#30821,2.55) ;
#26852 = CYLINDRICAL_SURFACE('',#30826,6.2) ;
#26853 = CYLINDRICAL_SURFACE('',#30842,6.3) ;
#26854 = CYLINDRICAL_SURFACE('',#30845,6.3) ;
#26855 = CYLINDRICAL_SURFACE('',#30847,6.8) ;
#26856 = CYLINDRICAL_SURFACE('',#30861,0.4) ;
#26857 = CYLINDRICAL_SURFACE('',#30864,0.4) ;
#26858 = CYLINDRICAL_SURFACE('',#30867,0.4) ;
#26859 = CYLINDRICAL_SURFACE('',#30870,0.4) ;
#26860 = CYLINDRICAL_SURFACE('',#30873,0.4) ;
#26861 = CYLINDRICAL_SURFACE('',#30876,0.4) ;
#26862 = CYLINDRICAL_SURFACE('',#30879,0.4) ;
#26863 = CYLINDRICAL_SURFACE('',#30882,0.51) ;
#26864 = CYLINDRICAL_SURFACE('',#30890,8.) ;
#26865 = CYLINDRICAL_SURFACE('',#30892,0.4) ;
#26866 = CYLINDRICAL_SURFACE('',#30899,0.31) ;
#26867 = CYLINDRICAL_SURFACE('',#30905,0.15) ;
#26868 = CYLINDRICAL_SURFACE('',#30907,0.51) ;
#26869 = CYLINDRICAL_SURFACE('',#30926,0.7) ;
#26870 = CYLINDRICAL_SURFACE('',#30936,0.8) ;
#26871 = CYLINDRICAL_SURFACE('',#30939,0.5) ;
#26872 = CYLINDRICAL_SURFACE('',#30951,0.15) ;
#26873 = CYLINDRICAL_SURFACE('',#30969,0.15) ;
#26874 = CYLINDRICAL_SURFACE('',#30971,0.15) ;
#26875 = CYLINDRICAL_SURFACE('',#30974,0.4) ;
#26876 = CYLINDRICAL_SURFACE('',#30980,0.4) ;
#26877 = CYLINDRICAL_SURFACE('',#30985,0.4) ;
#26878 = CYLINDRICAL_SURFACE('',#30987,0.4) ;
#26879 = CYLINDRICAL_SURFACE('',#30990,0.4) ;
#26880 = CYLINDRICAL_SURFACE('',#30994,0.4) ;
#26881 = CYLINDRICAL_SURFACE('',#30995,0.4) ;
#26882 = CYLINDRICAL_SURFACE('',#31007,0.15) ;
#26883 = CYLINDRICAL_SURFACE('',#31008,0.4) ;
#26884 = CYLINDRICAL_SURFACE('',#31015,0.4) ;
#26885 = CYLINDRICAL_SURFACE('',#31016,0.4) ;
#26886 = CYLINDRICAL_SURFACE('',#31018,0.15) ;
#26887 = CYLINDRICAL_SURFACE('',#31027,0.4) ;
#26888 = CYLINDRICAL_SURFACE('',#31029,0.15) ;
#26889 = CYLINDRICAL_SURFACE('',#31032,0.4) ;
#26890 = CYLINDRICAL_SURFACE('',#31037,0.125) ;
#26891 = CYLINDRICAL_SURFACE('',#31049,0.125) ;
#26892 = CYLINDRICAL_SURFACE('',#31052,0.125) ;
#26893 = CYLINDRICAL_SURFACE('',#31058,0.29) ;
#26894 = CYLINDRICAL_SURFACE('',#31064,0.29) ;
#26895 = CYLINDRICAL_SURFACE('',#31070,0.55) ;
#26896 = CYLINDRICAL_SURFACE('',#31073,0.25) ;
#26897 = CYLINDRICAL_SURFACE('',#31078,0.15) ;
#26898 = CYLINDRICAL_SURFACE('',#31081,0.8) ;
#26899 = CYLINDRICAL_SURFACE('',#31084,1.1) ;
#26900 = CYLINDRICAL_SURFACE('',#31089,0.8) ;
#26901 = CYLINDRICAL_SURFACE('',#31093,1.1) ;
#26902 = CYLINDRICAL_SURFACE('',#31674,0.15) ;
#26903 = CYLINDRICAL_SURFACE('',#31676,0.15) ;
#26904 = CYLINDRICAL_SURFACE('',#31678,0.15) ;
#26905 = CYLINDRICAL_SURFACE('',#31681,0.15) ;
#26906 = CYLINDRICAL_SURFACE('',#31684,0.15) ;
#26907 = CYLINDRICAL_SURFACE('',#31687,0.15) ;
#26908 = CYLINDRICAL_SURFACE('',#31690,0.15) ;
#26909 = CYLINDRICAL_SURFACE('',#31693,0.15) ;
#26910 = CYLINDRICAL_SURFACE('',#31696,0.15) ;
#26911 = CYLINDRICAL_SURFACE('',#31699,0.15) ;
#26912 = CYLINDRICAL_SURFACE('',#31702,0.15) ;
#26913 = CYLINDRICAL_SURFACE('',#31705,0.15) ;
#26914 = CYLINDRICAL_SURFACE('',#31708,0.15) ;
#26915 = CYLINDRICAL_SURFACE('',#31711,0.15) ;
#26916 = CYLINDRICAL_SURFACE('',#31714,0.15) ;
#26917 = CYLINDRICAL_SURFACE('',#31717,0.15) ;
#26918 = CYLINDRICAL_SURFACE('',#31720,0.15) ;
#26919 = CYLINDRICAL_SURFACE('',#31723,0.15) ;
#26920 = CYLINDRICAL_SURFACE('',#31726,0.15) ;
#26921 = CYLINDRICAL_SURFACE('',#31729,0.15) ;
#26922 = CYLINDRICAL_SURFACE('',#31732,0.15) ;
#26923 = CYLINDRICAL_SURFACE('',#31735,0.15) ;
#26924 = CYLINDRICAL_SURFACE('',#31738,0.15) ;
#26925 = CYLINDRICAL_SURFACE('',#31741,0.15) ;
#26926 = CYLINDRICAL_SURFACE('',#31744,0.15) ;
#26927 = CYLINDRICAL_SURFACE('',#31747,0.15) ;
#26928 = CYLINDRICAL_SURFACE('',#31750,0.15) ;
#26929 = CYLINDRICAL_SURFACE('',#31753,0.15) ;
#26930 = CYLINDRICAL_SURFACE('',#31756,0.15) ;
#26931 = CYLINDRICAL_SURFACE('',#31759,0.15) ;
#26932 = CYLINDRICAL_SURFACE('',#31762,0.15) ;
#26933 = CYLINDRICAL_SURFACE('',#31765,0.15) ;
#26934 = CYLINDRICAL_SURFACE('',#31768,0.15) ;
#26935 = CYLINDRICAL_SURFACE('',#31771,0.15) ;
#26936 = CYLINDRICAL_SURFACE('',#31774,0.15) ;
#26937 = CYLINDRICAL_SURFACE('',#31777,0.15) ;
#26938 = CYLINDRICAL_SURFACE('',#31780,0.15) ;
#26939 = CYLINDRICAL_SURFACE('',#31783,0.15) ;
#26940 = CYLINDRICAL_SURFACE('',#31786,0.15) ;
#26941 = CYLINDRICAL_SURFACE('',#31789,0.15) ;
#26942 = CYLINDRICAL_SURFACE('',#31792,0.15) ;
#26943 = CYLINDRICAL_SURFACE('',#31795,0.15) ;
#26944 = CYLINDRICAL_SURFACE('',#31798,0.15) ;
#26945 = CYLINDRICAL_SURFACE('',#31801,0.15) ;
#26946 = CYLINDRICAL_SURFACE('',#31804,0.15) ;
#26947 = CYLINDRICAL_SURFACE('',#31807,0.15) ;
#26948 = CYLINDRICAL_SURFACE('',#31810,0.15) ;
#26949 = CYLINDRICAL_SURFACE('',#31813,0.15) ;
#26950 = CYLINDRICAL_SURFACE('',#31816,0.15) ;
#26951 = CYLINDRICAL_SURFACE('',#31819,0.15) ;
#26952 = CYLINDRICAL_SURFACE('',#31822,0.15) ;
#26953 = CYLINDRICAL_SURFACE('',#31825,0.15) ;
#26954 = CYLINDRICAL_SURFACE('',#31828,0.15) ;
#26955 = CYLINDRICAL_SURFACE('',#31831,0.15) ;
#26956 = CYLINDRICAL_SURFACE('',#31834,0.15) ;
#26957 = CYLINDRICAL_SURFACE('',#31837,0.15) ;
#26958 = CYLINDRICAL_SURFACE('',#31840,0.15) ;
#26959 = CYLINDRICAL_SURFACE('',#31843,0.15) ;
#26960 = CYLINDRICAL_SURFACE('',#31846,0.15) ;
#26961 = CYLINDRICAL_SURFACE('',#31849,0.15) ;
#26962 = CYLINDRICAL_SURFACE('',#31852,0.15) ;
#26963 = CYLINDRICAL_SURFACE('',#31855,0.15) ;
#26964 = CYLINDRICAL_SURFACE('',#31858,0.15) ;
#26965 = CYLINDRICAL_SURFACE('',#31861,0.15) ;
#26966 = CYLINDRICAL_SURFACE('',#31864,0.15) ;
#26967 = CYLINDRICAL_SURFACE('',#31867,0.15) ;
#26968 = CYLINDRICAL_SURFACE('',#31870,0.15) ;
#26969 = CYLINDRICAL_SURFACE('',#31873,0.15) ;
#26970 = CYLINDRICAL_SURFACE('',#31876,0.15) ;
#26971 = CYLINDRICAL_SURFACE('',#31879,0.15) ;
#26972 = CYLINDRICAL_SURFACE('',#31882,0.15) ;
#26973 = CYLINDRICAL_SURFACE('',#31885,0.15) ;
#26974 = CYLINDRICAL_SURFACE('',#31888,0.15) ;
#26975 = CYLINDRICAL_SURFACE('',#31891,0.15) ;
#26976 = CYLINDRICAL_SURFACE('',#31894,0.15) ;
#26977 = CYLINDRICAL_SURFACE('',#31897,0.15) ;
#26978 = CYLINDRICAL_SURFACE('',#31900,0.15) ;
#26979 = CYLINDRICAL_SURFACE('',#31903,0.15) ;
#26980 = CYLINDRICAL_SURFACE('',#31906,0.15) ;
#26981 = CYLINDRICAL_SURFACE('',#31909,0.15) ;
#26982 = CYLINDRICAL_SURFACE('',#31912,0.15) ;
#26983 = CYLINDRICAL_SURFACE('',#31915,0.15) ;
#26984 = CYLINDRICAL_SURFACE('',#31918,0.15) ;
#26985 = CYLINDRICAL_SURFACE('',#31921,0.15) ;
#26986 = CYLINDRICAL_SURFACE('',#31924,0.15) ;
#26987 = CYLINDRICAL_SURFACE('',#31927,0.15) ;
#26988 = CYLINDRICAL_SURFACE('',#31930,0.15) ;
#26989 = CYLINDRICAL_SURFACE('',#31933,0.15) ;
#26990 = CYLINDRICAL_SURFACE('',#31936,0.15) ;
#26991 = CYLINDRICAL_SURFACE('',#31939,0.15) ;
#26992 = CYLINDRICAL_SURFACE('',#31942,0.15) ;
#26993 = CYLINDRICAL_SURFACE('',#31945,0.15) ;
#26994 = CYLINDRICAL_SURFACE('',#31948,0.15) ;
#26995 = CYLINDRICAL_SURFACE('',#31951,0.15) ;
#26996 = CYLINDRICAL_SURFACE('',#31954,0.15) ;
#26997 = CYLINDRICAL_SURFACE('',#31957,0.15) ;
#26998 = CYLINDRICAL_SURFACE('',#31960,0.15) ;
#26999 = CYLINDRICAL_SURFACE('',#31963,0.15) ;
#27000 = CYLINDRICAL_SURFACE('',#31966,0.15) ;
#27001 = CYLINDRICAL_SURFACE('',#31969,0.15) ;
#27002 = CYLINDRICAL_SURFACE('',#31972,0.15) ;
#27003 = CYLINDRICAL_SURFACE('',#31975,0.15) ;
#27004 = CYLINDRICAL_SURFACE('',#31978,0.15) ;
#27005 = CYLINDRICAL_SURFACE('',#31981,0.15) ;
#27006 = CYLINDRICAL_SURFACE('',#31984,0.15) ;
#27007 = CYLINDRICAL_SURFACE('',#31987,0.15) ;
#27008 = CYLINDRICAL_SURFACE('',#31990,0.15) ;
#27009 = CYLINDRICAL_SURFACE('',#31993,0.15) ;
#27010 = CYLINDRICAL_SURFACE('',#31996,0.15) ;
#27011 = CYLINDRICAL_SURFACE('',#31999,0.15) ;
#27012 = CYLINDRICAL_SURFACE('',#32002,0.15) ;
#27013 = CYLINDRICAL_SURFACE('',#32005,0.15) ;
#27014 = CYLINDRICAL_SURFACE('',#32008,0.15) ;
#27015 = CYLINDRICAL_SURFACE('',#32011,0.15) ;
#27016 = CYLINDRICAL_SURFACE('',#32014,0.15) ;
#27017 = CYLINDRICAL_SURFACE('',#32017,0.15) ;
#27018 = CYLINDRICAL_SURFACE('',#32020,0.15) ;
#27019 = CYLINDRICAL_SURFACE('',#32023,0.15) ;
#27020 = CYLINDRICAL_SURFACE('',#32026,0.15) ;
#27021 = CYLINDRICAL_SURFACE('',#32029,0.15) ;
#27022 = CYLINDRICAL_SURFACE('',#32032,0.15) ;
#27023 = CYLINDRICAL_SURFACE('',#32035,0.15) ;
#27024 = CYLINDRICAL_SURFACE('',#32038,0.15) ;
#27025 = CYLINDRICAL_SURFACE('',#32041,0.15) ;
#27026 = CYLINDRICAL_SURFACE('',#32044,0.15) ;
#27027 = CYLINDRICAL_SURFACE('',#32047,0.15) ;
#27028 = CYLINDRICAL_SURFACE('',#32050,0.15) ;
#27029 = CYLINDRICAL_SURFACE('',#32053,0.15) ;
#27030 = CYLINDRICAL_SURFACE('',#32056,0.55) ;
#27031 = CYLINDRICAL_SURFACE('',#32059,0.25) ;
#27032 = CYLINDRICAL_SURFACE('',#32064,0.15) ;
#27033 = CYLINDRICAL_SURFACE('',#32088,3.3) ;
#27034 = CYLINDRICAL_SURFACE('',#32090,3.3) ;
#27035 = CYLINDRICAL_SURFACE('',#32094,3.5) ;
#27036 = CYLINDRICAL_SURFACE('',#32096,3.5) ;
#27037 = CYLINDRICAL_SURFACE('',#32103,3.5) ;
#27038 = CYLINDRICAL_SURFACE('',#32105,3.5) ;
#27039 = CYLINDRICAL_SURFACE('',#32108,3.3) ;
#27040 = CYLINDRICAL_SURFACE('',#32111,3.3) ;
#27041 = CYLINDRICAL_SURFACE('',#32119,0.6) ;
#27042 = CYLINDRICAL_SURFACE('',#32134,1.) ;
#27043 = CYLINDRICAL_SURFACE('',#32137,0.32) ;
#27044 = CYLINDRICAL_SURFACE('',#32138,0.32) ;
#27045 = CYLINDRICAL_SURFACE('',#32141,1.) ;
#27046 = CYLINDRICAL_SURFACE('',#32146,4.5) ;
#27047 = CYLINDRICAL_SURFACE('',#32155,4.5) ;
#27048 = CYLINDRICAL_SURFACE('',#32156,3.5) ;
#27049 = CYLINDRICAL_SURFACE('',#32158,1.) ;
#27050 = CYLINDRICAL_SURFACE('',#32161,1.02) ;
#27051 = CYLINDRICAL_SURFACE('',#32167,3.5) ;
#27052 = CYLINDRICAL_SURFACE('',#32195,3.5) ;
#27053 = CYLINDRICAL_SURFACE('',#32197,3.8) ;
#27054 = CYLINDRICAL_SURFACE('',#32208,0.6) ;
#27055 = CYLINDRICAL_SURFACE('',#32221,0.6) ;
#27056 = CYLINDRICAL_SURFACE('',#32233,0.4) ;
#27057 = CYLINDRICAL_SURFACE('',#32246,0.5) ;
#27058 = CYLINDRICAL_SURFACE('',#32261,0.45) ;
#27059 = CYLINDRICAL_SURFACE('',#32264,0.245) ;
#27060 = CYLINDRICAL_SURFACE('',#32271,0.45) ;
#27061 = CYLINDRICAL_SURFACE('',#32274,0.245) ;
#27062 = CYLINDRICAL_SURFACE('',#32278,0.25) ;
#27063 = CYLINDRICAL_SURFACE('',#32330,0.25) ;
#27064 = CYLINDRICAL_SURFACE('',#32335,0.25) ;
#27065 = CYLINDRICAL_SURFACE('',#32338,0.25) ;
#27066 = CYLINDRICAL_SURFACE('',#32341,0.25) ;
#27067 = CYLINDRICAL_SURFACE('',#32343,0.25) ;
#27068 = CYLINDRICAL_SURFACE('',#32345,0.25) ;
#27069 = CYLINDRICAL_SURFACE('',#32347,0.25) ;
#27070 = CYLINDRICAL_SURFACE('',#32349,0.25) ;
#27071 = CYLINDRICAL_SURFACE('',#32351,0.25) ;
#27072 = CYLINDRICAL_SURFACE('',#32354,0.25) ;
#27073 = CYLINDRICAL_SURFACE('',#32357,0.25) ;
#27074 = CYLINDRICAL_SURFACE('',#32360,0.3) ;
#27075 = ADVANCED_FACE('',(#2340),#26651,.F.) ;
#27076 = ADVANCED_FACE('',(#2341,#1112),#1408,.F.) ;
#27077 = ADVANCED_FACE('',(#2342),#1409,.F.) ;
#27078 = ADVANCED_FACE('',(#2343),#1410,.T.) ;
#27079 = ADVANCED_FACE('',(#2344),#1411,.F.) ;
#27080 = ADVANCED_FACE('',(#2345),#1412,.T.) ;
#27081 = ADVANCED_FACE('',(#2346),#1413,.F.) ;
#27082 = ADVANCED_FACE('',(#2347,#1113),#1414,.F.) ;
#27083 = ADVANCED_FACE('',(#2348),#1415,.F.) ;
#27084 = ADVANCED_FACE('',(#2349),#26652,.T.) ;
#27085 = ADVANCED_FACE('',(#2350),#26653,.F.) ;
#27086 = ADVANCED_FACE('',(#2351,#1114),#1416,.F.) ;
#27087 = ADVANCED_FACE('',(#2352),#1417,.F.) ;
#27088 = ADVANCED_FACE('',(#2353),#1418,.T.) ;
#27089 = ADVANCED_FACE('',(#2354),#1419,.F.) ;
#27090 = ADVANCED_FACE('',(#2355),#1420,.T.) ;
#27091 = ADVANCED_FACE('',(#2356),#1421,.F.) ;
#27092 = ADVANCED_FACE('',(#2357,#1115),#1422,.F.) ;
#27093 = ADVANCED_FACE('',(#2358),#1423,.F.) ;
#27094 = ADVANCED_FACE('',(#2359),#1424,.T.) ;
#27095 = ADVANCED_FACE('',(#2360),#1425,.F.) ;
#27096 = ADVANCED_FACE('',(#2361),#1426,.F.) ;
#27097 = ADVANCED_FACE('',(#2362),#1427,.F.) ;
#27098 = ADVANCED_FACE('',(#2363),#1428,.F.) ;
#27099 = ADVANCED_FACE('',(#2364),#1429,.F.) ;
#27100 = ADVANCED_FACE('',(#2365),#1430,.T.) ;
#27101 = ADVANCED_FACE('',(#2366),#1431,.F.) ;
#27102 = ADVANCED_FACE('',(#2367),#1432,.F.) ;
#27103 = ADVANCED_FACE('',(#2368),#1433,.F.) ;
#27104 = ADVANCED_FACE('',(#2369),#1434,.T.) ;
#27105 = ADVANCED_FACE('',(#2370),#1435,.F.) ;
#27106 = ADVANCED_FACE('',(#2371),#1436,.F.) ;
#27107 = ADVANCED_FACE('',(#2372),#1437,.F.) ;
#27108 = ADVANCED_FACE('',(#2373),#1438,.F.) ;
#27109 = ADVANCED_FACE('',(#2374),#1439,.F.) ;
#27110 = ADVANCED_FACE('',(#2375),#1440,.T.) ;
#27111 = ADVANCED_FACE('',(#2376),#1441,.F.) ;
#27112 = ADVANCED_FACE('',(#2377),#1442,.F.) ;
#27113 = ADVANCED_FACE('',(#2378),#1443,.F.) ;
#27114 = ADVANCED_FACE('',(#2379),#1444,.T.) ;
#27115 = ADVANCED_FACE('',(#2380),#1445,.F.) ;
#27116 = ADVANCED_FACE('',(#2381),#1446,.F.) ;
#27117 = ADVANCED_FACE('',(#2382),#1447,.F.) ;
#27118 = ADVANCED_FACE('',(#2383),#1448,.F.) ;
#27119 = ADVANCED_FACE('',(#2384),#1449,.F.) ;
#27120 = ADVANCED_FACE('',(#2385),#1450,.T.) ;
#27121 = ADVANCED_FACE('',(#2386),#1451,.F.) ;
#27122 = ADVANCED_FACE('',(#2387),#1452,.F.) ;
#27123 = ADVANCED_FACE('',(#2388),#1453,.F.) ;
#27124 = ADVANCED_FACE('',(#2389),#1454,.T.) ;
#27125 = ADVANCED_FACE('',(#2390),#1455,.F.) ;
#27126 = ADVANCED_FACE('',(#2391),#1456,.F.) ;
#27127 = ADVANCED_FACE('',(#2392),#1457,.F.) ;
#27128 = ADVANCED_FACE('',(#2393),#1458,.F.) ;
#27129 = ADVANCED_FACE('',(#2394),#1459,.F.) ;
#27130 = ADVANCED_FACE('',(#2395),#1460,.T.) ;
#27131 = ADVANCED_FACE('',(#2396),#1461,.F.) ;
#27132 = ADVANCED_FACE('',(#2397),#1462,.F.) ;
#27133 = ADVANCED_FACE('',(#2398),#1463,.F.) ;
#27134 = ADVANCED_FACE('',(#2399),#26654,.F.) ;
#27135 = ADVANCED_FACE('',(#2400),#26655,.F.) ;
#27136 = ADVANCED_FACE('',(#2401,#1116),#1464,.T.) ;
#27137 = ADVANCED_FACE('',(#2402,#1117),#1465,.T.) ;
#27138 = ADVANCED_FACE('',(#2403,#1118,#1119,#1120,#1121),#1090,.F.) ;
#27139 = ADVANCED_FACE('',(#2404,#1122,#1123,#1124,#1125),#1091,.T.) ;
#27140 = ADVANCED_FACE('',(#2405,#1126),#1466,.T.) ;
#27141 = ADVANCED_FACE('',(#2406),#1467,.F.) ;
#27142 = ADVANCED_FACE('',(#2407),#1468,.T.) ;
#27143 = ADVANCED_FACE('',(#2408),#1469,.T.) ;
#27144 = ADVANCED_FACE('',(#2409),#1470,.F.) ;
#27145 = ADVANCED_FACE('',(#2410),#1471,.F.) ;
#27146 = ADVANCED_FACE('',(#2411),#1472,.T.) ;
#27147 = ADVANCED_FACE('',(#2412),#1473,.F.) ;
#27148 = ADVANCED_FACE('',(#2413),#1474,.F.) ;
#27149 = ADVANCED_FACE('',(#2414),#26656,.F.) ;
#27150 = ADVANCED_FACE('',(#2415,#1127),#1475,.T.) ;
#27151 = ADVANCED_FACE('',(#2416),#26657,.T.) ;
#27152 = ADVANCED_FACE('',(#2417),#1476,.T.) ;
#27153 = ADVANCED_FACE('',(#2418,#1128,#1129),#1477,.T.) ;
#27154 = ADVANCED_FACE('',(#2419),#1478,.T.) ;
#27155 = ADVANCED_FACE('',(#2420),#1479,.F.) ;
#27156 = ADVANCED_FACE('',(#2421),#1480,.F.) ;
#27157 = ADVANCED_FACE('',(#2422),#1481,.T.) ;
#27158 = ADVANCED_FACE('',(#2423),#26658,.T.) ;
#27159 = ADVANCED_FACE('',(#2424),#1482,.T.) ;
#27160 = ADVANCED_FACE('',(#2425),#1483,.F.) ;
#27161 = ADVANCED_FACE('',(#2426),#1484,.F.) ;
#27162 = ADVANCED_FACE('',(#2427),#1485,.F.) ;
#27163 = ADVANCED_FACE('',(#2428),#1486,.F.) ;
#27164 = ADVANCED_FACE('',(#2429),#1487,.F.) ;
#27165 = ADVANCED_FACE('',(#2430),#1488,.F.) ;
#27166 = ADVANCED_FACE('',(#2431),#1489,.F.) ;
#27167 = ADVANCED_FACE('',(#2432),#1490,.F.) ;
#27168 = ADVANCED_FACE('',(#2433),#1491,.F.) ;
#27169 = ADVANCED_FACE('',(#2434),#1492,.F.) ;
#27170 = ADVANCED_FACE('',(#2435),#1493,.F.) ;
#27171 = ADVANCED_FACE('',(#2436),#1494,.F.) ;
#27172 = ADVANCED_FACE('',(#2437),#1495,.F.) ;
#27173 = ADVANCED_FACE('',(#2438),#1496,.F.) ;
#27174 = ADVANCED_FACE('',(#2439),#26659,.T.) ;
#27175 = ADVANCED_FACE('',(#2440),#26660,.T.) ;
#27176 = ADVANCED_FACE('',(#2441),#26661,.F.) ;
#27177 = ADVANCED_FACE('',(#2442),#1497,.F.) ;
#27178 = ADVANCED_FACE('',(#2443),#1498,.F.) ;
#27179 = ADVANCED_FACE('',(#2444),#1499,.F.) ;
#27180 = ADVANCED_FACE('',(#2445),#1500,.F.) ;
#27181 = ADVANCED_FACE('',(#2446),#1501,.F.) ;
#27182 = ADVANCED_FACE('',(#2447),#1502,.F.) ;
#27183 = ADVANCED_FACE('',(#2448),#1503,.F.) ;
#27184 = ADVANCED_FACE('',(#2449),#1504,.F.) ;
#27185 = ADVANCED_FACE('',(#2450,#1130,#1131,#1132,#1133,#1134,#1135,#1136,
#1137,#1138,#1139,#1140,#1141,#1142,#1143,#1144,#1145,#1146,#1147,#1148,
#1149,#1150,#1151,#1152,#1153,#1154,#1155,#1156,#1157,#1158,#1159,#1160,
#1161,#1162,#1163,#1164,#1165,#1166,#1167,#1168,#1169,#1170,#1171,#1172,
#1173,#1174,#1175,#1176,#1177,#1178,#1179,#1180,#1181),#1505,.T.) ;
#27186 = ADVANCED_FACE('',(#2451),#26662,.F.) ;
#27187 = ADVANCED_FACE('',(#2452,#1182,#1183,#1184,#1185,#1186,#1187,#1188,
#1189,#1190,#1191,#1192,#1193,#1194,#1195,#1196,#1197,#1198,#1199,#1200,
#1201,#1202,#1203,#1204,#1205,#1206,#1207,#1208,#1209,#1210,#1211,#1212,
#1213,#1214,#1215,#1216,#1217,#1218,#1219,#1220,#1221,#1222,#1223,#1224,
#1225,#1226,#1227,#1228,#1229,#1230,#1231,#1232,#1233),#1506,.T.) ;
#27188 = ADVANCED_FACE('',(#2453),#26663,.T.) ;
#27189 = ADVANCED_FACE('',(#2454),#26664,.T.) ;
#27190 = ADVANCED_FACE('',(#2455),#1507,.F.) ;
#27191 = ADVANCED_FACE('',(#2456),#1508,.F.) ;
#27192 = ADVANCED_FACE('',(#2457),#1509,.F.) ;
#27193 = ADVANCED_FACE('',(#2458),#1510,.F.) ;
#27194 = ADVANCED_FACE('',(#2459),#1511,.F.) ;
#27195 = ADVANCED_FACE('',(#2460),#1512,.F.) ;
#27196 = ADVANCED_FACE('',(#2461),#1513,.F.) ;
#27197 = ADVANCED_FACE('',(#2462),#1514,.F.) ;
#27198 = ADVANCED_FACE('',(#2463),#1515,.F.) ;
#27199 = ADVANCED_FACE('',(#2464),#1516,.F.) ;
#27200 = ADVANCED_FACE('',(#2465),#1517,.F.) ;
#27201 = ADVANCED_FACE('',(#2466),#1518,.F.) ;
#27202 = ADVANCED_FACE('',(#2467),#1519,.F.) ;
#27203 = ADVANCED_FACE('',(#2468),#1520,.F.) ;
#27204 = ADVANCED_FACE('',(#2469),#1521,.F.) ;
#27205 = ADVANCED_FACE('',(#2470),#1522,.F.) ;
#27206 = ADVANCED_FACE('',(#2471),#1523,.F.) ;
#27207 = ADVANCED_FACE('',(#2472),#26665,.F.) ;
#27208 = ADVANCED_FACE('',(#2473),#26666,.T.) ;
#27209 = ADVANCED_FACE('',(#2474),#1524,.F.) ;
#27210 = ADVANCED_FACE('',(#2475),#1525,.F.) ;
#27211 = ADVANCED_FACE('',(#2476),#1526,.F.) ;
#27212 = ADVANCED_FACE('',(#2477),#1527,.F.) ;
#27213 = ADVANCED_FACE('',(#2478),#1528,.F.) ;
#27214 = ADVANCED_FACE('',(#2479),#26667,.F.) ;
#27215 = ADVANCED_FACE('',(#2480),#26668,.T.) ;
#27216 = ADVANCED_FACE('',(#2481),#26669,.T.) ;
#27217 = ADVANCED_FACE('',(#2482),#1529,.F.) ;
#27218 = ADVANCED_FACE('',(#2483),#1530,.F.) ;
#27219 = ADVANCED_FACE('',(#2484),#1531,.F.) ;
#27220 = ADVANCED_FACE('',(#2485),#1532,.F.) ;
#27221 = ADVANCED_FACE('',(#2486),#1533,.F.) ;
#27222 = ADVANCED_FACE('',(#2487),#1534,.F.) ;
#27223 = ADVANCED_FACE('',(#2488),#1535,.F.) ;
#27224 = ADVANCED_FACE('',(#2489),#1536,.F.) ;
#27225 = ADVANCED_FACE('',(#2490),#1537,.F.) ;
#27226 = ADVANCED_FACE('',(#2491),#1538,.F.) ;
#27227 = ADVANCED_FACE('',(#2492),#1539,.F.) ;
#27228 = ADVANCED_FACE('',(#2493),#1540,.F.) ;
#27229 = ADVANCED_FACE('',(#2494),#1541,.F.) ;
#27230 = ADVANCED_FACE('',(#2495),#1542,.F.) ;
#27231 = ADVANCED_FACE('',(#2496),#1543,.F.) ;
#27232 = ADVANCED_FACE('',(#2497),#1544,.F.) ;
#27233 = ADVANCED_FACE('',(#2498),#1545,.F.) ;
#27234 = ADVANCED_FACE('',(#2499),#26670,.T.) ;
#27235 = ADVANCED_FACE('',(#2500),#1546,.F.) ;
#27236 = ADVANCED_FACE('',(#2501),#1547,.F.) ;
#27237 = ADVANCED_FACE('',(#2502),#1548,.F.) ;
#27238 = ADVANCED_FACE('',(#2503),#1549,.F.) ;
#27239 = ADVANCED_FACE('',(#2504),#1550,.F.) ;
#27240 = ADVANCED_FACE('',(#2505),#1551,.F.) ;
#27241 = ADVANCED_FACE('',(#2506),#1552,.F.) ;
#27242 = ADVANCED_FACE('',(#2507),#1553,.F.) ;
#27243 = ADVANCED_FACE('',(#2508),#26671,.T.) ;
#27244 = ADVANCED_FACE('',(#2509),#1554,.F.) ;
#27245 = ADVANCED_FACE('',(#2510),#1555,.F.) ;
#27246 = ADVANCED_FACE('',(#2511),#1556,.F.) ;
#27247 = ADVANCED_FACE('',(#2512),#1557,.F.) ;
#27248 = ADVANCED_FACE('',(#2513),#1558,.F.) ;
#27249 = ADVANCED_FACE('',(#2514),#1559,.F.) ;
#27250 = ADVANCED_FACE('',(#2515),#1560,.F.) ;
#27251 = ADVANCED_FACE('',(#2516),#1561,.F.) ;
#27252 = ADVANCED_FACE('',(#2517),#1562,.F.) ;
#27253 = ADVANCED_FACE('',(#2518),#1563,.F.) ;
#27254 = ADVANCED_FACE('',(#2519),#1564,.F.) ;
#27255 = ADVANCED_FACE('',(#2520),#1565,.F.) ;
#27256 = ADVANCED_FACE('',(#2521),#1566,.F.) ;
#27257 = ADVANCED_FACE('',(#2522),#1567,.F.) ;
#27258 = ADVANCED_FACE('',(#2523),#1568,.F.) ;
#27259 = ADVANCED_FACE('',(#2524),#1569,.F.) ;
#27260 = ADVANCED_FACE('',(#2525),#1570,.F.) ;
#27261 = ADVANCED_FACE('',(#2526),#1571,.F.) ;
#27262 = ADVANCED_FACE('',(#2527),#1572,.F.) ;
#27263 = ADVANCED_FACE('',(#2528),#26672,.F.) ;
#27264 = ADVANCED_FACE('',(#2529),#26673,.T.) ;
#27265 = ADVANCED_FACE('',(#2530),#1573,.F.) ;
#27266 = ADVANCED_FACE('',(#2531),#26674,.T.) ;
#27267 = ADVANCED_FACE('',(#2532),#26675,.T.) ;
#27268 = ADVANCED_FACE('',(#2533),#1574,.F.) ;
#27269 = ADVANCED_FACE('',(#2534),#1575,.F.) ;
#27270 = ADVANCED_FACE('',(#2535),#1576,.F.) ;
#27271 = ADVANCED_FACE('',(#2536),#1577,.F.) ;
#27272 = ADVANCED_FACE('',(#2537),#1578,.F.) ;
#27273 = ADVANCED_FACE('',(#2538),#1579,.F.) ;
#27274 = ADVANCED_FACE('',(#2539),#1580,.F.) ;
#27275 = ADVANCED_FACE('',(#2540),#1581,.F.) ;
#27276 = ADVANCED_FACE('',(#2541),#1582,.F.) ;
#27277 = ADVANCED_FACE('',(#2542),#1583,.F.) ;
#27278 = ADVANCED_FACE('',(#2543),#1584,.F.) ;
#27279 = ADVANCED_FACE('',(#2544),#1585,.F.) ;
#27280 = ADVANCED_FACE('',(#2545),#1586,.F.) ;
#27281 = ADVANCED_FACE('',(#2546),#1587,.F.) ;
#27282 = ADVANCED_FACE('',(#2547),#1588,.F.) ;
#27283 = ADVANCED_FACE('',(#2548),#1589,.F.) ;
#27284 = ADVANCED_FACE('',(#2549),#1590,.F.) ;
#27285 = ADVANCED_FACE('',(#2550),#1591,.F.) ;
#27286 = ADVANCED_FACE('',(#2551),#1592,.F.) ;
#27287 = ADVANCED_FACE('',(#2552),#1593,.F.) ;
#27288 = ADVANCED_FACE('',(#2553),#1594,.F.) ;
#27289 = ADVANCED_FACE('',(#2554),#1595,.F.) ;
#27290 = ADVANCED_FACE('',(#2555),#26676,.T.) ;
#27291 = ADVANCED_FACE('',(#2556),#26677,.T.) ;
#27292 = ADVANCED_FACE('',(#2557),#26678,.F.) ;
#27293 = ADVANCED_FACE('',(#2558),#26679,.F.) ;
#27294 = ADVANCED_FACE('',(#2559),#1596,.F.) ;
#27295 = ADVANCED_FACE('',(#2560),#1597,.F.) ;
#27296 = ADVANCED_FACE('',(#2561),#1598,.F.) ;
#27297 = ADVANCED_FACE('',(#2562),#1599,.F.) ;
#27298 = ADVANCED_FACE('',(#2563),#1600,.F.) ;
#27299 = ADVANCED_FACE('',(#2564),#1601,.F.) ;
#27300 = ADVANCED_FACE('',(#2565),#1602,.F.) ;
#27301 = ADVANCED_FACE('',(#2566),#1603,.F.) ;
#27302 = ADVANCED_FACE('',(#2567),#1604,.F.) ;
#27303 = ADVANCED_FACE('',(#2568),#1605,.F.) ;
#27304 = ADVANCED_FACE('',(#2569),#1606,.F.) ;
#27305 = ADVANCED_FACE('',(#2570),#1607,.F.) ;
#27306 = ADVANCED_FACE('',(#2571),#1608,.F.) ;
#27307 = ADVANCED_FACE('',(#2572),#1609,.F.) ;
#27308 = ADVANCED_FACE('',(#2573),#1610,.F.) ;
#27309 = ADVANCED_FACE('',(#2574),#1611,.F.) ;
#27310 = ADVANCED_FACE('',(#2575),#1612,.F.) ;
#27311 = ADVANCED_FACE('',(#2576),#1613,.F.) ;
#27312 = ADVANCED_FACE('',(#2577),#1614,.F.) ;
#27313 = ADVANCED_FACE('',(#2578),#1615,.F.) ;
#27314 = ADVANCED_FACE('',(#2579),#1616,.F.) ;
#27315 = ADVANCED_FACE('',(#2580),#1617,.F.) ;
#27316 = ADVANCED_FACE('',(#2581),#1618,.F.) ;
#27317 = ADVANCED_FACE('',(#2582),#1619,.F.) ;
#27318 = ADVANCED_FACE('',(#2583),#26680,.F.) ;
#27319 = ADVANCED_FACE('',(#2584),#26681,.F.) ;
#27320 = ADVANCED_FACE('',(#2585),#26682,.T.) ;
#27321 = ADVANCED_FACE('',(#2586),#1620,.F.) ;
#27322 = ADVANCED_FACE('',(#2587),#1621,.F.) ;
#27323 = ADVANCED_FACE('',(#2588),#1622,.F.) ;
#27324 = ADVANCED_FACE('',(#2589),#1623,.F.) ;
#27325 = ADVANCED_FACE('',(#2590),#1624,.F.) ;
#27326 = ADVANCED_FACE('',(#2591),#1625,.F.) ;
#27327 = ADVANCED_FACE('',(#2592),#26683,.F.) ;
#27328 = ADVANCED_FACE('',(#2593),#26684,.T.) ;
#27329 = ADVANCED_FACE('',(#2594),#1626,.F.) ;
#27330 = ADVANCED_FACE('',(#2595),#1627,.F.) ;
#27331 = ADVANCED_FACE('',(#2596),#1628,.F.) ;
#27332 = ADVANCED_FACE('',(#2597),#1629,.F.) ;
#27333 = ADVANCED_FACE('',(#2598),#1630,.F.) ;
#27334 = ADVANCED_FACE('',(#2599),#1631,.F.) ;
#27335 = ADVANCED_FACE('',(#2600),#1632,.F.) ;
#27336 = ADVANCED_FACE('',(#2601),#1633,.F.) ;
#27337 = ADVANCED_FACE('',(#2602),#1634,.F.) ;
#27338 = ADVANCED_FACE('',(#2603),#1635,.F.) ;
#27339 = ADVANCED_FACE('',(#2604),#1636,.F.) ;
#27340 = ADVANCED_FACE('',(#2605),#1637,.F.) ;
#27341 = ADVANCED_FACE('',(#2606),#1638,.F.) ;
#27342 = ADVANCED_FACE('',(#2607),#1639,.F.) ;
#27343 = ADVANCED_FACE('',(#2608),#1640,.F.) ;
#27344 = ADVANCED_FACE('',(#2609),#1641,.F.) ;
#27345 = ADVANCED_FACE('',(#2610),#1642,.F.) ;
#27346 = ADVANCED_FACE('',(#2611),#1643,.F.) ;
#27347 = ADVANCED_FACE('',(#2612),#26685,.F.) ;
#27348 = ADVANCED_FACE('',(#2613),#26686,.T.) ;
#27349 = ADVANCED_FACE('',(#2614),#1644,.F.) ;
#27350 = ADVANCED_FACE('',(#2615),#1645,.F.) ;
#27351 = ADVANCED_FACE('',(#2616),#26687,.T.) ;
#27352 = ADVANCED_FACE('',(#2617),#26688,.T.) ;
#27353 = ADVANCED_FACE('',(#2618),#26689,.F.) ;
#27354 = ADVANCED_FACE('',(#2619),#1646,.F.) ;
#27355 = ADVANCED_FACE('',(#2620),#1647,.F.) ;
#27356 = ADVANCED_FACE('',(#2621),#1648,.F.) ;
#27357 = ADVANCED_FACE('',(#2622),#1649,.F.) ;
#27358 = ADVANCED_FACE('',(#2623),#1650,.F.) ;
#27359 = ADVANCED_FACE('',(#2624),#1651,.F.) ;
#27360 = ADVANCED_FACE('',(#2625),#1652,.F.) ;
#27361 = ADVANCED_FACE('',(#2626),#1653,.F.) ;
#27362 = ADVANCED_FACE('',(#2627),#1654,.F.) ;
#27363 = ADVANCED_FACE('',(#2628),#1655,.F.) ;
#27364 = ADVANCED_FACE('',(#2629),#1656,.F.) ;
#27365 = ADVANCED_FACE('',(#2630),#1657,.F.) ;
#27366 = ADVANCED_FACE('',(#2631),#1658,.F.) ;
#27367 = ADVANCED_FACE('',(#2632),#1659,.F.) ;
#27368 = ADVANCED_FACE('',(#2633),#1660,.F.) ;
#27369 = ADVANCED_FACE('',(#2634),#1661,.F.) ;
#27370 = ADVANCED_FACE('',(#2635),#1662,.F.) ;
#27371 = ADVANCED_FACE('',(#2636),#1663,.F.) ;
#27372 = ADVANCED_FACE('',(#2637),#1664,.F.) ;
#27373 = ADVANCED_FACE('',(#2638),#1665,.F.) ;
#27374 = ADVANCED_FACE('',(#2639),#1666,.F.) ;
#27375 = ADVANCED_FACE('',(#2640),#1667,.F.) ;
#27376 = ADVANCED_FACE('',(#2641),#26690,.F.) ;
#27377 = ADVANCED_FACE('',(#2642),#1668,.F.) ;
#27378 = ADVANCED_FACE('',(#2643),#1669,.F.) ;
#27379 = ADVANCED_FACE('',(#2644),#26691,.F.) ;
#27380 = ADVANCED_FACE('',(#2645),#26692,.F.) ;
#27381 = ADVANCED_FACE('',(#2646),#26693,.T.) ;
#27382 = ADVANCED_FACE('',(#2647),#1670,.F.) ;
#27383 = ADVANCED_FACE('',(#2648),#1671,.F.) ;
#27384 = ADVANCED_FACE('',(#2649),#1672,.F.) ;
#27385 = ADVANCED_FACE('',(#2650),#1673,.F.) ;
#27386 = ADVANCED_FACE('',(#2651),#1674,.F.) ;
#27387 = ADVANCED_FACE('',(#2652),#1675,.F.) ;
#27388 = ADVANCED_FACE('',(#2653),#1676,.F.) ;
#27389 = ADVANCED_FACE('',(#2654),#1677,.F.) ;
#27390 = ADVANCED_FACE('',(#2655),#1678,.F.) ;
#27391 = ADVANCED_FACE('',(#2656),#1679,.F.) ;
#27392 = ADVANCED_FACE('',(#2657),#1680,.F.) ;
#27393 = ADVANCED_FACE('',(#2658),#1681,.F.) ;
#27394 = ADVANCED_FACE('',(#2659),#1682,.F.) ;
#27395 = ADVANCED_FACE('',(#2660),#1683,.F.) ;
#27396 = ADVANCED_FACE('',(#2661),#1684,.F.) ;
#27397 = ADVANCED_FACE('',(#2662),#1685,.F.) ;
#27398 = ADVANCED_FACE('',(#2663),#26694,.T.) ;
#27399 = ADVANCED_FACE('',(#2664),#1686,.F.) ;
#27400 = ADVANCED_FACE('',(#2665),#1687,.F.) ;
#27401 = ADVANCED_FACE('',(#2666),#26695,.T.) ;
#27402 = ADVANCED_FACE('',(#2667),#26696,.F.) ;
#27403 = ADVANCED_FACE('',(#2668),#1688,.F.) ;
#27404 = ADVANCED_FACE('',(#2669),#1689,.F.) ;
#27405 = ADVANCED_FACE('',(#2670),#1690,.F.) ;
#27406 = ADVANCED_FACE('',(#2671),#1691,.F.) ;
#27407 = ADVANCED_FACE('',(#2672),#1692,.F.) ;
#27408 = ADVANCED_FACE('',(#2673),#1693,.F.) ;
#27409 = ADVANCED_FACE('',(#2674),#1694,.F.) ;
#27410 = ADVANCED_FACE('',(#2675),#1695,.F.) ;
#27411 = ADVANCED_FACE('',(#2676),#1696,.F.) ;
#27412 = ADVANCED_FACE('',(#2677),#1697,.F.) ;
#27413 = ADVANCED_FACE('',(#2678),#1698,.F.) ;
#27414 = ADVANCED_FACE('',(#2679),#26697,.F.) ;
#27415 = ADVANCED_FACE('',(#2680),#26698,.T.) ;
#27416 = ADVANCED_FACE('',(#2681),#26699,.T.) ;
#27417 = ADVANCED_FACE('',(#2682),#1699,.F.) ;
#27418 = ADVANCED_FACE('',(#2683),#1700,.F.) ;
#27419 = ADVANCED_FACE('',(#2684),#26700,.T.) ;
#27420 = ADVANCED_FACE('',(#2685),#26701,.F.) ;
#27421 = ADVANCED_FACE('',(#2686),#1701,.F.) ;
#27422 = ADVANCED_FACE('',(#2687),#1702,.F.) ;
#27423 = ADVANCED_FACE('',(#2688),#1703,.F.) ;
#27424 = ADVANCED_FACE('',(#2689),#1704,.F.) ;
#27425 = ADVANCED_FACE('',(#2690),#1705,.F.) ;
#27426 = ADVANCED_FACE('',(#2691),#1706,.F.) ;
#27427 = ADVANCED_FACE('',(#2692),#1707,.F.) ;
#27428 = ADVANCED_FACE('',(#2693),#1708,.F.) ;
#27429 = ADVANCED_FACE('',(#2694),#1709,.F.) ;
#27430 = ADVANCED_FACE('',(#2695),#26702,.F.) ;
#27431 = ADVANCED_FACE('',(#2696),#1710,.F.) ;
#27432 = ADVANCED_FACE('',(#2697),#26703,.T.) ;
#27433 = ADVANCED_FACE('',(#2698),#1711,.F.) ;
#27434 = ADVANCED_FACE('',(#2699),#1712,.F.) ;
#27435 = ADVANCED_FACE('',(#2700),#1713,.F.) ;
#27436 = ADVANCED_FACE('',(#2701),#1714,.F.) ;
#27437 = ADVANCED_FACE('',(#2702),#1715,.F.) ;
#27438 = ADVANCED_FACE('',(#2703),#1716,.F.) ;
#27439 = ADVANCED_FACE('',(#2704),#1717,.F.) ;
#27440 = ADVANCED_FACE('',(#2705),#26704,.T.) ;
#27441 = ADVANCED_FACE('',(#2706),#1718,.F.) ;
#27442 = ADVANCED_FACE('',(#2707),#1719,.F.) ;
#27443 = ADVANCED_FACE('',(#2708),#1720,.F.) ;
#27444 = ADVANCED_FACE('',(#2709),#1721,.F.) ;
#27445 = ADVANCED_FACE('',(#2710),#1722,.F.) ;
#27446 = ADVANCED_FACE('',(#2711),#26705,.T.) ;
#27447 = ADVANCED_FACE('',(#2712),#26706,.F.) ;
#27448 = ADVANCED_FACE('',(#2713),#1723,.F.) ;
#27449 = ADVANCED_FACE('',(#2714),#1724,.F.) ;
#27450 = ADVANCED_FACE('',(#2715),#1725,.F.) ;
#27451 = ADVANCED_FACE('',(#2716),#1726,.F.) ;
#27452 = ADVANCED_FACE('',(#2717),#1727,.F.) ;
#27453 = ADVANCED_FACE('',(#2718),#1728,.F.) ;
#27454 = ADVANCED_FACE('',(#2719),#699,.T.) ;
#27455 = ADVANCED_FACE('',(#2720),#700,.T.) ;
#27456 = ADVANCED_FACE('',(#2721),#701,.T.) ;
#27457 = ADVANCED_FACE('',(#2722),#702,.T.) ;
#27458 = ADVANCED_FACE('',(#2723),#703,.T.) ;
#27459 = ADVANCED_FACE('',(#2724),#704,.T.) ;
#27460 = ADVANCED_FACE('',(#2725),#705,.T.) ;
#27461 = ADVANCED_FACE('',(#2726),#706,.T.) ;
#27462 = ADVANCED_FACE('',(#2727),#707,.T.) ;
#27463 = ADVANCED_FACE('',(#2728),#708,.T.) ;
#27464 = ADVANCED_FACE('',(#2729),#709,.T.) ;
#27465 = ADVANCED_FACE('',(#2730),#710,.T.) ;
#27466 = ADVANCED_FACE('',(#2731),#711,.T.) ;
#27467 = ADVANCED_FACE('',(#2732),#712,.T.) ;
#27468 = ADVANCED_FACE('',(#2733),#713,.T.) ;
#27469 = ADVANCED_FACE('',(#2734),#714,.T.) ;
#27470 = ADVANCED_FACE('',(#2735),#715,.T.) ;
#27471 = ADVANCED_FACE('',(#2736),#716,.T.) ;
#27472 = ADVANCED_FACE('',(#2737),#717,.T.) ;
#27473 = ADVANCED_FACE('',(#2738),#718,.T.) ;
#27474 = ADVANCED_FACE('',(#2739),#719,.T.) ;
#27475 = ADVANCED_FACE('',(#2740),#720,.T.) ;
#27476 = ADVANCED_FACE('',(#2741),#721,.T.) ;
#27477 = ADVANCED_FACE('',(#2742),#722,.T.) ;
#27478 = ADVANCED_FACE('',(#2743),#723,.T.) ;
#27479 = ADVANCED_FACE('',(#2744),#724,.T.) ;
#27480 = ADVANCED_FACE('',(#2745),#725,.T.) ;
#27481 = ADVANCED_FACE('',(#2746),#726,.T.) ;
#27482 = ADVANCED_FACE('',(#2747),#26707,.T.) ;
#27483 = ADVANCED_FACE('',(#2748),#26708,.T.) ;
#27484 = ADVANCED_FACE('',(#2749),#26709,.T.) ;
#27485 = ADVANCED_FACE('',(#2750),#26710,.T.) ;
#27486 = ADVANCED_FACE('',(#2751),#26711,.T.) ;
#27487 = ADVANCED_FACE('',(#2752),#26712,.T.) ;
#27488 = ADVANCED_FACE('',(#2753),#26713,.T.) ;
#27489 = ADVANCED_FACE('',(#2754),#26714,.T.) ;
#27490 = ADVANCED_FACE('',(#2755),#26715,.T.) ;
#27491 = ADVANCED_FACE('',(#2756),#26716,.T.) ;
#27492 = ADVANCED_FACE('',(#2757),#26717,.T.) ;
#27493 = ADVANCED_FACE('',(#2758),#26718,.T.) ;
#27494 = ADVANCED_FACE('',(#2759),#26719,.T.) ;
#27495 = ADVANCED_FACE('',(#2760),#26720,.T.) ;
#27496 = ADVANCED_FACE('',(#2761),#26721,.T.) ;
#27497 = ADVANCED_FACE('',(#2762),#26722,.T.) ;
#27498 = ADVANCED_FACE('',(#2763),#26723,.T.) ;
#27499 = ADVANCED_FACE('',(#2764),#26724,.T.) ;
#27500 = ADVANCED_FACE('',(#2765),#26725,.T.) ;
#27501 = ADVANCED_FACE('',(#2766),#26726,.T.) ;
#27502 = ADVANCED_FACE('',(#2767),#26727,.T.) ;
#27503 = ADVANCED_FACE('',(#2768),#26728,.T.) ;
#27504 = ADVANCED_FACE('',(#2769),#26729,.T.) ;
#27505 = ADVANCED_FACE('',(#2770),#26730,.T.) ;
#27506 = ADVANCED_FACE('',(#2771),#26731,.T.) ;
#27507 = ADVANCED_FACE('',(#2772),#26732,.T.) ;
#27508 = ADVANCED_FACE('',(#2773),#26733,.T.) ;
#27509 = ADVANCED_FACE('',(#2774),#26734,.T.) ;
#27510 = ADVANCED_FACE('',(#2775),#26735,.F.) ;
#27511 = ADVANCED_FACE('',(#2776),#26736,.F.) ;
#27512 = ADVANCED_FACE('',(#2777),#26737,.F.) ;
#27513 = ADVANCED_FACE('',(#2778),#26738,.F.) ;
#27514 = ADVANCED_FACE('',(#2779),#26739,.F.) ;
#27515 = ADVANCED_FACE('',(#2780),#26740,.F.) ;
#27516 = ADVANCED_FACE('',(#2781),#26741,.T.) ;
#27517 = ADVANCED_FACE('',(#2782),#1729,.T.) ;
#27518 = ADVANCED_FACE('',(#2783),#1730,.T.) ;
#27519 = ADVANCED_FACE('',(#2784),#1731,.T.) ;
#27520 = ADVANCED_FACE('',(#2785,#1234,#1235),#1732,.T.) ;
#27521 = ADVANCED_FACE('',(#2786,#1236,#1237),#1733,.F.) ;
#27522 = ADVANCED_FACE('',(#2787),#1734,.T.) ;
#27523 = ADVANCED_FACE('',(#2788),#1735,.T.) ;
#27524 = ADVANCED_FACE('',(#2789),#26742,.F.) ;
#27525 = ADVANCED_FACE('',(#2790),#26743,.F.) ;
#27526 = ADVANCED_FACE('',(#2791),#26744,.T.) ;
#27527 = ADVANCED_FACE('',(#2792),#1736,.T.) ;
#27528 = ADVANCED_FACE('',(#2793),#1737,.T.) ;
#27529 = ADVANCED_FACE('',(#2794),#1738,.T.) ;
#27530 = ADVANCED_FACE('',(#2795,#1238,#1239),#1739,.T.) ;
#27531 = ADVANCED_FACE('',(#2796,#1240,#1241),#1740,.F.) ;
#27532 = ADVANCED_FACE('',(#2797),#1741,.T.) ;
#27533 = ADVANCED_FACE('',(#2798),#1742,.T.) ;
#27534 = ADVANCED_FACE('',(#2799),#26745,.F.) ;
#27535 = ADVANCED_FACE('',(#2800),#26746,.F.) ;
#27536 = ADVANCED_FACE('',(#2801),#26747,.F.) ;
#27537 = ADVANCED_FACE('',(#2802),#26748,.T.) ;
#27538 = ADVANCED_FACE('',(#2803,#1242),#1743,.T.) ;
#27539 = ADVANCED_FACE('',(#2804,#1243,#1244,#1245,#1246),#1744,.T.) ;
#27540 = ADVANCED_FACE('',(#2805),#26749,.F.) ;
#27541 = ADVANCED_FACE('',(#2806),#26750,.T.) ;
#27542 = ADVANCED_FACE('',(#2807,#1247),#1745,.T.) ;
#27543 = ADVANCED_FACE('',(#2808),#1746,.T.) ;
#27544 = ADVANCED_FACE('',(#2809),#1747,.T.) ;
#27545 = ADVANCED_FACE('',(#2810),#1748,.T.) ;
#27546 = ADVANCED_FACE('',(#2811),#1749,.T.) ;
#27547 = ADVANCED_FACE('',(#2812),#1750,.T.) ;
#27548 = ADVANCED_FACE('',(#2813,#1248),#1751,.F.) ;
#27549 = ADVANCED_FACE('',(#2814),#1752,.F.) ;
#27550 = ADVANCED_FACE('',(#2815),#1753,.F.) ;
#27551 = ADVANCED_FACE('',(#2816,#1249,#1250),#1754,.F.) ;
#27552 = ADVANCED_FACE('',(#2817),#1755,.F.) ;
#27553 = ADVANCED_FACE('',(#2818),#1756,.F.) ;
#27554 = ADVANCED_FACE('',(#2819),#1757,.T.) ;
#27555 = ADVANCED_FACE('',(#2820),#1758,.F.) ;
#27556 = ADVANCED_FACE('',(#2821),#1759,.F.) ;
#27557 = ADVANCED_FACE('',(#2822),#1760,.F.) ;
#27558 = ADVANCED_FACE('',(#2823),#1761,.F.) ;
#27559 = ADVANCED_FACE('',(#2824),#1762,.F.) ;
#27560 = ADVANCED_FACE('',(#2825),#1763,.F.) ;
#27561 = ADVANCED_FACE('',(#2826),#1764,.T.) ;
#27562 = ADVANCED_FACE('',(#2827),#1765,.F.) ;
#27563 = ADVANCED_FACE('',(#2828),#1766,.F.) ;
#27564 = ADVANCED_FACE('',(#2829),#1767,.F.) ;
#27565 = ADVANCED_FACE('',(#2830),#1768,.T.) ;
#27566 = ADVANCED_FACE('',(#2831),#1769,.F.) ;
#27567 = ADVANCED_FACE('',(#2832),#1770,.F.) ;
#27568 = ADVANCED_FACE('',(#2833,#1251),#1771,.F.) ;
#27569 = ADVANCED_FACE('',(#2834),#1772,.F.) ;
#27570 = ADVANCED_FACE('',(#2835),#1773,.F.) ;
#27571 = ADVANCED_FACE('',(#2836),#1774,.F.) ;
#27572 = ADVANCED_FACE('',(#2837),#1775,.T.) ;
#27573 = ADVANCED_FACE('',(#2838),#1776,.T.) ;
#27574 = ADVANCED_FACE('',(#2839),#1777,.T.) ;
#27575 = ADVANCED_FACE('',(#2840),#1778,.T.) ;
#27576 = ADVANCED_FACE('',(#2841,#1252),#1779,.F.) ;
#27577 = ADVANCED_FACE('',(#2842),#1780,.T.) ;
#27578 = ADVANCED_FACE('',(#2843),#1781,.F.) ;
#27579 = ADVANCED_FACE('',(#2844),#1782,.F.) ;
#27580 = ADVANCED_FACE('',(#2845,#1253),#1783,.F.) ;
#27581 = ADVANCED_FACE('',(#2846),#1784,.F.) ;
#27582 = ADVANCED_FACE('',(#2847),#1785,.F.) ;
#27583 = ADVANCED_FACE('',(#2848),#1786,.F.) ;
#27584 = ADVANCED_FACE('',(#2849),#1787,.T.) ;
#27585 = ADVANCED_FACE('',(#2850),#1788,.T.) ;
#27586 = ADVANCED_FACE('',(#2851),#1789,.T.) ;
#27587 = ADVANCED_FACE('',(#2852),#1790,.T.) ;
#27588 = ADVANCED_FACE('',(#2853,#1254),#1791,.T.) ;
#27589 = ADVANCED_FACE('',(#2854,#1255),#1792,.T.) ;
#27590 = ADVANCED_FACE('',(#2855),#26751,.T.) ;
#27591 = ADVANCED_FACE('',(#2856),#26752,.T.) ;
#27592 = ADVANCED_FACE('',(#2857),#26753,.F.) ;
#27593 = ADVANCED_FACE('',(#2858),#26754,.F.) ;
#27594 = ADVANCED_FACE('',(#2859),#1793,.T.) ;
#27595 = ADVANCED_FACE('',(#2860),#1794,.F.) ;
#27596 = ADVANCED_FACE('',(#2861),#1795,.F.) ;
#27597 = ADVANCED_FACE('',(#2862),#1796,.T.) ;
#27598 = ADVANCED_FACE('',(#2863),#1797,.F.) ;
#27599 = ADVANCED_FACE('',(#2864),#1798,.F.) ;
#27600 = ADVANCED_FACE('',(#2865,#1256),#1799,.F.) ;
#27601 = ADVANCED_FACE('',(#2866,#1257),#1800,.F.) ;
#27602 = ADVANCED_FACE('',(#2867),#1801,.F.) ;
#27603 = ADVANCED_FACE('',(#2868,#1258,#1259),#1802,.F.) ;
#27604 = ADVANCED_FACE('',(#2869),#1803,.F.) ;
#27605 = ADVANCED_FACE('',(#2870),#1804,.F.) ;
#27606 = ADVANCED_FACE('',(#2871,#1260),#1805,.F.) ;
#27607 = ADVANCED_FACE('',(#2872),#1806,.T.) ;
#27608 = ADVANCED_FACE('',(#2873),#1807,.T.) ;
#27609 = ADVANCED_FACE('',(#2874),#1808,.T.) ;
#27610 = ADVANCED_FACE('',(#2875),#1809,.T.) ;
#27611 = ADVANCED_FACE('',(#2876),#1810,.T.) ;
#27612 = ADVANCED_FACE('',(#2877,#1261),#1811,.T.) ;
#27613 = ADVANCED_FACE('',(#2878),#26755,.T.) ;
#27614 = ADVANCED_FACE('',(#2879),#26756,.F.) ;
#27615 = ADVANCED_FACE('',(#2880,#1262,#1263,#1264,#1265),#1812,.T.) ;
#27616 = ADVANCED_FACE('',(#2881,#1266),#1813,.T.) ;
#27617 = ADVANCED_FACE('',(#2882),#26757,.T.) ;
#27618 = ADVANCED_FACE('',(#2883),#26758,.F.) ;
#27619 = ADVANCED_FACE('',(#2884),#26759,.T.) ;
#27620 = ADVANCED_FACE('',(#2885),#1814,.F.) ;
#27621 = ADVANCED_FACE('',(#2886),#1815,.F.) ;
#27622 = ADVANCED_FACE('',(#2887),#1816,.F.) ;
#27623 = ADVANCED_FACE('',(#2888),#1817,.F.) ;
#27624 = ADVANCED_FACE('',(#2889),#1818,.F.) ;
#27625 = ADVANCED_FACE('',(#2890),#1819,.T.) ;
#27626 = ADVANCED_FACE('',(#2891),#1820,.F.) ;
#27627 = ADVANCED_FACE('',(#2892),#1821,.F.) ;
#27628 = ADVANCED_FACE('',(#2893),#1822,.F.) ;
#27629 = ADVANCED_FACE('',(#2894),#1823,.T.) ;
#27630 = ADVANCED_FACE('',(#2895,#1267),#1824,.F.) ;
#27631 = ADVANCED_FACE('',(#2896),#1825,.F.) ;
#27632 = ADVANCED_FACE('',(#2897),#1826,.F.) ;
#27633 = ADVANCED_FACE('',(#2898,#1268),#1827,.F.) ;
#27634 = ADVANCED_FACE('',(#2899),#1828,.F.) ;
#27635 = ADVANCED_FACE('',(#2900),#1829,.T.) ;
#27636 = ADVANCED_FACE('',(#2901,#1269),#1830,.F.) ;
#27637 = ADVANCED_FACE('',(#2902),#1831,.F.) ;
#27638 = ADVANCED_FACE('',(#2903),#26760,.T.) ;
#27639 = ADVANCED_FACE('',(#2904),#1832,.T.) ;
#27640 = ADVANCED_FACE('',(#2905),#1833,.T.) ;
#27641 = ADVANCED_FACE('',(#2906),#1834,.T.) ;
#27642 = ADVANCED_FACE('',(#2907),#1835,.T.) ;
#27643 = ADVANCED_FACE('',(#2908),#1836,.F.) ;
#27644 = ADVANCED_FACE('',(#2909),#1837,.F.) ;
#27645 = ADVANCED_FACE('',(#2910),#1838,.T.) ;
#27646 = ADVANCED_FACE('',(#2911),#1839,.T.) ;
#27647 = ADVANCED_FACE('',(#2912),#1840,.T.) ;
#27648 = ADVANCED_FACE('',(#2913),#1841,.T.) ;
#27649 = ADVANCED_FACE('',(#2914),#26761,.T.) ;
#27650 = ADVANCED_FACE('',(#2915),#1842,.T.) ;
#27651 = ADVANCED_FACE('',(#2916),#1843,.T.) ;
#27652 = ADVANCED_FACE('',(#2917),#1844,.T.) ;
#27653 = ADVANCED_FACE('',(#2918),#26762,.F.) ;
#27654 = ADVANCED_FACE('',(#2919),#1845,.T.) ;
#27655 = ADVANCED_FACE('',(#2920),#1846,.T.) ;
#27656 = ADVANCED_FACE('',(#2921),#1847,.F.) ;
#27657 = ADVANCED_FACE('',(#2922),#1848,.F.) ;
#27658 = ADVANCED_FACE('',(#2923),#26763,.T.) ;
#27659 = ADVANCED_FACE('',(#2924),#1849,.T.) ;
#27660 = ADVANCED_FACE('',(#2925),#1850,.T.) ;
#27661 = ADVANCED_FACE('',(#2926),#1851,.T.) ;
#27662 = ADVANCED_FACE('',(#2927),#26764,.T.) ;
#27663 = ADVANCED_FACE('',(#2928),#1852,.T.) ;
#27664 = ADVANCED_FACE('',(#2929),#1853,.T.) ;
#27665 = ADVANCED_FACE('',(#2930),#1854,.T.) ;
#27666 = ADVANCED_FACE('',(#2931),#1855,.F.) ;
#27667 = ADVANCED_FACE('',(#2932),#1856,.F.) ;
#27668 = ADVANCED_FACE('',(#2933),#26765,.T.) ;
#27669 = ADVANCED_FACE('',(#2934),#1857,.T.) ;
#27670 = ADVANCED_FACE('',(#2935),#1858,.T.) ;
#27671 = ADVANCED_FACE('',(#2936),#26766,.T.) ;
#27672 = ADVANCED_FACE('',(#2937),#1859,.T.) ;
#27673 = ADVANCED_FACE('',(#2938),#1860,.T.) ;
#27674 = ADVANCED_FACE('',(#2939),#1861,.T.) ;
#27675 = ADVANCED_FACE('',(#2940),#26767,.T.) ;
#27676 = ADVANCED_FACE('',(#2941),#1862,.T.) ;
#27677 = ADVANCED_FACE('',(#2942),#1863,.T.) ;
#27678 = ADVANCED_FACE('',(#2943),#1864,.T.) ;
#27679 = ADVANCED_FACE('',(#2944),#1865,.T.) ;
#27680 = ADVANCED_FACE('',(#2945),#1866,.T.) ;
#27681 = ADVANCED_FACE('',(#2946),#26768,.T.) ;
#27682 = ADVANCED_FACE('',(#2947),#1867,.T.) ;
#27683 = ADVANCED_FACE('',(#2948),#1868,.T.) ;
#27684 = ADVANCED_FACE('',(#2949),#1869,.F.) ;
#27685 = ADVANCED_FACE('',(#2950),#1870,.T.) ;
#27686 = ADVANCED_FACE('',(#2951),#1871,.T.) ;
#27687 = ADVANCED_FACE('',(#2952),#26769,.F.) ;
#27688 = ADVANCED_FACE('',(#2953),#26770,.F.) ;
#27689 = ADVANCED_FACE('',(#2954),#1872,.T.) ;
#27690 = ADVANCED_FACE('',(#2955),#1873,.T.) ;
#27691 = ADVANCED_FACE('',(#2956),#1874,.F.) ;
#27692 = ADVANCED_FACE('',(#2957),#1875,.T.) ;
#27693 = ADVANCED_FACE('',(#2958),#1876,.T.) ;
#27694 = ADVANCED_FACE('',(#2959),#1877,.T.) ;
#27695 = ADVANCED_FACE('',(#2960),#26771,.F.) ;
#27696 = ADVANCED_FACE('',(#2961),#26772,.F.) ;
#27697 = ADVANCED_FACE('',(#2962),#1878,.F.) ;
#27698 = ADVANCED_FACE('',(#2963),#1879,.F.) ;
#27699 = ADVANCED_FACE('',(#2964),#1880,.F.) ;
#27700 = ADVANCED_FACE('',(#2965),#1881,.T.) ;
#27701 = ADVANCED_FACE('',(#2966),#1882,.T.) ;
#27702 = ADVANCED_FACE('',(#2967),#26773,.F.) ;
#27703 = ADVANCED_FACE('',(#2968),#1883,.T.) ;
#27704 = ADVANCED_FACE('',(#2969),#1884,.T.) ;
#27705 = ADVANCED_FACE('',(#2970),#1885,.T.) ;
#27706 = ADVANCED_FACE('',(#2971),#1886,.T.) ;
#27707 = ADVANCED_FACE('',(#2972),#1887,.T.) ;
#27708 = ADVANCED_FACE('',(#2973),#1888,.T.) ;
#27709 = ADVANCED_FACE('',(#2974),#1889,.F.) ;
#27710 = ADVANCED_FACE('',(#2975),#1890,.F.) ;
#27711 = ADVANCED_FACE('',(#2976),#1891,.T.) ;
#27712 = ADVANCED_FACE('',(#2977),#1892,.T.) ;
#27713 = ADVANCED_FACE('',(#2978),#1893,.T.) ;
#27714 = ADVANCED_FACE('',(#2979),#1894,.T.) ;
#27715 = ADVANCED_FACE('',(#2980),#1895,.T.) ;
#27716 = ADVANCED_FACE('',(#2981),#1896,.F.) ;
#27717 = ADVANCED_FACE('',(#2982),#1897,.F.) ;
#27718 = ADVANCED_FACE('',(#2983),#1898,.F.) ;
#27719 = ADVANCED_FACE('',(#2984),#1899,.T.) ;
#27720 = ADVANCED_FACE('',(#2985),#1900,.F.) ;
#27721 = ADVANCED_FACE('',(#2986),#1901,.F.) ;
#27722 = ADVANCED_FACE('',(#2987),#1902,.T.) ;
#27723 = ADVANCED_FACE('',(#2988),#1903,.T.) ;
#27724 = ADVANCED_FACE('',(#2989),#1904,.F.) ;
#27725 = ADVANCED_FACE('',(#2990),#1905,.F.) ;
#27726 = ADVANCED_FACE('',(#2991),#1906,.F.) ;
#27727 = ADVANCED_FACE('',(#2992),#1907,.F.) ;
#27728 = ADVANCED_FACE('',(#2993),#1908,.F.) ;
#27729 = ADVANCED_FACE('',(#2994),#1909,.F.) ;
#27730 = ADVANCED_FACE('',(#2995),#26774,.F.) ;
#27731 = ADVANCED_FACE('',(#2996),#1910,.T.) ;
#27732 = ADVANCED_FACE('',(#2997),#1911,.T.) ;
#27733 = ADVANCED_FACE('',(#2998),#1912,.T.) ;
#27734 = ADVANCED_FACE('',(#2999),#1913,.F.) ;
#27735 = ADVANCED_FACE('',(#3000),#1914,.F.) ;
#27736 = ADVANCED_FACE('',(#3001),#26775,.F.) ;
#27737 = ADVANCED_FACE('',(#3002),#1915,.F.) ;
#27738 = ADVANCED_FACE('',(#3003),#1916,.F.) ;
#27739 = ADVANCED_FACE('',(#3004),#1917,.F.) ;
#27740 = ADVANCED_FACE('',(#3005),#1918,.F.) ;
#27741 = ADVANCED_FACE('',(#3006),#1919,.T.) ;
#27742 = ADVANCED_FACE('',(#3007),#1920,.T.) ;
#27743 = ADVANCED_FACE('',(#3008),#1921,.F.) ;
#27744 = ADVANCED_FACE('',(#3009),#1922,.F.) ;
#27745 = ADVANCED_FACE('',(#3010),#1923,.F.) ;
#27746 = ADVANCED_FACE('',(#3011),#1924,.F.) ;
#27747 = ADVANCED_FACE('',(#3012),#1925,.F.) ;
#27748 = ADVANCED_FACE('',(#3013),#26776,.F.) ;
#27749 = ADVANCED_FACE('',(#3014,#1270),#1926,.T.) ;
#27750 = ADVANCED_FACE('',(#3015),#26777,.T.) ;
#27751 = ADVANCED_FACE('',(#3016),#1927,.T.) ;
#27752 = ADVANCED_FACE('',(#3017,#1271,#1272),#26778,.T.) ;
#27753 = ADVANCED_FACE('',(#3018),#1928,.T.) ;
#27754 = ADVANCED_FACE('',(#3019),#26779,.F.) ;
#27755 = ADVANCED_FACE('',(#3020,#1273),#1929,.T.) ;
#27756 = ADVANCED_FACE('',(#3021),#26780,.T.) ;
#27757 = ADVANCED_FACE('',(#3022),#1930,.T.) ;
#27758 = ADVANCED_FACE('',(#3023,#1274,#1275),#26781,.T.) ;
#27759 = ADVANCED_FACE('',(#3024),#1931,.T.) ;
#27760 = ADVANCED_FACE('',(#3025),#26782,.F.) ;
#27761 = ADVANCED_FACE('',(#3026),#26783,.F.) ;
#27762 = ADVANCED_FACE('',(#3027),#26784,.F.) ;
#27763 = ADVANCED_FACE('',(#3028),#26785,.F.) ;
#27764 = ADVANCED_FACE('',(#3029),#26786,.F.) ;
#27765 = ADVANCED_FACE('',(#3030),#1932,.F.) ;
#27766 = ADVANCED_FACE('',(#3031),#1933,.T.) ;
#27767 = ADVANCED_FACE('',(#3032),#1934,.F.) ;
#27768 = ADVANCED_FACE('',(#3033),#26787,.F.) ;
#27769 = ADVANCED_FACE('',(#3034,#1276),#1935,.F.) ;
#27770 = ADVANCED_FACE('',(#3035),#1936,.F.) ;
#27771 = ADVANCED_FACE('',(#3036),#26788,.F.) ;
#27772 = ADVANCED_FACE('',(#3037,#1277),#1937,.F.) ;
#27773 = ADVANCED_FACE('',(#3038),#1938,.F.) ;
#27774 = ADVANCED_FACE('',(#3039),#26789,.F.) ;
#27775 = ADVANCED_FACE('',(#3040),#26790,.F.) ;
#27776 = ADVANCED_FACE('',(#3041),#1939,.F.) ;
#27777 = ADVANCED_FACE('',(#3042),#26791,.T.) ;
#27778 = ADVANCED_FACE('',(#3043,#1278),#1940,.T.) ;
#27779 = ADVANCED_FACE('',(#3044),#26792,.F.) ;
#27780 = ADVANCED_FACE('',(#3045),#26793,.F.) ;
#27781 = ADVANCED_FACE('',(#3046),#1941,.F.) ;
#27782 = ADVANCED_FACE('',(#3047),#1942,.F.) ;
#27783 = ADVANCED_FACE('',(#3048),#1943,.F.) ;
#27784 = ADVANCED_FACE('',(#3049),#1944,.F.) ;
#27785 = ADVANCED_FACE('',(#3050),#1945,.F.) ;
#27786 = ADVANCED_FACE('',(#3051),#1946,.F.) ;
#27787 = ADVANCED_FACE('',(#3052),#1947,.F.) ;
#27788 = ADVANCED_FACE('',(#3053),#1948,.F.) ;
#27789 = ADVANCED_FACE('',(#3054),#1949,.F.) ;
#27790 = ADVANCED_FACE('',(#3055),#1950,.F.) ;
#27791 = ADVANCED_FACE('',(#3056),#1951,.F.) ;
#27792 = ADVANCED_FACE('',(#3057),#1952,.F.) ;
#27793 = ADVANCED_FACE('',(#3058),#1953,.F.) ;
#27794 = ADVANCED_FACE('',(#3059),#26794,.F.) ;
#27795 = ADVANCED_FACE('',(#3060),#26795,.T.) ;
#27796 = ADVANCED_FACE('',(#3061),#26796,.F.) ;
#27797 = ADVANCED_FACE('',(#3062),#1954,.F.) ;
#27798 = ADVANCED_FACE('',(#3063,#1279),#1955,.T.) ;
#27799 = ADVANCED_FACE('',(#3064),#26797,.F.) ;
#27800 = ADVANCED_FACE('',(#3065),#1956,.F.) ;
#27801 = ADVANCED_FACE('',(#3066),#26798,.T.) ;
#27802 = ADVANCED_FACE('',(#3067,#1280),#1957,.T.) ;
#27803 = ADVANCED_FACE('',(#3068),#26799,.F.) ;
#27804 = ADVANCED_FACE('',(#3069),#1958,.F.) ;
#27805 = ADVANCED_FACE('',(#3070),#26800,.T.) ;
#27806 = ADVANCED_FACE('',(#3071,#1281),#1959,.T.) ;
#27807 = ADVANCED_FACE('',(#3072,#1282),#1960,.T.) ;
#27808 = ADVANCED_FACE('',(#3073,#1283),#1961,.F.) ;
#27809 = ADVANCED_FACE('',(#3074),#1962,.F.) ;
#27810 = ADVANCED_FACE('',(#3075),#1963,.F.) ;
#27811 = ADVANCED_FACE('',(#3076,#1284),#1964,.F.) ;
#27812 = ADVANCED_FACE('',(#3077,#1285),#1965,.T.) ;
#27813 = ADVANCED_FACE('',(#3078,#1286),#1966,.F.) ;
#27814 = ADVANCED_FACE('',(#3079),#1967,.F.) ;
#27815 = ADVANCED_FACE('',(#3080),#1968,.F.) ;
#27816 = ADVANCED_FACE('',(#3081,#1287),#1969,.T.) ;
#27817 = ADVANCED_FACE('',(#3082,#1288),#1970,.F.) ;
#27818 = ADVANCED_FACE('',(#3083),#1971,.F.) ;
#27819 = ADVANCED_FACE('',(#3084),#1972,.F.) ;
#27820 = ADVANCED_FACE('',(#3085,#1289),#1973,.T.) ;
#27821 = ADVANCED_FACE('',(#3086,#1290),#1974,.F.) ;
#27822 = ADVANCED_FACE('',(#3087),#1975,.F.) ;
#27823 = ADVANCED_FACE('',(#3088),#1976,.F.) ;
#27824 = ADVANCED_FACE('',(#3089),#1977,.F.) ;
#27825 = ADVANCED_FACE('',(#3090,#1291,#1292,#1293),#1978,.F.) ;
#27826 = ADVANCED_FACE('',(#3091),#26801,.T.) ;
#27827 = ADVANCED_FACE('',(#3092),#1979,.T.) ;
#27828 = ADVANCED_FACE('',(#3093),#1980,.F.) ;
#27829 = ADVANCED_FACE('',(#3094),#1981,.F.) ;
#27830 = ADVANCED_FACE('',(#3095,#1294),#1982,.T.) ;
#27831 = ADVANCED_FACE('',(#3096),#1983,.F.) ;
#27832 = ADVANCED_FACE('',(#3097),#1984,.F.) ;
#27833 = ADVANCED_FACE('',(#3098),#1985,.F.) ;
#27834 = ADVANCED_FACE('',(#3099),#1986,.F.) ;
#27835 = ADVANCED_FACE('',(#3100),#1987,.T.) ;
#27836 = ADVANCED_FACE('',(#3101),#1988,.F.) ;
#27837 = ADVANCED_FACE('',(#3102),#1989,.F.) ;
#27838 = ADVANCED_FACE('',(#3103),#1990,.F.) ;
#27839 = ADVANCED_FACE('',(#3104),#1991,.F.) ;
#27840 = ADVANCED_FACE('',(#3105),#1992,.F.) ;
#27841 = ADVANCED_FACE('',(#3106),#1993,.F.) ;
#27842 = ADVANCED_FACE('',(#3107),#26802,.T.) ;
#27843 = ADVANCED_FACE('',(#3108),#26803,.T.) ;
#27844 = ADVANCED_FACE('',(#3109),#26804,.T.) ;
#27845 = ADVANCED_FACE('',(#3110),#26805,.T.) ;
#27846 = ADVANCED_FACE('',(#3111),#26806,.T.) ;
#27847 = ADVANCED_FACE('',(#3112),#26807,.T.) ;
#27848 = ADVANCED_FACE('',(#3113),#1994,.F.) ;
#27849 = ADVANCED_FACE('',(#3114),#1995,.F.) ;
#27850 = ADVANCED_FACE('',(#3115),#1996,.F.) ;
#27851 = ADVANCED_FACE('',(#3116),#1997,.F.) ;
#27852 = ADVANCED_FACE('',(#3117),#1998,.F.) ;
#27853 = ADVANCED_FACE('',(#3118),#1999,.F.) ;
#27854 = ADVANCED_FACE('',(#3119),#2000,.T.) ;
#27855 = ADVANCED_FACE('',(#3120),#2001,.F.) ;
#27856 = ADVANCED_FACE('',(#3121),#2002,.F.) ;
#27857 = ADVANCED_FACE('',(#3122),#2003,.T.) ;
#27858 = ADVANCED_FACE('',(#3123),#2004,.F.) ;
#27859 = ADVANCED_FACE('',(#3124),#2005,.F.) ;
#27860 = ADVANCED_FACE('',(#3125),#2006,.T.) ;
#27861 = ADVANCED_FACE('',(#3126),#2007,.T.) ;
#27862 = ADVANCED_FACE('',(#3127),#2008,.F.) ;
#27863 = ADVANCED_FACE('',(#3128),#2009,.T.) ;
#27864 = ADVANCED_FACE('',(#3129),#2010,.T.) ;
#27865 = ADVANCED_FACE('',(#3130),#2011,.F.) ;
#27866 = ADVANCED_FACE('',(#3131),#26808,.T.) ;
#27867 = ADVANCED_FACE('',(#3132),#26809,.T.) ;
#27868 = ADVANCED_FACE('',(#3133),#26810,.T.) ;
#27869 = ADVANCED_FACE('',(#3134),#26811,.T.) ;
#27870 = ADVANCED_FACE('',(#3135),#26812,.T.) ;
#27871 = ADVANCED_FACE('',(#3136),#26813,.T.) ;
#27872 = ADVANCED_FACE('',(#3137),#2012,.T.) ;
#27873 = ADVANCED_FACE('',(#3138),#2013,.T.) ;
#27874 = ADVANCED_FACE('',(#3139),#2014,.F.) ;
#27875 = ADVANCED_FACE('',(#3140),#2015,.T.) ;
#27876 = ADVANCED_FACE('',(#3141),#2016,.T.) ;
#27877 = ADVANCED_FACE('',(#3142),#2017,.T.) ;
#27878 = ADVANCED_FACE('',(#3143),#2018,.T.) ;
#27879 = ADVANCED_FACE('',(#3144),#2019,.T.) ;
#27880 = ADVANCED_FACE('',(#3145),#26814,.T.) ;
#27881 = ADVANCED_FACE('',(#3146),#2020,.F.) ;
#27882 = ADVANCED_FACE('',(#3147),#2021,.T.) ;
#27883 = ADVANCED_FACE('',(#3148),#2022,.T.) ;
#27884 = ADVANCED_FACE('',(#3149),#2023,.T.) ;
#27885 = ADVANCED_FACE('',(#3150),#2024,.T.) ;
#27886 = ADVANCED_FACE('',(#3151),#2025,.T.) ;
#27887 = ADVANCED_FACE('',(#3152),#2026,.T.) ;
#27888 = ADVANCED_FACE('',(#3153),#2027,.T.) ;
#27889 = ADVANCED_FACE('',(#3154),#2028,.T.) ;
#27890 = ADVANCED_FACE('',(#3155),#26815,.T.) ;
#27891 = ADVANCED_FACE('',(#3156),#2029,.T.) ;
#27892 = ADVANCED_FACE('',(#3157,#1295),#2030,.T.) ;
#27893 = ADVANCED_FACE('',(#3158),#26816,.T.) ;
#27894 = ADVANCED_FACE('',(#3159,#1296),#2031,.T.) ;
#27895 = ADVANCED_FACE('',(#3160),#26817,.F.) ;
#27896 = ADVANCED_FACE('',(#3161),#26818,.T.) ;
#27897 = ADVANCED_FACE('',(#3162,#1297),#2032,.T.) ;
#27898 = ADVANCED_FACE('',(#3163,#1298),#2033,.T.) ;
#27899 = ADVANCED_FACE('',(#3164),#2034,.T.) ;
#27900 = ADVANCED_FACE('',(#3165),#2035,.T.) ;
#27901 = ADVANCED_FACE('',(#3166),#2036,.F.) ;
#27902 = ADVANCED_FACE('',(#3167),#2037,.T.) ;
#27903 = ADVANCED_FACE('',(#3168),#26819,.T.) ;
#27904 = ADVANCED_FACE('',(#3169),#26820,.F.) ;
#27905 = ADVANCED_FACE('',(#3170),#2038,.F.) ;
#27906 = ADVANCED_FACE('',(#3171),#2039,.T.) ;
#27907 = ADVANCED_FACE('',(#3172),#2040,.F.) ;
#27908 = ADVANCED_FACE('',(#3173),#2041,.T.) ;
#27909 = ADVANCED_FACE('',(#3174),#2042,.F.) ;
#27910 = ADVANCED_FACE('',(#3175),#2043,.F.) ;
#27911 = ADVANCED_FACE('',(#3176),#2044,.F.) ;
#27912 = ADVANCED_FACE('',(#3177),#2045,.T.) ;
#27913 = ADVANCED_FACE('',(#3178),#26821,.T.) ;
#27914 = ADVANCED_FACE('',(#3179),#2046,.T.) ;
#27915 = ADVANCED_FACE('',(#3180),#2047,.T.) ;
#27916 = ADVANCED_FACE('',(#3181),#26822,.T.) ;
#27917 = ADVANCED_FACE('',(#3182),#2048,.T.) ;
#27918 = ADVANCED_FACE('',(#3183),#26823,.F.) ;
#27919 = ADVANCED_FACE('',(#3184),#26824,.T.) ;
#27920 = ADVANCED_FACE('',(#3185,#1299,#1300),#2049,.T.) ;
#27921 = ADVANCED_FACE('',(#3186,#1301),#2050,.T.) ;
#27922 = ADVANCED_FACE('',(#3187),#26825,.F.) ;
#27923 = ADVANCED_FACE('',(#3188),#26826,.T.) ;
#27924 = ADVANCED_FACE('',(#3189,#1302),#2051,.T.) ;
#27925 = ADVANCED_FACE('',(#3190,#1303),#2052,.T.) ;
#27926 = ADVANCED_FACE('',(#3191),#26827,.F.) ;
#27927 = ADVANCED_FACE('',(#3192),#26828,.T.) ;
#27928 = ADVANCED_FACE('',(#3193,#1304),#2053,.T.) ;
#27929 = ADVANCED_FACE('',(#3194,#1305),#2054,.T.) ;
#27930 = ADVANCED_FACE('',(#3195),#26829,.T.) ;
#27931 = ADVANCED_FACE('',(#3196),#2055,.T.) ;
#27932 = ADVANCED_FACE('',(#3197),#2056,.T.) ;
#27933 = ADVANCED_FACE('',(#3198,#1306),#2057,.T.) ;
#27934 = ADVANCED_FACE('',(#3199,#1307),#2058,.T.) ;
#27935 = ADVANCED_FACE('',(#3200),#26830,.T.) ;
#27936 = ADVANCED_FACE('',(#3201,#1308,#1309,#1310,#1311,#1312,#1313),#26831,
 .T.) ;
#27937 = ADVANCED_FACE('',(#3202),#2059,.T.) ;
#27938 = ADVANCED_FACE('',(#3203),#2060,.F.) ;
#27939 = ADVANCED_FACE('',(#3204),#2061,.F.) ;
#27940 = ADVANCED_FACE('',(#3205),#2062,.F.) ;
#27941 = ADVANCED_FACE('',(#3206),#2063,.F.) ;
#27942 = ADVANCED_FACE('',(#3207),#2064,.F.) ;
#27943 = ADVANCED_FACE('',(#3208),#2065,.T.) ;
#27944 = ADVANCED_FACE('',(#3209),#2066,.F.) ;
#27945 = ADVANCED_FACE('',(#3210),#2067,.F.) ;
#27946 = ADVANCED_FACE('',(#3211),#2068,.F.) ;
#27947 = ADVANCED_FACE('',(#3212),#2069,.T.) ;
#27948 = ADVANCED_FACE('',(#3213),#2070,.F.) ;
#27949 = ADVANCED_FACE('',(#3214),#2071,.F.) ;
#27950 = ADVANCED_FACE('',(#3215),#2072,.F.) ;
#27951 = ADVANCED_FACE('',(#3216),#2073,.F.) ;
#27952 = ADVANCED_FACE('',(#3217),#2074,.F.) ;
#27953 = ADVANCED_FACE('',(#3218),#2075,.T.) ;
#27954 = ADVANCED_FACE('',(#3219),#2076,.F.) ;
#27955 = ADVANCED_FACE('',(#3220),#2077,.F.) ;
#27956 = ADVANCED_FACE('',(#3221),#2078,.F.) ;
#27957 = ADVANCED_FACE('',(#3222),#2079,.T.) ;
#27958 = ADVANCED_FACE('',(#3223),#2080,.F.) ;
#27959 = ADVANCED_FACE('',(#3224),#2081,.F.) ;
#27960 = ADVANCED_FACE('',(#3225),#2082,.F.) ;
#27961 = ADVANCED_FACE('',(#3226),#2083,.F.) ;
#27962 = ADVANCED_FACE('',(#3227),#2084,.F.) ;
#27963 = ADVANCED_FACE('',(#3228),#2085,.T.) ;
#27964 = ADVANCED_FACE('',(#3229),#2086,.F.) ;
#27965 = ADVANCED_FACE('',(#3230),#2087,.F.) ;
#27966 = ADVANCED_FACE('',(#3231),#2088,.F.) ;
#27967 = ADVANCED_FACE('',(#3232),#2089,.T.) ;
#27968 = ADVANCED_FACE('',(#3233),#2090,.F.) ;
#27969 = ADVANCED_FACE('',(#3234),#2091,.F.) ;
#27970 = ADVANCED_FACE('',(#3235),#2092,.F.) ;
#27971 = ADVANCED_FACE('',(#3236),#2093,.F.) ;
#27972 = ADVANCED_FACE('',(#3237),#2094,.F.) ;
#27973 = ADVANCED_FACE('',(#3238),#2095,.T.) ;
#27974 = ADVANCED_FACE('',(#3239),#2096,.F.) ;
#27975 = ADVANCED_FACE('',(#3240),#2097,.F.) ;
#27976 = ADVANCED_FACE('',(#3241),#2098,.F.) ;
#27977 = ADVANCED_FACE('',(#3242),#26832,.T.) ;
#27978 = ADVANCED_FACE('',(#3243),#2099,.T.) ;
#27979 = ADVANCED_FACE('',(#3244),#2100,.T.) ;
#27980 = ADVANCED_FACE('',(#3245),#26833,.F.) ;
#27981 = ADVANCED_FACE('',(#3246),#26834,.T.) ;
#27982 = ADVANCED_FACE('',(#3247,#1314),#2101,.T.) ;
#27983 = ADVANCED_FACE('',(#3248,#1315),#2102,.T.) ;
#27984 = ADVANCED_FACE('',(#3249),#26835,.F.) ;
#27985 = ADVANCED_FACE('',(#3250,#1316),#2103,.F.) ;
#27986 = ADVANCED_FACE('',(#3251),#2104,.F.) ;
#27987 = ADVANCED_FACE('',(#3252),#2105,.F.) ;
#27988 = ADVANCED_FACE('',(#3253),#2106,.F.) ;
#27989 = ADVANCED_FACE('',(#3254,#1317),#2107,.T.) ;
#27990 = ADVANCED_FACE('',(#3255),#2108,.F.) ;
#27991 = ADVANCED_FACE('',(#3256),#2109,.F.) ;
#27992 = ADVANCED_FACE('',(#3257),#26836,.F.) ;
#27993 = ADVANCED_FACE('',(#3258),#2110,.T.) ;
#27994 = ADVANCED_FACE('',(#3259),#2111,.F.) ;
#27995 = ADVANCED_FACE('',(#3260,#1318),#2112,.F.) ;
#27996 = ADVANCED_FACE('',(#3261),#2113,.F.) ;
#27997 = ADVANCED_FACE('',(#3262,#1319),#2114,.F.) ;
#27998 = ADVANCED_FACE('',(#3263),#26837,.F.) ;
#27999 = ADVANCED_FACE('',(#3264),#26838,.F.) ;
#28000 = ADVANCED_FACE('',(#3265),#26839,.F.) ;
#28001 = ADVANCED_FACE('',(#3266),#26840,.F.) ;
#28002 = ADVANCED_FACE('',(#3267),#26841,.F.) ;
#28003 = ADVANCED_FACE('',(#3268,#1320,#1321),#2115,.T.) ;
#28004 = ADVANCED_FACE('',(#3269),#2116,.F.) ;
#28005 = ADVANCED_FACE('',(#3270,#1322,#1323),#2117,.T.) ;
#28006 = ADVANCED_FACE('',(#3271),#2118,.F.) ;
#28007 = ADVANCED_FACE('',(#3272),#2119,.F.) ;
#28008 = ADVANCED_FACE('',(#3273),#2120,.F.) ;
#28009 = ADVANCED_FACE('',(#3274),#2121,.F.) ;
#28010 = ADVANCED_FACE('',(#3275,#1324,#1325),#2122,.T.) ;
#28011 = ADVANCED_FACE('',(#3276),#2123,.F.) ;
#28012 = ADVANCED_FACE('',(#3277),#2124,.F.) ;
#28013 = ADVANCED_FACE('',(#3278),#2125,.F.) ;
#28014 = ADVANCED_FACE('',(#3279),#26842,.F.) ;
#28015 = ADVANCED_FACE('',(#3280,#1326,#1327,#1328,#1329,#1330,#1331),#2126,
 .F.) ;
#28016 = ADVANCED_FACE('',(#3281),#26843,.F.) ;
#28017 = ADVANCED_FACE('',(#3282),#2127,.F.) ;
#28018 = ADVANCED_FACE('',(#3283),#2128,.F.) ;
#28019 = ADVANCED_FACE('',(#3284),#2129,.F.) ;
#28020 = ADVANCED_FACE('',(#3285),#2130,.F.) ;
#28021 = ADVANCED_FACE('',(#3286),#2131,.F.) ;
#28022 = ADVANCED_FACE('',(#3287),#2132,.F.) ;
#28023 = ADVANCED_FACE('',(#3288),#2133,.T.) ;
#28024 = ADVANCED_FACE('',(#3289),#2134,.F.) ;
#28025 = ADVANCED_FACE('',(#3290),#2135,.F.) ;
#28026 = ADVANCED_FACE('',(#3291),#2136,.F.) ;
#28027 = ADVANCED_FACE('',(#3292),#2137,.F.) ;
#28028 = ADVANCED_FACE('',(#3293),#26844,.F.) ;
#28029 = ADVANCED_FACE('',(#3294),#2138,.F.) ;
#28030 = ADVANCED_FACE('',(#3295),#2139,.F.) ;
#28031 = ADVANCED_FACE('',(#3296),#2140,.F.) ;
#28032 = ADVANCED_FACE('',(#3297),#2141,.F.) ;
#28033 = ADVANCED_FACE('',(#3298),#2142,.F.) ;
#28034 = ADVANCED_FACE('',(#3299),#26845,.F.) ;
#28035 = ADVANCED_FACE('',(#3300),#2143,.F.) ;
#28036 = ADVANCED_FACE('',(#3301),#2144,.F.) ;
#28037 = ADVANCED_FACE('',(#3302),#2145,.F.) ;
#28038 = ADVANCED_FACE('',(#3303),#2146,.F.) ;
#28039 = ADVANCED_FACE('',(#3304),#2147,.F.) ;
#28040 = ADVANCED_FACE('',(#3305),#26846,.F.) ;
#28041 = ADVANCED_FACE('',(#3306,#1332,#1333,#1334),#2148,.T.) ;
#28042 = ADVANCED_FACE('',(#3307,#1335,#1336,#1337),#2149,.F.) ;
#28043 = ADVANCED_FACE('',(#3308),#2150,.F.) ;
#28044 = ADVANCED_FACE('',(#3309),#2151,.F.) ;
#28045 = ADVANCED_FACE('',(#3310),#2152,.T.) ;
#28046 = ADVANCED_FACE('',(#3311),#2153,.T.) ;
#28047 = ADVANCED_FACE('',(#3312),#2154,.T.) ;
#28048 = ADVANCED_FACE('',(#3313),#2155,.T.) ;
#28049 = ADVANCED_FACE('',(#3314),#2156,.F.) ;
#28050 = ADVANCED_FACE('',(#3315),#2157,.T.) ;
#28051 = ADVANCED_FACE('',(#3316),#2158,.T.) ;
#28052 = ADVANCED_FACE('',(#3317),#2159,.T.) ;
#28053 = ADVANCED_FACE('',(#3318),#2160,.T.) ;
#28054 = ADVANCED_FACE('',(#3319),#2161,.T.) ;
#28055 = ADVANCED_FACE('',(#3320),#2162,.T.) ;
#28056 = ADVANCED_FACE('',(#3321),#2163,.T.) ;
#28057 = ADVANCED_FACE('',(#3322),#2164,.T.) ;
#28058 = ADVANCED_FACE('',(#3323),#2165,.T.) ;
#28059 = ADVANCED_FACE('',(#3324),#2166,.T.) ;
#28060 = ADVANCED_FACE('',(#3325),#2167,.T.) ;
#28061 = ADVANCED_FACE('',(#3326),#2168,.T.) ;
#28062 = ADVANCED_FACE('',(#3327),#2169,.T.) ;
#28063 = ADVANCED_FACE('',(#3328),#2170,.T.) ;
#28064 = ADVANCED_FACE('',(#3329),#2171,.T.) ;
#28065 = ADVANCED_FACE('',(#3330),#2172,.T.) ;
#28066 = ADVANCED_FACE('',(#3331),#2173,.T.) ;
#28067 = ADVANCED_FACE('',(#3332),#2174,.T.) ;
#28068 = ADVANCED_FACE('',(#3333),#2175,.T.) ;
#28069 = ADVANCED_FACE('',(#3334),#2176,.T.) ;
#28070 = ADVANCED_FACE('',(#3335),#2177,.T.) ;
#28071 = ADVANCED_FACE('',(#3336),#2178,.T.) ;
#28072 = ADVANCED_FACE('',(#3337),#2179,.T.) ;
#28073 = ADVANCED_FACE('',(#3338),#2180,.T.) ;
#28074 = ADVANCED_FACE('',(#3339),#2181,.T.) ;
#28075 = ADVANCED_FACE('',(#3340),#2182,.T.) ;
#28076 = ADVANCED_FACE('',(#3341),#2183,.T.) ;
#28077 = ADVANCED_FACE('',(#3342),#2184,.T.) ;
#28078 = ADVANCED_FACE('',(#3343),#2185,.T.) ;
#28079 = ADVANCED_FACE('',(#3344),#2186,.T.) ;
#28080 = ADVANCED_FACE('',(#3345),#2187,.T.) ;
#28081 = ADVANCED_FACE('',(#3346),#2188,.T.) ;
#28082 = ADVANCED_FACE('',(#3347),#2189,.T.) ;
#28083 = ADVANCED_FACE('',(#3348),#2190,.F.) ;
#28084 = ADVANCED_FACE('',(#3349),#2191,.F.) ;
#28085 = ADVANCED_FACE('',(#3350),#2192,.F.) ;
#28086 = ADVANCED_FACE('',(#3351),#2193,.F.) ;
#28087 = ADVANCED_FACE('',(#3352),#26847,.F.) ;
#28088 = ADVANCED_FACE('',(#3353),#26848,.F.) ;
#28089 = ADVANCED_FACE('',(#3354),#26849,.F.) ;
#28090 = ADVANCED_FACE('',(#3355),#26850,.F.) ;
#28091 = ADVANCED_FACE('',(#3356,#1338),#26851,.F.) ;
#28092 = ADVANCED_FACE('',(#3357,#1339,#1340,#1341,#1342,#1343),#2194,.F.) ;
#28093 = ADVANCED_FACE('',(#3358),#26852,.F.) ;
#28094 = ADVANCED_FACE('',(#3359),#1092,.T.) ;
#28095 = ADVANCED_FACE('',(#3360,#1344,#1345,#1346,#1347,#1348),#2195,.T.) ;
#28096 = ADVANCED_FACE('',(#3361),#2196,.F.) ;
#28097 = ADVANCED_FACE('',(#3362),#2197,.F.) ;
#28098 = ADVANCED_FACE('',(#3363),#2198,.F.) ;
#28099 = ADVANCED_FACE('',(#3364),#2199,.F.) ;
#28100 = ADVANCED_FACE('',(#3365),#1093,.F.) ;
#28101 = ADVANCED_FACE('',(#3366,#1349),#2200,.T.) ;
#28102 = ADVANCED_FACE('',(#3367),#26853,.F.) ;
#28103 = ADVANCED_FACE('',(#3368),#26854,.F.) ;
#28104 = ADVANCED_FACE('',(#3369),#26855,.T.) ;
#28105 = ADVANCED_FACE('',(#3370,#1350),#2201,.T.) ;
#28106 = ADVANCED_FACE('',(#3371,#1351),#2202,.T.) ;
#28107 = ADVANCED_FACE('',(#3372,#1352),#2203,.T.) ;
#28108 = ADVANCED_FACE('',(#3373,#1353),#2204,.T.) ;
#28109 = ADVANCED_FACE('',(#3374),#1094,.T.) ;
#28110 = ADVANCED_FACE('',(#3375),#1095,.F.) ;
#28111 = ADVANCED_FACE('',(#3376),#26856,.F.) ;
#28112 = ADVANCED_FACE('',(#3377),#26857,.F.) ;
#28113 = ADVANCED_FACE('',(#3378),#26858,.F.) ;
#28114 = ADVANCED_FACE('',(#3379),#26859,.F.) ;
#28115 = ADVANCED_FACE('',(#3380),#26860,.F.) ;
#28116 = ADVANCED_FACE('',(#3381),#26861,.F.) ;
#28117 = ADVANCED_FACE('',(#3382),#26862,.F.) ;
#28118 = ADVANCED_FACE('',(#3383),#26863,.F.) ;
#28119 = ADVANCED_FACE('',(#3384),#2205,.F.) ;
#28120 = ADVANCED_FACE('',(#3385,#1354,#1355,#1356,#1357,#1358,#1359,#1360,
#1361),#2206,.T.) ;
#28121 = ADVANCED_FACE('',(#3386,#1362,#1363,#1364,#1365,#1366,#1367,#1368,
#1369),#2207,.T.) ;
#28122 = ADVANCED_FACE('',(#3387),#26864,.T.) ;
#28123 = ADVANCED_FACE('',(#3388),#26865,.T.) ;
#28124 = ADVANCED_FACE('',(#3389),#2208,.T.) ;
#28125 = ADVANCED_FACE('',(#3390),#2209,.F.) ;
#28126 = ADVANCED_FACE('',(#3391),#2210,.F.) ;
#28127 = ADVANCED_FACE('',(#3392),#26866,.F.) ;
#28128 = ADVANCED_FACE('',(#3393,#1370),#2211,.F.) ;
#28129 = ADVANCED_FACE('',(#3394),#2212,.F.) ;
#28130 = ADVANCED_FACE('',(#3395),#26867,.F.) ;
#28131 = ADVANCED_FACE('',(#3396),#26868,.F.) ;
#28132 = ADVANCED_FACE('',(#3397,#1371),#2213,.F.) ;
#28133 = ADVANCED_FACE('',(#3398,#1372),#2214,.T.) ;
#28134 = ADVANCED_FACE('',(#3399,#1373),#2215,.F.) ;
#28135 = ADVANCED_FACE('',(#3400),#2216,.F.) ;
#28136 = ADVANCED_FACE('',(#3401,#1374),#2217,.F.) ;
#28137 = ADVANCED_FACE('',(#3402),#2218,.F.) ;
#28138 = ADVANCED_FACE('',(#3403),#2219,.F.) ;
#28139 = ADVANCED_FACE('',(#3404),#2220,.F.) ;
#28140 = ADVANCED_FACE('',(#3405),#2221,.T.) ;
#28141 = ADVANCED_FACE('',(#3406),#2222,.F.) ;
#28142 = ADVANCED_FACE('',(#3407),#2223,.F.) ;
#28143 = ADVANCED_FACE('',(#3408),#2224,.F.) ;
#28144 = ADVANCED_FACE('',(#3409),#2225,.F.) ;
#28145 = ADVANCED_FACE('',(#3410),#2226,.F.) ;
#28146 = ADVANCED_FACE('',(#3411,#1375),#2227,.F.) ;
#28147 = ADVANCED_FACE('',(#3412),#26869,.T.) ;
#28148 = ADVANCED_FACE('',(#3413),#2228,.T.) ;
#28149 = ADVANCED_FACE('',(#3414),#727,.T.) ;
#28150 = ADVANCED_FACE('',(#3415,#1376),#2229,.T.) ;
#28151 = ADVANCED_FACE('',(#3416),#26870,.T.) ;
#28152 = ADVANCED_FACE('',(#3417),#2230,.T.) ;
#28153 = ADVANCED_FACE('',(#3418),#26871,.T.) ;
#28154 = ADVANCED_FACE('',(#3419),#2231,.T.) ;
#28155 = ADVANCED_FACE('',(#3420),#728,.F.) ;
#28156 = ADVANCED_FACE('',(#3421),#729,.F.) ;
#28157 = ADVANCED_FACE('',(#3422),#730,.F.) ;
#28158 = ADVANCED_FACE('',(#3423),#731,.T.) ;
#28159 = ADVANCED_FACE('',(#3424),#26872,.F.) ;
#28160 = ADVANCED_FACE('',(#3425),#732,.T.) ;
#28161 = ADVANCED_FACE('',(#3426),#733,.T.) ;
#28162 = ADVANCED_FACE('',(#3427),#734,.T.) ;
#28163 = ADVANCED_FACE('',(#3428),#735,.T.) ;
#28164 = ADVANCED_FACE('',(#3429),#736,.T.) ;
#28165 = ADVANCED_FACE('',(#3430),#26873,.F.) ;
#28166 = ADVANCED_FACE('',(#3431),#26874,.F.) ;
#28167 = ADVANCED_FACE('',(#3432),#26875,.T.) ;
#28168 = ADVANCED_FACE('',(#3433,#1377),#2232,.T.) ;
#28169 = ADVANCED_FACE('',(#3434),#26876,.T.) ;
#28170 = ADVANCED_FACE('',(#3435),#26877,.T.) ;
#28171 = ADVANCED_FACE('',(#3436),#26878,.T.) ;
#28172 = ADVANCED_FACE('',(#3437),#26879,.T.) ;
#28173 = ADVANCED_FACE('',(#3438),#26880,.T.) ;
#28174 = ADVANCED_FACE('',(#3439),#26881,.T.) ;
#28175 = ADVANCED_FACE('',(#3440,#1378),#2233,.T.) ;
#28176 = ADVANCED_FACE('',(#3441),#737,.T.) ;
#28177 = ADVANCED_FACE('',(#3442),#738,.T.) ;
#28178 = ADVANCED_FACE('',(#3443),#739,.T.) ;
#28179 = ADVANCED_FACE('',(#3444),#740,.T.) ;
#28180 = ADVANCED_FACE('',(#3445),#741,.T.) ;
#28181 = ADVANCED_FACE('',(#3446),#26882,.F.) ;
#28182 = ADVANCED_FACE('',(#3447),#26883,.T.) ;
#28183 = ADVANCED_FACE('',(#3448),#742,.F.) ;
#28184 = ADVANCED_FACE('',(#3449),#743,.T.) ;
#28185 = ADVANCED_FACE('',(#3450),#26884,.T.) ;
#28186 = ADVANCED_FACE('',(#3451),#26885,.T.) ;
#28187 = ADVANCED_FACE('',(#3452),#26886,.F.) ;
#28188 = ADVANCED_FACE('',(#3453),#744,.T.) ;
#28189 = ADVANCED_FACE('',(#3454),#745,.T.) ;
#28190 = ADVANCED_FACE('',(#3455),#26887,.T.) ;
#28191 = ADVANCED_FACE('',(#3456),#26888,.F.) ;
#28192 = ADVANCED_FACE('',(#3457),#26889,.T.) ;
#28193 = ADVANCED_FACE('',(#3458),#746,.T.) ;
#28194 = ADVANCED_FACE('',(#3459),#747,.F.) ;
#28195 = ADVANCED_FACE('',(#3460),#26890,.T.) ;
#28196 = ADVANCED_FACE('',(#3461),#2234,.T.) ;
#28197 = ADVANCED_FACE('',(#3462),#2235,.T.) ;
#28198 = ADVANCED_FACE('',(#3463),#2236,.T.) ;
#28199 = ADVANCED_FACE('',(#3464),#26891,.T.) ;
#28200 = ADVANCED_FACE('',(#3465),#2237,.T.) ;
#28201 = ADVANCED_FACE('',(#3466),#26892,.T.) ;
#28202 = ADVANCED_FACE('',(#3467),#2238,.T.) ;
#28203 = ADVANCED_FACE('',(#3468),#2239,.T.) ;
#28204 = ADVANCED_FACE('',(#3469),#26893,.T.) ;
#28205 = ADVANCED_FACE('',(#3470),#2240,.T.) ;
#28206 = ADVANCED_FACE('',(#3471),#2241,.T.) ;
#28207 = ADVANCED_FACE('',(#3472),#26894,.T.) ;
#28208 = ADVANCED_FACE('',(#3473),#2242,.T.) ;
#28209 = ADVANCED_FACE('',(#3474),#2243,.T.) ;
#28210 = ADVANCED_FACE('',(#3475,#1379),#26895,.T.) ;
#28211 = ADVANCED_FACE('',(#3476),#26896,.F.) ;
#28212 = ADVANCED_FACE('',(#3477,#1380),#2244,.T.) ;
#28213 = ADVANCED_FACE('',(#3478,#1381),#2245,.T.) ;
#28214 = ADVANCED_FACE('',(#3479),#26897,.T.) ;
#28215 = ADVANCED_FACE('',(#3480),#2246,.T.) ;
#28216 = ADVANCED_FACE('',(#3481),#26898,.F.) ;
#28217 = ADVANCED_FACE('',(#3482),#26899,.T.) ;
#28218 = ADVANCED_FACE('',(#3483,#1382),#2247,.T.) ;
#28219 = ADVANCED_FACE('',(#3484,#1383),#2248,.T.) ;
#28220 = ADVANCED_FACE('',(#3485),#26900,.F.) ;
#28221 = ADVANCED_FACE('',(#3486),#26901,.T.) ;
#28222 = ADVANCED_FACE('',(#3487,#1384),#2249,.T.) ;
#28223 = ADVANCED_FACE('',(#3488,#1385),#2250,.T.) ;
#28224 = ADVANCED_FACE('',(#3489),#2251,.T.) ;
#28225 = ADVANCED_FACE('',(#3490),#748,.T.) ;
#28226 = ADVANCED_FACE('',(#3491),#749,.T.) ;
#28227 = ADVANCED_FACE('',(#3492),#750,.T.) ;
#28228 = ADVANCED_FACE('',(#3493),#751,.T.) ;
#28229 = ADVANCED_FACE('',(#3494),#752,.T.) ;
#28230 = ADVANCED_FACE('',(#3495),#753,.T.) ;
#28231 = ADVANCED_FACE('',(#3496),#754,.T.) ;
#28232 = ADVANCED_FACE('',(#3497),#755,.T.) ;
#28233 = ADVANCED_FACE('',(#3498),#756,.T.) ;
#28234 = ADVANCED_FACE('',(#3499),#757,.T.) ;
#28235 = ADVANCED_FACE('',(#3500),#758,.T.) ;
#28236 = ADVANCED_FACE('',(#3501),#759,.T.) ;
#28237 = ADVANCED_FACE('',(#3502),#760,.T.) ;
#28238 = ADVANCED_FACE('',(#3503),#761,.T.) ;
#28239 = ADVANCED_FACE('',(#3504),#762,.T.) ;
#28240 = ADVANCED_FACE('',(#3505),#763,.T.) ;
#28241 = ADVANCED_FACE('',(#3506),#764,.T.) ;
#28242 = ADVANCED_FACE('',(#3507),#765,.T.) ;
#28243 = ADVANCED_FACE('',(#3508),#766,.T.) ;
#28244 = ADVANCED_FACE('',(#3509),#767,.T.) ;
#28245 = ADVANCED_FACE('',(#3510),#768,.T.) ;
#28246 = ADVANCED_FACE('',(#3511),#769,.T.) ;
#28247 = ADVANCED_FACE('',(#3512),#770,.T.) ;
#28248 = ADVANCED_FACE('',(#3513),#771,.T.) ;
#28249 = ADVANCED_FACE('',(#3514),#772,.T.) ;
#28250 = ADVANCED_FACE('',(#3515),#773,.T.) ;
#28251 = ADVANCED_FACE('',(#3516),#774,.T.) ;
#28252 = ADVANCED_FACE('',(#3517),#775,.T.) ;
#28253 = ADVANCED_FACE('',(#3518),#776,.T.) ;
#28254 = ADVANCED_FACE('',(#3519),#777,.T.) ;
#28255 = ADVANCED_FACE('',(#3520),#778,.T.) ;
#28256 = ADVANCED_FACE('',(#3521),#779,.T.) ;
#28257 = ADVANCED_FACE('',(#3522),#780,.T.) ;
#28258 = ADVANCED_FACE('',(#3523),#781,.T.) ;
#28259 = ADVANCED_FACE('',(#3524),#782,.T.) ;
#28260 = ADVANCED_FACE('',(#3525),#783,.T.) ;
#28261 = ADVANCED_FACE('',(#3526),#784,.T.) ;
#28262 = ADVANCED_FACE('',(#3527),#785,.T.) ;
#28263 = ADVANCED_FACE('',(#3528),#786,.T.) ;
#28264 = ADVANCED_FACE('',(#3529),#787,.T.) ;
#28265 = ADVANCED_FACE('',(#3530),#788,.T.) ;
#28266 = ADVANCED_FACE('',(#3531),#789,.T.) ;
#28267 = ADVANCED_FACE('',(#3532),#790,.T.) ;
#28268 = ADVANCED_FACE('',(#3533),#791,.T.) ;
#28269 = ADVANCED_FACE('',(#3534),#792,.T.) ;
#28270 = ADVANCED_FACE('',(#3535),#793,.T.) ;
#28271 = ADVANCED_FACE('',(#3536),#794,.T.) ;
#28272 = ADVANCED_FACE('',(#3537),#795,.T.) ;
#28273 = ADVANCED_FACE('',(#3538),#796,.T.) ;
#28274 = ADVANCED_FACE('',(#3539),#797,.T.) ;
#28275 = ADVANCED_FACE('',(#3540),#798,.T.) ;
#28276 = ADVANCED_FACE('',(#3541),#799,.T.) ;
#28277 = ADVANCED_FACE('',(#3542),#800,.T.) ;
#28278 = ADVANCED_FACE('',(#3543),#801,.T.) ;
#28279 = ADVANCED_FACE('',(#3544),#802,.T.) ;
#28280 = ADVANCED_FACE('',(#3545),#803,.T.) ;
#28281 = ADVANCED_FACE('',(#3546),#804,.T.) ;
#28282 = ADVANCED_FACE('',(#3547),#805,.T.) ;
#28283 = ADVANCED_FACE('',(#3548),#806,.T.) ;
#28284 = ADVANCED_FACE('',(#3549),#807,.T.) ;
#28285 = ADVANCED_FACE('',(#3550),#808,.T.) ;
#28286 = ADVANCED_FACE('',(#3551),#809,.T.) ;
#28287 = ADVANCED_FACE('',(#3552),#810,.T.) ;
#28288 = ADVANCED_FACE('',(#3553),#811,.T.) ;
#28289 = ADVANCED_FACE('',(#3554),#812,.T.) ;
#28290 = ADVANCED_FACE('',(#3555),#813,.T.) ;
#28291 = ADVANCED_FACE('',(#3556),#814,.T.) ;
#28292 = ADVANCED_FACE('',(#3557),#815,.T.) ;
#28293 = ADVANCED_FACE('',(#3558),#816,.T.) ;
#28294 = ADVANCED_FACE('',(#3559),#817,.T.) ;
#28295 = ADVANCED_FACE('',(#3560),#818,.T.) ;
#28296 = ADVANCED_FACE('',(#3561),#819,.T.) ;
#28297 = ADVANCED_FACE('',(#3562),#820,.T.) ;
#28298 = ADVANCED_FACE('',(#3563),#821,.T.) ;
#28299 = ADVANCED_FACE('',(#3564),#822,.T.) ;
#28300 = ADVANCED_FACE('',(#3565),#823,.T.) ;
#28301 = ADVANCED_FACE('',(#3566),#824,.T.) ;
#28302 = ADVANCED_FACE('',(#3567),#825,.T.) ;
#28303 = ADVANCED_FACE('',(#3568),#826,.T.) ;
#28304 = ADVANCED_FACE('',(#3569),#827,.T.) ;
#28305 = ADVANCED_FACE('',(#3570),#828,.T.) ;
#28306 = ADVANCED_FACE('',(#3571),#829,.T.) ;
#28307 = ADVANCED_FACE('',(#3572),#830,.T.) ;
#28308 = ADVANCED_FACE('',(#3573),#831,.T.) ;
#28309 = ADVANCED_FACE('',(#3574),#832,.T.) ;
#28310 = ADVANCED_FACE('',(#3575),#833,.T.) ;
#28311 = ADVANCED_FACE('',(#3576),#834,.T.) ;
#28312 = ADVANCED_FACE('',(#3577),#835,.T.) ;
#28313 = ADVANCED_FACE('',(#3578),#836,.T.) ;
#28314 = ADVANCED_FACE('',(#3579),#837,.T.) ;
#28315 = ADVANCED_FACE('',(#3580),#838,.T.) ;
#28316 = ADVANCED_FACE('',(#3581),#839,.T.) ;
#28317 = ADVANCED_FACE('',(#3582),#840,.T.) ;
#28318 = ADVANCED_FACE('',(#3583),#841,.T.) ;
#28319 = ADVANCED_FACE('',(#3584),#842,.T.) ;
#28320 = ADVANCED_FACE('',(#3585),#843,.T.) ;
#28321 = ADVANCED_FACE('',(#3586),#844,.T.) ;
#28322 = ADVANCED_FACE('',(#3587),#845,.T.) ;
#28323 = ADVANCED_FACE('',(#3588),#846,.T.) ;
#28324 = ADVANCED_FACE('',(#3589),#847,.T.) ;
#28325 = ADVANCED_FACE('',(#3590),#848,.T.) ;
#28326 = ADVANCED_FACE('',(#3591),#849,.T.) ;
#28327 = ADVANCED_FACE('',(#3592),#850,.T.) ;
#28328 = ADVANCED_FACE('',(#3593),#851,.T.) ;
#28329 = ADVANCED_FACE('',(#3594),#852,.T.) ;
#28330 = ADVANCED_FACE('',(#3595),#853,.T.) ;
#28331 = ADVANCED_FACE('',(#3596),#854,.T.) ;
#28332 = ADVANCED_FACE('',(#3597),#855,.T.) ;
#28333 = ADVANCED_FACE('',(#3598),#856,.T.) ;
#28334 = ADVANCED_FACE('',(#3599),#857,.T.) ;
#28335 = ADVANCED_FACE('',(#3600),#858,.T.) ;
#28336 = ADVANCED_FACE('',(#3601),#859,.T.) ;
#28337 = ADVANCED_FACE('',(#3602),#860,.T.) ;
#28338 = ADVANCED_FACE('',(#3603),#861,.T.) ;
#28339 = ADVANCED_FACE('',(#3604),#862,.T.) ;
#28340 = ADVANCED_FACE('',(#3605),#863,.T.) ;
#28341 = ADVANCED_FACE('',(#3606),#864,.T.) ;
#28342 = ADVANCED_FACE('',(#3607),#865,.T.) ;
#28343 = ADVANCED_FACE('',(#3608),#866,.T.) ;
#28344 = ADVANCED_FACE('',(#3609),#867,.T.) ;
#28345 = ADVANCED_FACE('',(#3610),#868,.T.) ;
#28346 = ADVANCED_FACE('',(#3611),#869,.T.) ;
#28347 = ADVANCED_FACE('',(#3612),#870,.T.) ;
#28348 = ADVANCED_FACE('',(#3613),#871,.T.) ;
#28349 = ADVANCED_FACE('',(#3614),#872,.T.) ;
#28350 = ADVANCED_FACE('',(#3615),#873,.T.) ;
#28351 = ADVANCED_FACE('',(#3616),#874,.T.) ;
#28352 = ADVANCED_FACE('',(#3617),#26902,.T.) ;
#28353 = ADVANCED_FACE('',(#3618),#26903,.T.) ;
#28354 = ADVANCED_FACE('',(#3619),#26904,.T.) ;
#28355 = ADVANCED_FACE('',(#3620),#26905,.T.) ;
#28356 = ADVANCED_FACE('',(#3621),#26906,.T.) ;
#28357 = ADVANCED_FACE('',(#3622),#26907,.T.) ;
#28358 = ADVANCED_FACE('',(#3623),#26908,.T.) ;
#28359 = ADVANCED_FACE('',(#3624),#26909,.T.) ;
#28360 = ADVANCED_FACE('',(#3625),#26910,.T.) ;
#28361 = ADVANCED_FACE('',(#3626),#26911,.T.) ;
#28362 = ADVANCED_FACE('',(#3627),#26912,.T.) ;
#28363 = ADVANCED_FACE('',(#3628),#26913,.T.) ;
#28364 = ADVANCED_FACE('',(#3629),#26914,.T.) ;
#28365 = ADVANCED_FACE('',(#3630),#26915,.T.) ;
#28366 = ADVANCED_FACE('',(#3631),#26916,.T.) ;
#28367 = ADVANCED_FACE('',(#3632),#26917,.T.) ;
#28368 = ADVANCED_FACE('',(#3633),#26918,.T.) ;
#28369 = ADVANCED_FACE('',(#3634),#26919,.T.) ;
#28370 = ADVANCED_FACE('',(#3635),#26920,.T.) ;
#28371 = ADVANCED_FACE('',(#3636),#26921,.T.) ;
#28372 = ADVANCED_FACE('',(#3637),#26922,.T.) ;
#28373 = ADVANCED_FACE('',(#3638),#26923,.T.) ;
#28374 = ADVANCED_FACE('',(#3639),#26924,.T.) ;
#28375 = ADVANCED_FACE('',(#3640),#26925,.T.) ;
#28376 = ADVANCED_FACE('',(#3641),#26926,.T.) ;
#28377 = ADVANCED_FACE('',(#3642),#26927,.T.) ;
#28378 = ADVANCED_FACE('',(#3643),#26928,.T.) ;
#28379 = ADVANCED_FACE('',(#3644),#26929,.T.) ;
#28380 = ADVANCED_FACE('',(#3645),#26930,.T.) ;
#28381 = ADVANCED_FACE('',(#3646),#26931,.T.) ;
#28382 = ADVANCED_FACE('',(#3647),#26932,.T.) ;
#28383 = ADVANCED_FACE('',(#3648),#26933,.T.) ;
#28384 = ADVANCED_FACE('',(#3649),#26934,.T.) ;
#28385 = ADVANCED_FACE('',(#3650),#26935,.T.) ;
#28386 = ADVANCED_FACE('',(#3651),#26936,.T.) ;
#28387 = ADVANCED_FACE('',(#3652),#26937,.T.) ;
#28388 = ADVANCED_FACE('',(#3653),#26938,.T.) ;
#28389 = ADVANCED_FACE('',(#3654),#26939,.T.) ;
#28390 = ADVANCED_FACE('',(#3655),#26940,.T.) ;
#28391 = ADVANCED_FACE('',(#3656),#26941,.T.) ;
#28392 = ADVANCED_FACE('',(#3657),#26942,.T.) ;
#28393 = ADVANCED_FACE('',(#3658),#26943,.T.) ;
#28394 = ADVANCED_FACE('',(#3659),#26944,.T.) ;
#28395 = ADVANCED_FACE('',(#3660),#26945,.T.) ;
#28396 = ADVANCED_FACE('',(#3661),#26946,.T.) ;
#28397 = ADVANCED_FACE('',(#3662),#26947,.T.) ;
#28398 = ADVANCED_FACE('',(#3663),#26948,.T.) ;
#28399 = ADVANCED_FACE('',(#3664),#26949,.T.) ;
#28400 = ADVANCED_FACE('',(#3665),#26950,.T.) ;
#28401 = ADVANCED_FACE('',(#3666),#26951,.T.) ;
#28402 = ADVANCED_FACE('',(#3667),#26952,.T.) ;
#28403 = ADVANCED_FACE('',(#3668),#26953,.T.) ;
#28404 = ADVANCED_FACE('',(#3669),#26954,.T.) ;
#28405 = ADVANCED_FACE('',(#3670),#26955,.T.) ;
#28406 = ADVANCED_FACE('',(#3671),#26956,.T.) ;
#28407 = ADVANCED_FACE('',(#3672),#26957,.T.) ;
#28408 = ADVANCED_FACE('',(#3673),#26958,.T.) ;
#28409 = ADVANCED_FACE('',(#3674),#26959,.T.) ;
#28410 = ADVANCED_FACE('',(#3675),#26960,.T.) ;
#28411 = ADVANCED_FACE('',(#3676),#26961,.T.) ;
#28412 = ADVANCED_FACE('',(#3677),#26962,.T.) ;
#28413 = ADVANCED_FACE('',(#3678),#26963,.T.) ;
#28414 = ADVANCED_FACE('',(#3679),#26964,.T.) ;
#28415 = ADVANCED_FACE('',(#3680),#26965,.T.) ;
#28416 = ADVANCED_FACE('',(#3681),#26966,.T.) ;
#28417 = ADVANCED_FACE('',(#3682),#26967,.T.) ;
#28418 = ADVANCED_FACE('',(#3683),#26968,.T.) ;
#28419 = ADVANCED_FACE('',(#3684),#26969,.T.) ;
#28420 = ADVANCED_FACE('',(#3685),#26970,.T.) ;
#28421 = ADVANCED_FACE('',(#3686),#26971,.T.) ;
#28422 = ADVANCED_FACE('',(#3687),#26972,.T.) ;
#28423 = ADVANCED_FACE('',(#3688),#26973,.T.) ;
#28424 = ADVANCED_FACE('',(#3689),#26974,.T.) ;
#28425 = ADVANCED_FACE('',(#3690),#26975,.T.) ;
#28426 = ADVANCED_FACE('',(#3691),#26976,.T.) ;
#28427 = ADVANCED_FACE('',(#3692),#26977,.T.) ;
#28428 = ADVANCED_FACE('',(#3693),#26978,.T.) ;
#28429 = ADVANCED_FACE('',(#3694),#26979,.T.) ;
#28430 = ADVANCED_FACE('',(#3695),#26980,.T.) ;
#28431 = ADVANCED_FACE('',(#3696),#26981,.T.) ;
#28432 = ADVANCED_FACE('',(#3697),#26982,.T.) ;
#28433 = ADVANCED_FACE('',(#3698),#26983,.T.) ;
#28434 = ADVANCED_FACE('',(#3699),#26984,.T.) ;
#28435 = ADVANCED_FACE('',(#3700),#26985,.T.) ;
#28436 = ADVANCED_FACE('',(#3701),#26986,.T.) ;
#28437 = ADVANCED_FACE('',(#3702),#26987,.T.) ;
#28438 = ADVANCED_FACE('',(#3703),#26988,.T.) ;
#28439 = ADVANCED_FACE('',(#3704),#26989,.T.) ;
#28440 = ADVANCED_FACE('',(#3705),#26990,.T.) ;
#28441 = ADVANCED_FACE('',(#3706),#26991,.T.) ;
#28442 = ADVANCED_FACE('',(#3707),#26992,.T.) ;
#28443 = ADVANCED_FACE('',(#3708),#26993,.T.) ;
#28444 = ADVANCED_FACE('',(#3709),#26994,.T.) ;
#28445 = ADVANCED_FACE('',(#3710),#26995,.T.) ;
#28446 = ADVANCED_FACE('',(#3711),#26996,.T.) ;
#28447 = ADVANCED_FACE('',(#3712),#26997,.T.) ;
#28448 = ADVANCED_FACE('',(#3713),#26998,.T.) ;
#28449 = ADVANCED_FACE('',(#3714),#26999,.T.) ;
#28450 = ADVANCED_FACE('',(#3715),#27000,.T.) ;
#28451 = ADVANCED_FACE('',(#3716),#27001,.T.) ;
#28452 = ADVANCED_FACE('',(#3717),#27002,.T.) ;
#28453 = ADVANCED_FACE('',(#3718),#27003,.T.) ;
#28454 = ADVANCED_FACE('',(#3719),#27004,.T.) ;
#28455 = ADVANCED_FACE('',(#3720),#27005,.T.) ;
#28456 = ADVANCED_FACE('',(#3721),#27006,.T.) ;
#28457 = ADVANCED_FACE('',(#3722),#27007,.T.) ;
#28458 = ADVANCED_FACE('',(#3723),#27008,.T.) ;
#28459 = ADVANCED_FACE('',(#3724),#27009,.T.) ;
#28460 = ADVANCED_FACE('',(#3725),#27010,.T.) ;
#28461 = ADVANCED_FACE('',(#3726),#27011,.T.) ;
#28462 = ADVANCED_FACE('',(#3727),#27012,.T.) ;
#28463 = ADVANCED_FACE('',(#3728),#27013,.T.) ;
#28464 = ADVANCED_FACE('',(#3729),#27014,.T.) ;
#28465 = ADVANCED_FACE('',(#3730),#27015,.T.) ;
#28466 = ADVANCED_FACE('',(#3731),#27016,.T.) ;
#28467 = ADVANCED_FACE('',(#3732),#27017,.T.) ;
#28468 = ADVANCED_FACE('',(#3733),#27018,.T.) ;
#28469 = ADVANCED_FACE('',(#3734),#27019,.T.) ;
#28470 = ADVANCED_FACE('',(#3735),#27020,.T.) ;
#28471 = ADVANCED_FACE('',(#3736),#27021,.T.) ;
#28472 = ADVANCED_FACE('',(#3737),#27022,.T.) ;
#28473 = ADVANCED_FACE('',(#3738),#27023,.T.) ;
#28474 = ADVANCED_FACE('',(#3739),#27024,.T.) ;
#28475 = ADVANCED_FACE('',(#3740),#27025,.T.) ;
#28476 = ADVANCED_FACE('',(#3741),#27026,.T.) ;
#28477 = ADVANCED_FACE('',(#3742),#27027,.T.) ;
#28478 = ADVANCED_FACE('',(#3743),#27028,.T.) ;
#28479 = ADVANCED_FACE('',(#3744),#27029,.T.) ;
#28480 = ADVANCED_FACE('',(#3745),#2252,.T.) ;
#28481 = ADVANCED_FACE('',(#3746),#27030,.T.) ;
#28482 = ADVANCED_FACE('',(#3747),#27031,.F.) ;
#28483 = ADVANCED_FACE('',(#3748,#1386),#2253,.T.) ;
#28484 = ADVANCED_FACE('',(#3749,#1387),#2254,.T.) ;
#28485 = ADVANCED_FACE('',(#3750),#27032,.T.) ;
#28486 = ADVANCED_FACE('',(#3751),#2255,.T.) ;
#28487 = ADVANCED_FACE('',(#3752),#875,.F.) ;
#28488 = ADVANCED_FACE('',(#3753),#876,.T.) ;
#28489 = ADVANCED_FACE('',(#3754),#27033,.F.) ;
#28490 = ADVANCED_FACE('',(#3755),#27034,.F.) ;
#28491 = ADVANCED_FACE('',(#3756,#1388),#2256,.T.) ;
#28492 = ADVANCED_FACE('',(#3757),#27035,.T.) ;
#28493 = ADVANCED_FACE('',(#3758),#27036,.T.) ;
#28494 = ADVANCED_FACE('',(#3759,#1389),#2257,.T.) ;
#28495 = ADVANCED_FACE('',(#3760),#27037,.T.) ;
#28496 = ADVANCED_FACE('',(#3761),#27038,.T.) ;
#28497 = ADVANCED_FACE('',(#3762),#27039,.F.) ;
#28498 = ADVANCED_FACE('',(#3763),#27040,.F.) ;
#28499 = ADVANCED_FACE('',(#3764),#877,.T.) ;
#28500 = ADVANCED_FACE('',(#3765),#878,.T.) ;
#28501 = ADVANCED_FACE('',(#3766),#879,.T.) ;
#28502 = ADVANCED_FACE('',(#3767),#27041,.T.) ;
#28503 = ADVANCED_FACE('',(#3768),#2258,.T.) ;
#28504 = ADVANCED_FACE('',(#3769),#2259,.F.) ;
#28505 = ADVANCED_FACE('',(#3770),#2260,.T.) ;
#28506 = ADVANCED_FACE('',(#3771),#2261,.F.) ;
#28507 = ADVANCED_FACE('',(#3772,#1390),#2262,.F.) ;
#28508 = ADVANCED_FACE('',(#3773),#2263,.F.) ;
#28509 = ADVANCED_FACE('',(#3774),#2264,.F.) ;
#28510 = ADVANCED_FACE('',(#3775),#2265,.F.) ;
#28511 = ADVANCED_FACE('',(#3776),#2266,.T.) ;
#28512 = ADVANCED_FACE('',(#3777),#2267,.T.) ;
#28513 = ADVANCED_FACE('',(#3778,#1391),#27042,.T.) ;
#28514 = ADVANCED_FACE('',(#3779),#2268,.T.) ;
#28515 = ADVANCED_FACE('',(#3780),#27043,.F.) ;
#28516 = ADVANCED_FACE('',(#3781),#27044,.F.) ;
#28517 = ADVANCED_FACE('',(#3782),#2269,.T.) ;
#28518 = ADVANCED_FACE('',(#3783,#1392),#27045,.T.) ;
#28519 = ADVANCED_FACE('',(#3784),#2270,.T.) ;
#28520 = ADVANCED_FACE('',(#3785),#2271,.T.) ;
#28521 = ADVANCED_FACE('',(#3786,#1393),#27046,.T.) ;
#28522 = ADVANCED_FACE('',(#3787,#1394),#2272,.T.) ;
#28523 = ADVANCED_FACE('',(#3788,#1395),#2273,.T.) ;
#28524 = ADVANCED_FACE('',(#3789),#27047,.T.) ;
#28525 = ADVANCED_FACE('',(#3790),#27048,.F.) ;
#28526 = ADVANCED_FACE('',(#3791),#27049,.F.) ;
#28527 = ADVANCED_FACE('',(#3792),#27050,.T.) ;
#28528 = ADVANCED_FACE('',(#3793,#1396),#2274,.T.) ;
#28529 = ADVANCED_FACE('',(#3794,#1397),#2275,.T.) ;
#28530 = ADVANCED_FACE('',(#3795),#27051,.F.) ;
#28531 = ADVANCED_FACE('',(#3796),#2276,.F.) ;
#28532 = ADVANCED_FACE('',(#3797),#2277,.T.) ;
#28533 = ADVANCED_FACE('',(#3798),#2278,.T.) ;
#28534 = ADVANCED_FACE('',(#3799),#2279,.F.) ;
#28535 = ADVANCED_FACE('',(#3800),#2280,.F.) ;
#28536 = ADVANCED_FACE('',(#3801),#2281,.F.) ;
#28537 = ADVANCED_FACE('',(#3802),#2282,.F.) ;
#28538 = ADVANCED_FACE('',(#3803),#2283,.T.) ;
#28539 = ADVANCED_FACE('',(#3804),#2284,.F.) ;
#28540 = ADVANCED_FACE('',(#3805),#2285,.F.) ;
#28541 = ADVANCED_FACE('',(#3806),#2286,.F.) ;
#28542 = ADVANCED_FACE('',(#3807),#2287,.F.) ;
#28543 = ADVANCED_FACE('',(#3808),#2288,.F.) ;
#28544 = ADVANCED_FACE('',(#3809),#2289,.F.) ;
#28545 = ADVANCED_FACE('',(#3810),#2290,.F.) ;
#28546 = ADVANCED_FACE('',(#3811),#2291,.T.) ;
#28547 = ADVANCED_FACE('',(#3812),#2292,.F.) ;
#28548 = ADVANCED_FACE('',(#3813),#2293,.F.) ;
#28549 = ADVANCED_FACE('',(#3814),#2294,.F.) ;
#28550 = ADVANCED_FACE('',(#3815,#1398),#2295,.T.) ;
#28551 = ADVANCED_FACE('',(#3816),#27052,.F.) ;
#28552 = ADVANCED_FACE('',(#3817),#27053,.T.) ;
#28553 = ADVANCED_FACE('',(#3818,#1399),#2296,.T.) ;
#28554 = ADVANCED_FACE('',(#3819),#27054,.T.) ;
#28555 = ADVANCED_FACE('',(#3820),#2297,.T.) ;
#28556 = ADVANCED_FACE('',(#3821),#2298,.F.) ;
#28557 = ADVANCED_FACE('',(#3822),#2299,.F.) ;
#28558 = ADVANCED_FACE('',(#3823),#2300,.T.) ;
#28559 = ADVANCED_FACE('',(#3824),#2301,.F.) ;
#28560 = ADVANCED_FACE('',(#3825),#2302,.F.) ;
#28561 = ADVANCED_FACE('',(#3826),#2303,.F.) ;
#28562 = ADVANCED_FACE('',(#3827),#2304,.F.) ;
#28563 = ADVANCED_FACE('',(#3828,#1400),#2305,.T.) ;
#28564 = ADVANCED_FACE('',(#3829),#27055,.F.) ;
#28565 = ADVANCED_FACE('',(#3830),#2306,.F.) ;
#28566 = ADVANCED_FACE('',(#3831),#2307,.F.) ;
#28567 = ADVANCED_FACE('',(#3832,#1401),#2308,.T.) ;
#28568 = ADVANCED_FACE('',(#3833),#2309,.F.) ;
#28569 = ADVANCED_FACE('',(#3834),#2310,.F.) ;
#28570 = ADVANCED_FACE('',(#3835),#2311,.F.) ;
#28571 = ADVANCED_FACE('',(#3836),#2312,.F.) ;
#28572 = ADVANCED_FACE('',(#3837,#1402),#2313,.T.) ;
#28573 = ADVANCED_FACE('',(#3838),#27056,.T.) ;
#28574 = ADVANCED_FACE('',(#3839),#2314,.T.) ;
#28575 = ADVANCED_FACE('',(#3840),#2315,.F.) ;
#28576 = ADVANCED_FACE('',(#3841),#2316,.F.) ;
#28577 = ADVANCED_FACE('',(#3842),#2317,.T.) ;
#28578 = ADVANCED_FACE('',(#3843),#2318,.F.) ;
#28579 = ADVANCED_FACE('',(#3844),#2319,.F.) ;
#28580 = ADVANCED_FACE('',(#3845),#2320,.F.) ;
#28581 = ADVANCED_FACE('',(#3846),#2321,.F.) ;
#28582 = ADVANCED_FACE('',(#3847,#1403),#2322,.T.) ;
#28583 = ADVANCED_FACE('',(#3848),#27057,.F.) ;
#28584 = ADVANCED_FACE('',(#3849),#2323,.F.) ;
#28585 = ADVANCED_FACE('',(#3850),#2324,.F.) ;
#28586 = ADVANCED_FACE('',(#3851,#1404),#2325,.T.) ;
#28587 = ADVANCED_FACE('',(#3852),#2326,.F.) ;
#28588 = ADVANCED_FACE('',(#3853),#2327,.F.) ;
#28589 = ADVANCED_FACE('',(#3854),#2328,.F.) ;
#28590 = ADVANCED_FACE('',(#3855),#2329,.F.) ;
#28591 = ADVANCED_FACE('',(#3856,#1405),#2330,.T.) ;
#28592 = ADVANCED_FACE('',(#3857,#1406),#2331,.T.) ;
#28593 = ADVANCED_FACE('',(#3858),#27058,.T.) ;
#28594 = ADVANCED_FACE('',(#3859),#2332,.T.) ;
#28595 = ADVANCED_FACE('',(#3860),#27059,.T.) ;
#28596 = ADVANCED_FACE('',(#3861),#2333,.T.) ;
#28597 = ADVANCED_FACE('',(#3862,#1407),#2334,.T.) ;
#28598 = ADVANCED_FACE('',(#3863),#27060,.T.) ;
#28599 = ADVANCED_FACE('',(#3864),#2335,.T.) ;
#28600 = ADVANCED_FACE('',(#3865),#27061,.T.) ;
#28601 = ADVANCED_FACE('',(#3866),#2336,.T.) ;
#28602 = ADVANCED_FACE('',(#3867),#27062,.T.) ;
#28603 = ADVANCED_FACE('',(#3868),#880,.T.) ;
#28604 = ADVANCED_FACE('',(#3869),#881,.T.) ;
#28605 = ADVANCED_FACE('',(#3870),#882,.T.) ;
#28606 = ADVANCED_FACE('',(#3871),#883,.T.) ;
#28607 = ADVANCED_FACE('',(#3872),#884,.T.) ;
#28608 = ADVANCED_FACE('',(#3873),#885,.T.) ;
#28609 = ADVANCED_FACE('',(#3874),#886,.T.) ;
#28610 = ADVANCED_FACE('',(#3875),#887,.T.) ;
#28611 = ADVANCED_FACE('',(#3876),#888,.T.) ;
#28612 = ADVANCED_FACE('',(#3877),#889,.T.) ;
#28613 = ADVANCED_FACE('',(#3878),#890,.T.) ;
#28614 = ADVANCED_FACE('',(#3879),#27063,.T.) ;
#28615 = ADVANCED_FACE('',(#3880),#27064,.T.) ;
#28616 = ADVANCED_FACE('',(#3881),#27065,.T.) ;
#28617 = ADVANCED_FACE('',(#3882),#27066,.T.) ;
#28618 = ADVANCED_FACE('',(#3883),#27067,.T.) ;
#28619 = ADVANCED_FACE('',(#3884),#27068,.T.) ;
#28620 = ADVANCED_FACE('',(#3885),#27069,.T.) ;
#28621 = ADVANCED_FACE('',(#3886),#27070,.T.) ;
#28622 = ADVANCED_FACE('',(#3887),#27071,.T.) ;
#28623 = ADVANCED_FACE('',(#3888),#27072,.T.) ;
#28624 = ADVANCED_FACE('',(#3889),#27073,.T.) ;
#28625 = ADVANCED_FACE('',(#3890),#2337,.T.) ;
#28626 = ADVANCED_FACE('',(#3891),#27074,.T.) ;
#28627 = ADVANCED_FACE('',(#3892),#2338,.T.) ;
#28628 = ADVANCED_FACE('',(#3893),#2339,.T.) ;
#28629 = CLOSED_SHELL('',(#27075,#27076,#27077,#27078,#27079,#27080,#27081,
#27082,#27083,#27084,#27085,#27086,#27087,#27088,#27089,#27090,#27091,#27092,
#27093,#27094,#27095,#27096,#27097,#27098,#27099,#27100,#27101,#27102,#27103,
#27104,#27105,#27106,#27107,#27108,#27109,#27110,#27111,#27112,#27113,#27114,
#27115,#27116,#27117,#27118,#27119,#27120,#27121,#27122,#27123,#27124,#27125,
#27126,#27127,#27128,#27129,#27130,#27131,#27132,#27133,#27134,#27135,#27136,
#27137,#27138,#27139,#27140)) ;
#28630 = CLOSED_SHELL('',(#27141,#27142,#27143,#27144,#27145,#27146,#27147,
#27148,#27149,#27150,#27151,#27152,#27153)) ;
#28631 = CLOSED_SHELL('',(#27154,#27155,#27156,#27157,#27158,#27159)) ;
#28632 = CLOSED_SHELL('',(#27160,#27161,#27162,#27163,#27164,#27165,#27166,
#27167,#27168,#27169,#27170,#27171,#27172,#27173,#27174,#27175,#27176,#27177,
#27178,#27179,#27180,#27181,#27182,#27183,#27184,#27185,#27186,#27187,#27188,
#27189,#27190,#27191,#27192,#27193,#27194,#27195,#27196,#27197,#27198,#27199,
#27200,#27201,#27202,#27203,#27204,#27205,#27206,#27207,#27208,#27209,#27210,
#27211,#27212,#27213,#27214,#27215,#27216,#27217,#27218,#27219,#27220,#27221,
#27222,#27223,#27224,#27225,#27226,#27227,#27228,#27229,#27230,#27231,#27232,
#27233,#27234,#27235,#27236,#27237,#27238,#27239,#27240,#27241,#27242,#27243,
#27244,#27245,#27246,#27247,#27248,#27249,#27250,#27251,#27252,#27253,#27254,
#27255,#27256,#27257,#27258,#27259,#27260,#27261,#27262,#27263,#27264,#27265,
#27266,#27267,#27268,#27269,#27270,#27271,#27272,#27273,#27274,#27275,#27276,
#27277,#27278,#27279,#27280,#27281,#27282,#27283,#27284,#27285,#27286,#27287,
#27288,#27289,#27290,#27291,#27292,#27293,#27294,#27295,#27296,#27297,#27298,
#27299,#27300,#27301,#27302,#27303,#27304,#27305,#27306,#27307,#27308,#27309,
#27310,#27311,#27312,#27313,#27314,#27315,#27316,#27317,#27318,#27319,#27320,
#27321,#27322,#27323,#27324,#27325,#27326,#27327,#27328,#27329,#27330,#27331,
#27332,#27333,#27334,#27335,#27336,#27337,#27338,#27339,#27340,#27341,#27342,
#27343,#27344,#27345,#27346,#27347,#27348,#27349,#27350,#27351,#27352,#27353,
#27354,#27355,#27356,#27357,#27358,#27359,#27360,#27361,#27362,#27363,#27364,
#27365,#27366,#27367,#27368,#27369,#27370,#27371,#27372,#27373,#27374,#27375,
#27376,#27377,#27378,#27379,#27380,#27381,#27382,#27383,#27384,#27385,#27386,
#27387,#27388,#27389,#27390,#27391,#27392,#27393,#27394,#27395,#27396,#27397,
#27398,#27399,#27400,#27401,#27402,#27403,#27404,#27405,#27406,#27407,#27408,
#27409,#27410,#27411,#27412,#27413,#27414,#27415,#27416,#27417,#27418,#27419,
#27420,#27421,#27422,#27423,#27424,#27425,#27426,#27427,#27428,#27429,#27430,
#27431,#27432,#27433,#27434,#27435,#27436,#27437,#27438,#27439,#27440,#27441,
#27442,#27443,#27444,#27445,#27446,#27447,#27448,#27449,#27450,#27451,#27452,
#27453)) ;
#28633 = CLOSED_SHELL('',(#27454,#27455,#27456,#27457,#27458,#27459,#27460,
#27461,#27462,#27463,#27464,#27465,#27466,#27467,#27468,#27469,#27470,#27471,
#27472,#27473,#27474,#27475,#27476,#27477,#27478,#27479,#27480,#27481,#27482,
#27483,#27484,#27485,#27486,#27487,#27488,#27489,#27490,#27491,#27492,#27493,
#27494,#27495,#27496,#27497,#27498,#27499,#27500,#27501,#27502,#27503,#27504,
#27505,#27506,#27507,#27508,#27509)) ;
#28634 = CLOSED_SHELL('',(#27510,#27511,#27512,#27513,#27514,#27515,#27516,
#27517,#27518,#27519,#27520,#27521,#27522,#27523,#27524,#27525,#27526,#27527,
#27528,#27529,#27530,#27531,#27532,#27533,#27534,#27535,#27536,#27537,#27538,
#27539,#27540,#27541,#27542,#27543,#27544,#27545,#27546,#27547,#27548,#27549,
#27550,#27551,#27552,#27553,#27554,#27555,#27556,#27557,#27558,#27559,#27560,
#27561,#27562,#27563,#27564,#27565,#27566,#27567,#27568,#27569,#27570,#27571,
#27572,#27573,#27574,#27575,#27576,#27577,#27578,#27579,#27580,#27581,#27582,
#27583,#27584,#27585,#27586,#27587,#27588,#27589,#27590,#27591,#27592,#27593,
#27594,#27595,#27596,#27597,#27598,#27599,#27600,#27601,#27602,#27603,#27604,
#27605,#27606,#27607,#27608,#27609,#27610,#27611,#27612,#27613,#27614,#27615,
#27616,#27617,#27618,#27619,#27620,#27621,#27622,#27623,#27624,#27625,#27626,
#27627,#27628,#27629,#27630,#27631,#27632,#27633,#27634,#27635,#27636,#27637)) ;
#28635 = CLOSED_SHELL('',(#27638,#27639,#27640,#27641,#27642,#27643)) ;
#28636 = CLOSED_SHELL('',(#27644,#27645,#27646,#27647,#27648,#27649)) ;
#28637 = CLOSED_SHELL('',(#27650,#27651,#27652,#27653)) ;
#28638 = CLOSED_SHELL('',(#27654,#27655,#27656,#27657,#27658)) ;
#28639 = CLOSED_SHELL('',(#27659,#27660,#27661,#27662,#27663)) ;
#28640 = CLOSED_SHELL('',(#27664,#27665,#27666,#27667,#27668)) ;
#28641 = CLOSED_SHELL('',(#27669,#27670,#27671,#27672,#27673)) ;
#28642 = CLOSED_SHELL('',(#27674,#27675,#27676,#27677,#27678)) ;
#28643 = CLOSED_SHELL('',(#27679,#27680,#27681,#27682,#27683)) ;
#28644 = CLOSED_SHELL('',(#27684,#27685,#27686,#27687)) ;
#28645 = CLOSED_SHELL('',(#27688,#27689,#27690,#27691)) ;
#28646 = CLOSED_SHELL('',(#27692,#27693,#27694,#27695)) ;
#28647 = CLOSED_SHELL('',(#27696,#27697,#27698,#27699)) ;
#28648 = CLOSED_SHELL('',(#27700,#27701,#27702,#27703)) ;
#28649 = CLOSED_SHELL('',(#27704,#27705,#27706,#27707,#27708,#27709)) ;
#28650 = CLOSED_SHELL('',(#27710,#27711,#27712,#27713,#27714,#27715)) ;
#28651 = CLOSED_SHELL('',(#27716,#27717,#27718,#27719,#27720,#27721,#27722,
#27723,#27724,#27725,#27726,#27727,#27728,#27729)) ;
#28652 = CLOSED_SHELL('',(#27730,#27731,#27732,#27733)) ;
#28653 = CLOSED_SHELL('',(#27734,#27735,#27736,#27737,#27738,#27739,#27740,
#27741)) ;
#28654 = CLOSED_SHELL('',(#27742,#27743,#27744,#27745,#27746,#27747)) ;
#28655 = CLOSED_SHELL('',(#27748,#27749,#27750,#27751,#27752,#27753)) ;
#28656 = CLOSED_SHELL('',(#27754,#27755,#27756,#27757,#27758,#27759)) ;
#28657 = CLOSED_SHELL('',(#27760,#27761,#27762,#27763,#27764,#27765,#27766,
#27767,#27768,#27769,#27770,#27771,#27772,#27773,#27774,#27775,#27776,#27777,
#27778,#27779,#27780,#27781,#27782,#27783,#27784,#27785,#27786,#27787,#27788,
#27789,#27790,#27791,#27792,#27793,#27794,#27795,#27796,#27797,#27798,#27799,
#27800,#27801,#27802,#27803,#27804,#27805,#27806,#27807,#27808,#27809,#27810,
#27811,#27812,#27813,#27814,#27815,#27816,#27817,#27818,#27819,#27820,#27821,
#27822,#27823,#27824,#27825)) ;
#28658 = CLOSED_SHELL('',(#27826,#27827,#27828,#27829,#27830,#27831,#27832,
#27833,#27834,#27835)) ;
#28659 = CLOSED_SHELL('',(#27836,#27837,#27838,#27839,#27840,#27841,#27842,
#27843,#27844,#27845,#27846,#27847,#27848,#27849,#27850,#27851,#27852,#27853,
#27854,#27855,#27856,#27857,#27858,#27859,#27860,#27861,#27862,#27863,#27864,
#27865,#27866,#27867,#27868,#27869,#27870,#27871,#27872,#27873,#27874,#27875,
#27876,#27877,#27878,#27879,#27880,#27881,#27882,#27883,#27884,#27885,#27886,
#27887,#27888,#27889,#27890,#27891,#27892,#27893,#27894)) ;
#28660 = CLOSED_SHELL('',(#27895,#27896,#27897,#27898)) ;
#28661 = CLOSED_SHELL('',(#27899,#27900,#27901,#27902,#27903,#27904,#27905,
#27906,#27907,#27908,#27909,#27910,#27911,#27912)) ;
#28662 = CLOSED_SHELL('',(#27913,#27914,#27915)) ;
#28663 = CLOSED_SHELL('',(#27916,#27917,#27918,#27919,#27920,#27921)) ;
#28664 = CLOSED_SHELL('',(#27922,#27923,#27924,#27925)) ;
#28665 = CLOSED_SHELL('',(#27926,#27927,#27928,#27929)) ;
#28666 = CLOSED_SHELL('',(#27930,#27931,#27932)) ;
#28667 = CLOSED_SHELL('',(#27933,#27934,#27935,#27936,#27937,#27938,#27939,
#27940,#27941,#27942,#27943,#27944,#27945,#27946,#27947,#27948,#27949,#27950,
#27951,#27952,#27953,#27954,#27955,#27956,#27957,#27958,#27959,#27960,#27961,
#27962,#27963,#27964,#27965,#27966,#27967,#27968,#27969,#27970,#27971,#27972,
#27973,#27974,#27975,#27976,#27977,#27978,#27979)) ;
#28668 = CLOSED_SHELL('',(#27980,#27981,#27982,#27983)) ;
#28669 = CLOSED_SHELL('',(#27984,#27985,#27986,#27987,#27988,#27989,#27990,
#27991,#27992,#27993,#27994,#27995,#27996,#27997,#27998,#27999,#28000,#28001,
#28002,#28003,#28004,#28005,#28006,#28007,#28008,#28009,#28010,#28011,#28012,
#28013,#28014,#28015,#28016,#28017,#28018,#28019,#28020)) ;
#28670 = CLOSED_SHELL('',(#28021,#28022,#28023,#28024,#28025,#28026,#28027,
#28028,#28029,#28030,#28031,#28032,#28033,#28034,#28035,#28036,#28037,#28038,
#28039,#28040,#28041,#28042,#28043,#28044)) ;
#28671 = CLOSED_SHELL('',(#28045,#28046,#28047,#28048,#28049,#28050,#28051,
#28052,#28053,#28054,#28055,#28056,#28057,#28058,#28059,#28060,#28061,#28062,
#28063,#28064,#28065,#28066,#28067,#28068,#28069,#28070,#28071,#28072,#28073,
#28074,#28075,#28076,#28077,#28078,#28079,#28080,#28081,#28082,#28083,#28084,
#28085,#28086)) ;
#28672 = CLOSED_SHELL('',(#28087,#28088,#28089,#28090,#28091,#28092,#28093,
#28094,#28095,#28096,#28097,#28098,#28099,#28100,#28101)) ;
#28673 = CLOSED_SHELL('',(#28102,#28103,#28104,#28105,#28106)) ;
#28674 = CLOSED_SHELL('',(#28107,#28108,#28109,#28110)) ;
#28675 = CLOSED_SHELL('',(#28111,#28112,#28113,#28114,#28115,#28116,#28117,
#28118,#28119,#28120,#28121,#28122)) ;
#28676 = CLOSED_SHELL('',(#28123,#28124,#28125,#28126,#28127,#28128,#28129,
#28130,#28131,#28132,#28133,#28134,#28135,#28136,#28137,#28138,#28139,#28140,
#28141,#28142,#28143,#28144,#28145,#28146)) ;
#28677 = CLOSED_SHELL('',(#28147,#28148,#28149)) ;
#28678 = CLOSED_SHELL('',(#28150,#28151,#28152,#28153,#28154)) ;
#28679 = CLOSED_SHELL('',(#28155)) ;
#28680 = CLOSED_SHELL('',(#28156)) ;
#28681 = CLOSED_SHELL('',(#28157)) ;
#28682 = CLOSED_SHELL('',(#28158,#28159,#28160)) ;
#28683 = CLOSED_SHELL('',(#28161,#28162,#28163,#28164,#28165,#28166,#28167,
#28168,#28169,#28170,#28171,#28172,#28173,#28174,#28175,#28176,#28177,#28178)) ;
#28684 = CLOSED_SHELL('',(#28179,#28180,#28181,#28182)) ;
#28685 = CLOSED_SHELL('',(#28183)) ;
#28686 = CLOSED_SHELL('',(#28184,#28185,#28186,#28187,#28188)) ;
#28687 = CLOSED_SHELL('',(#28189,#28190,#28191,#28192,#28193)) ;
#28688 = CLOSED_SHELL('',(#28194)) ;
#28689 = CLOSED_SHELL('',(#28195,#28196,#28197,#28198,#28199,#28200)) ;
#28690 = CLOSED_SHELL('',(#28201,#28202,#28203)) ;
#28691 = CLOSED_SHELL('',(#28204,#28205,#28206)) ;
#28692 = CLOSED_SHELL('',(#28207,#28208,#28209)) ;
#28693 = CLOSED_SHELL('',(#28210,#28211,#28212,#28213,#28214,#28215)) ;
#28694 = CLOSED_SHELL('',(#28216,#28217,#28218,#28219)) ;
#28695 = CLOSED_SHELL('',(#28220,#28221,#28222,#28223,#28224,#28225,#28226,
#28227,#28228,#28229,#28230,#28231,#28232,#28233,#28234,#28235,#28236,#28237,
#28238,#28239,#28240,#28241,#28242,#28243,#28244,#28245,#28246,#28247,#28248,
#28249,#28250,#28251,#28252,#28253,#28254,#28255,#28256,#28257,#28258,#28259,
#28260,#28261,#28262,#28263,#28264,#28265,#28266,#28267,#28268,#28269,#28270,
#28271,#28272,#28273,#28274,#28275,#28276,#28277,#28278,#28279,#28280,#28281,
#28282,#28283,#28284,#28285,#28286,#28287,#28288,#28289,#28290,#28291,#28292,
#28293,#28294,#28295,#28296,#28297,#28298,#28299,#28300,#28301,#28302,#28303,
#28304,#28305,#28306,#28307,#28308,#28309,#28310,#28311,#28312,#28313,#28314,
#28315,#28316,#28317,#28318,#28319,#28320,#28321,#28322,#28323,#28324,#28325,
#28326,#28327,#28328,#28329,#28330,#28331,#28332,#28333,#28334,#28335,#28336,
#28337,#28338,#28339,#28340,#28341,#28342,#28343,#28344,#28345,#28346,#28347,
#28348,#28349,#28350,#28351,#28352,#28353,#28354,#28355,#28356,#28357,#28358,
#28359,#28360,#28361,#28362,#28363,#28364,#28365,#28366,#28367,#28368,#28369,
#28370,#28371,#28372,#28373,#28374,#28375,#28376,#28377,#28378,#28379,#28380,
#28381,#28382,#28383,#28384,#28385,#28386,#28387,#28388,#28389,#28390,#28391,
#28392,#28393,#28394,#28395,#28396,#28397,#28398,#28399,#28400,#28401,#28402,
#28403,#28404,#28405,#28406,#28407,#28408,#28409,#28410,#28411,#28412,#28413,
#28414,#28415,#28416,#28417,#28418,#28419,#28420,#28421,#28422,#28423,#28424,
#28425,#28426,#28427,#28428,#28429,#28430,#28431,#28432,#28433,#28434,#28435,
#28436,#28437,#28438,#28439,#28440,#28441,#28442,#28443,#28444,#28445,#28446,
#28447,#28448,#28449,#28450,#28451,#28452,#28453,#28454,#28455,#28456,#28457,
#28458,#28459,#28460,#28461,#28462,#28463,#28464,#28465,#28466,#28467,#28468,
#28469,#28470,#28471,#28472,#28473,#28474,#28475,#28476,#28477,#28478,#28479,
#28480)) ;
#28696 = CLOSED_SHELL('',(#28481,#28482,#28483,#28484,#28485,#28486)) ;
#28697 = CLOSED_SHELL('',(#28487)) ;
#28698 = CLOSED_SHELL('',(#28488,#28489,#28490)) ;
#28699 = CLOSED_SHELL('',(#28491,#28492,#28493,#28494,#28495,#28496,#28497,
#28498,#28499,#28500,#28501)) ;
#28700 = CLOSED_SHELL('',(#28502,#28503,#28504,#28505,#28506,#28507,#28508,
#28509,#28510)) ;
#28701 = CLOSED_SHELL('',(#28511,#28512,#28513,#28514,#28515)) ;
#28702 = CLOSED_SHELL('',(#28516,#28517,#28518,#28519,#28520)) ;
#28703 = CLOSED_SHELL('',(#28521,#28522,#28523,#28524,#28525)) ;
#28704 = CLOSED_SHELL('',(#28526,#28527,#28528,#28529)) ;
#28705 = CLOSED_SHELL('',(#28530,#28531,#28532,#28533,#28534,#28535,#28536,
#28537)) ;
#28706 = CLOSED_SHELL('',(#28538,#28539,#28540,#28541,#28542,#28543)) ;
#28707 = CLOSED_SHELL('',(#28544,#28545,#28546,#28547,#28548,#28549,#28550,
#28551,#28552,#28553)) ;
#28708 = CLOSED_SHELL('',(#28554,#28555,#28556,#28557,#28558,#28559,#28560,
#28561,#28562,#28563)) ;
#28709 = CLOSED_SHELL('',(#28564,#28565,#28566,#28567,#28568,#28569,#28570,
#28571,#28572)) ;
#28710 = CLOSED_SHELL('',(#28573,#28574,#28575,#28576,#28577,#28578,#28579,
#28580,#28581,#28582)) ;
#28711 = CLOSED_SHELL('',(#28583,#28584,#28585,#28586,#28587,#28588,#28589,
#28590,#28591)) ;
#28712 = CLOSED_SHELL('',(#28592,#28593,#28594,#28595,#28596)) ;
#28713 = CLOSED_SHELL('',(#28597,#28598,#28599,#28600,#28601)) ;
#28714 = CLOSED_SHELL('',(#28602,#28603,#28604,#28605,#28606,#28607,#28608,
#28609,#28610,#28611,#28612,#28613,#28614,#28615,#28616,#28617,#28618,#28619,
#28620,#28621,#28622,#28623,#28624,#28625,#28626,#28627,#28628)) ;
#28715 = DERIVED_UNIT_ELEMENT(#28805,1.) ;
#28716 = DERIVED_UNIT_ELEMENT(#50442,-3.) ;
#28717 = DERIVED_UNIT_ELEMENT(#28805,1.) ;
#28718 = DERIVED_UNIT_ELEMENT(#50442,-3.) ;
#28719 = DERIVED_UNIT_ELEMENT(#28805,1.) ;
#28720 = DERIVED_UNIT_ELEMENT(#50442,-3.) ;
#28721 = DERIVED_UNIT_ELEMENT(#28805,1.) ;
#28722 = DERIVED_UNIT_ELEMENT(#50442,-3.) ;
#28723 = DERIVED_UNIT_ELEMENT(#28805,1.) ;
#28724 = DERIVED_UNIT_ELEMENT(#50442,-3.) ;
#28725 = DERIVED_UNIT_ELEMENT(#28805,1.) ;
#28726 = DERIVED_UNIT_ELEMENT(#50442,-3.) ;
#28727 = DERIVED_UNIT_ELEMENT(#28805,1.) ;
#28728 = DERIVED_UNIT_ELEMENT(#50442,-3.) ;
#28729 = DERIVED_UNIT_ELEMENT(#28805,1.) ;
#28730 = DERIVED_UNIT_ELEMENT(#50442,-3.) ;
#28731 = DERIVED_UNIT_ELEMENT(#28805,1.) ;
#28732 = DERIVED_UNIT_ELEMENT(#50442,-3.) ;
#28733 = DERIVED_UNIT_ELEMENT(#28805,1.) ;
#28734 = DERIVED_UNIT_ELEMENT(#50442,-3.) ;
#28735 = DERIVED_UNIT_ELEMENT(#28805,1.) ;
#28736 = DERIVED_UNIT_ELEMENT(#50442,-3.) ;
#28737 = DERIVED_UNIT_ELEMENT(#28805,1.) ;
#28738 = DERIVED_UNIT_ELEMENT(#50442,-3.) ;
#28739 = DERIVED_UNIT_ELEMENT(#28805,1.) ;
#28740 = DERIVED_UNIT_ELEMENT(#50442,-3.) ;
#28741 = DERIVED_UNIT_ELEMENT(#28805,1.) ;
#28742 = DERIVED_UNIT_ELEMENT(#50442,-3.) ;
#28743 = DERIVED_UNIT_ELEMENT(#28805,1.) ;
#28744 = DERIVED_UNIT_ELEMENT(#50442,-3.) ;
#28745 = DERIVED_UNIT_ELEMENT(#28805,1.) ;
#28746 = DERIVED_UNIT_ELEMENT(#50442,-3.) ;
#28747 = DERIVED_UNIT_ELEMENT(#28805,1.) ;
#28748 = DERIVED_UNIT_ELEMENT(#50442,-3.) ;
#28749 = DERIVED_UNIT_ELEMENT(#28805,1.) ;
#28750 = DERIVED_UNIT_ELEMENT(#50442,-3.) ;
#28751 = DERIVED_UNIT_ELEMENT(#28805,1.) ;
#28752 = DERIVED_UNIT_ELEMENT(#50442,-3.) ;
#28753 = DERIVED_UNIT_ELEMENT(#28805,1.) ;
#28754 = DERIVED_UNIT_ELEMENT(#50442,-3.) ;
#28755 = DERIVED_UNIT_ELEMENT(#28805,1.) ;
#28756 = DERIVED_UNIT_ELEMENT(#50442,-3.) ;
#28757 = DERIVED_UNIT_ELEMENT(#28805,1.) ;
#28758 = DERIVED_UNIT_ELEMENT(#50442,-3.) ;
#28759 = DERIVED_UNIT_ELEMENT(#28805,1.) ;
#28760 = DERIVED_UNIT_ELEMENT(#50442,-3.) ;
#28761 = DERIVED_UNIT_ELEMENT(#28805,1.) ;
#28762 = DERIVED_UNIT_ELEMENT(#50442,-3.) ;
#28763 = DERIVED_UNIT_ELEMENT(#28805,1.) ;
#28764 = DERIVED_UNIT_ELEMENT(#50442,-3.) ;
#28765 = DERIVED_UNIT_ELEMENT(#28805,1.) ;
#28766 = DERIVED_UNIT_ELEMENT(#50442,-3.) ;
#28767 = DERIVED_UNIT_ELEMENT(#28805,1.) ;
#28768 = DERIVED_UNIT_ELEMENT(#50442,-3.) ;
#28769 = DERIVED_UNIT_ELEMENT(#28805,1.) ;
#28770 = DERIVED_UNIT_ELEMENT(#50442,-3.) ;
#28771 = DERIVED_UNIT_ELEMENT(#28805,1.) ;
#28772 = DERIVED_UNIT_ELEMENT(#50442,-3.) ;
#28773 = DERIVED_UNIT_ELEMENT(#28805,1.) ;
#28774 = DERIVED_UNIT_ELEMENT(#50442,-3.) ;
#28775 = DERIVED_UNIT_ELEMENT(#28805,1.) ;
#28776 = DERIVED_UNIT_ELEMENT(#50442,-3.) ;
#28777 = DERIVED_UNIT_ELEMENT(#28805,1.) ;
#28778 = DERIVED_UNIT_ELEMENT(#50442,-3.) ;
#28779 = DERIVED_UNIT_ELEMENT(#28805,1.) ;
#28780 = DERIVED_UNIT_ELEMENT(#50442,-3.) ;
#28781 = DERIVED_UNIT_ELEMENT(#28805,1.) ;
#28782 = DERIVED_UNIT_ELEMENT(#50442,-3.) ;
#28783 = DERIVED_UNIT_ELEMENT(#28805,1.) ;
#28784 = DERIVED_UNIT_ELEMENT(#50442,-3.) ;
#28785 = DERIVED_UNIT_ELEMENT(#28805,1.) ;
#28786 = DERIVED_UNIT_ELEMENT(#50442,-3.) ;
#28787 = DERIVED_UNIT_ELEMENT(#28805,1.) ;
#28788 = DERIVED_UNIT_ELEMENT(#50442,-3.) ;
#28789 = DERIVED_UNIT_ELEMENT(#28805,1.) ;
#28790 = DERIVED_UNIT_ELEMENT(#50442,-3.) ;
#28791 = DERIVED_UNIT_ELEMENT(#28805,1.) ;
#28792 = DERIVED_UNIT_ELEMENT(#50442,-3.) ;
#28793 = DERIVED_UNIT_ELEMENT(#28805,1.) ;
#28794 = DERIVED_UNIT_ELEMENT(#50442,-3.) ;
#28795 = DERIVED_UNIT_ELEMENT(#28805,1.) ;
#28796 = DERIVED_UNIT_ELEMENT(#50442,-3.) ;
#28797 = DERIVED_UNIT_ELEMENT(#28805,1.) ;
#28798 = DERIVED_UNIT_ELEMENT(#50442,-3.) ;
#28799 = DERIVED_UNIT_ELEMENT(#28805,1.) ;
#28800 = DERIVED_UNIT_ELEMENT(#50442,-3.) ;
#28801 = DERIVED_UNIT_ELEMENT(#28805,1.) ;
#28802 = DERIVED_UNIT_ELEMENT(#50442,-3.) ;
#28803 = DERIVED_UNIT_ELEMENT(#28805,1.) ;
#28804 = DERIVED_UNIT_ELEMENT(#50442,-3.) ;
#28805 = (
MASS_UNIT()
NAMED_UNIT(*)
SI_UNIT(.KILO.,.GRAM.)
) ;
#28806 = DERIVED_UNIT((#28715,#28716)) ;
#28807 = DERIVED_UNIT((#28717,#28718)) ;
#28808 = DERIVED_UNIT((#28719,#28720)) ;
#28809 = DERIVED_UNIT((#28721,#28722)) ;
#28810 = DERIVED_UNIT((#28723,#28724)) ;
#28811 = DERIVED_UNIT((#28725,#28726)) ;
#28812 = DERIVED_UNIT((#28727,#28728)) ;
#28813 = DERIVED_UNIT((#28729,#28730)) ;
#28814 = DERIVED_UNIT((#28731,#28732)) ;
#28815 = DERIVED_UNIT((#28733,#28734)) ;
#28816 = DERIVED_UNIT((#28735,#28736)) ;
#28817 = DERIVED_UNIT((#28737,#28738)) ;
#28818 = DERIVED_UNIT((#28739,#28740)) ;
#28819 = DERIVED_UNIT((#28741,#28742)) ;
#28820 = DERIVED_UNIT((#28743,#28744)) ;
#28821 = DERIVED_UNIT((#28745,#28746)) ;
#28822 = DERIVED_UNIT((#28747,#28748)) ;
#28823 = DERIVED_UNIT((#28749,#28750)) ;
#28824 = DERIVED_UNIT((#28751,#28752)) ;
#28825 = DERIVED_UNIT((#28753,#28754)) ;
#28826 = DERIVED_UNIT((#28755,#28756)) ;
#28827 = DERIVED_UNIT((#28757,#28758)) ;
#28828 = DERIVED_UNIT((#28759,#28760)) ;
#28829 = DERIVED_UNIT((#28761,#28762)) ;
#28830 = DERIVED_UNIT((#28763,#28764)) ;
#28831 = DERIVED_UNIT((#28765,#28766)) ;
#28832 = DERIVED_UNIT((#28767,#28768)) ;
#28833 = DERIVED_UNIT((#28769,#28770)) ;
#28834 = DERIVED_UNIT((#28771,#28772)) ;
#28835 = DERIVED_UNIT((#28773,#28774)) ;
#28836 = DERIVED_UNIT((#28775,#28776)) ;
#28837 = DERIVED_UNIT((#28777,#28778)) ;
#28838 = DERIVED_UNIT((#28779,#28780)) ;
#28839 = DERIVED_UNIT((#28781,#28782)) ;
#28840 = DERIVED_UNIT((#28783,#28784)) ;
#28841 = DERIVED_UNIT((#28785,#28786)) ;
#28842 = DERIVED_UNIT((#28787,#28788)) ;
#28843 = DERIVED_UNIT((#28789,#28790)) ;
#28844 = DERIVED_UNIT((#28791,#28792)) ;
#28845 = DERIVED_UNIT((#28793,#28794)) ;
#28846 = DERIVED_UNIT((#28795,#28796)) ;
#28847 = DERIVED_UNIT((#28797,#28798)) ;
#28848 = DERIVED_UNIT((#28799,#28800)) ;
#28849 = DERIVED_UNIT((#28801,#28802)) ;
#28850 = DERIVED_UNIT((#28803,#28804)) ;
#28851 = MEASURE_REPRESENTATION_ITEM('density measure',
POSITIVE_RATIO_MEASURE(7850.),#28806) ;
#28852 = MEASURE_REPRESENTATION_ITEM('density measure',
POSITIVE_RATIO_MEASURE(7850.),#28807) ;
#28853 = MEASURE_REPRESENTATION_ITEM('density measure',
POSITIVE_RATIO_MEASURE(7850.),#28808) ;
#28854 = MEASURE_REPRESENTATION_ITEM('density measure',
POSITIVE_RATIO_MEASURE(7850.),#28809) ;
#28855 = MEASURE_REPRESENTATION_ITEM('density measure',
POSITIVE_RATIO_MEASURE(7850.),#28810) ;
#28856 = MEASURE_REPRESENTATION_ITEM('density measure',
POSITIVE_RATIO_MEASURE(7850.),#28811) ;
#28857 = MEASURE_REPRESENTATION_ITEM('density measure',
POSITIVE_RATIO_MEASURE(7850.),#28812) ;
#28858 = MEASURE_REPRESENTATION_ITEM('density measure',
POSITIVE_RATIO_MEASURE(7850.),#28813) ;
#28859 = MEASURE_REPRESENTATION_ITEM('density measure',
POSITIVE_RATIO_MEASURE(7850.),#28814) ;
#28860 = MEASURE_REPRESENTATION_ITEM('density measure',
POSITIVE_RATIO_MEASURE(7850.),#28815) ;
#28861 = MEASURE_REPRESENTATION_ITEM('density measure',
POSITIVE_RATIO_MEASURE(7850.),#28816) ;
#28862 = MEASURE_REPRESENTATION_ITEM('density measure',
POSITIVE_RATIO_MEASURE(7850.),#28817) ;
#28863 = MEASURE_REPRESENTATION_ITEM('density measure',
POSITIVE_RATIO_MEASURE(7850.),#28818) ;
#28864 = MEASURE_REPRESENTATION_ITEM('density measure',
POSITIVE_RATIO_MEASURE(7850.),#28819) ;
#28865 = MEASURE_REPRESENTATION_ITEM('density measure',
POSITIVE_RATIO_MEASURE(7850.),#28820) ;
#28866 = MEASURE_REPRESENTATION_ITEM('density measure',
POSITIVE_RATIO_MEASURE(7850.),#28821) ;
#28867 = MEASURE_REPRESENTATION_ITEM('density measure',
POSITIVE_RATIO_MEASURE(7850.),#28822) ;
#28868 = MEASURE_REPRESENTATION_ITEM('density measure',
POSITIVE_RATIO_MEASURE(7850.),#28823) ;
#28869 = MEASURE_REPRESENTATION_ITEM('density measure',
POSITIVE_RATIO_MEASURE(7850.),#28824) ;
#28870 = MEASURE_REPRESENTATION_ITEM('density measure',
POSITIVE_RATIO_MEASURE(7850.),#28825) ;
#28871 = MEASURE_REPRESENTATION_ITEM('density measure',
POSITIVE_RATIO_MEASURE(7850.),#28826) ;
#28872 = MEASURE_REPRESENTATION_ITEM('density measure',
POSITIVE_RATIO_MEASURE(7850.),#28827) ;
#28873 = MEASURE_REPRESENTATION_ITEM('density measure',
POSITIVE_RATIO_MEASURE(7850.),#28828) ;
#28874 = MEASURE_REPRESENTATION_ITEM('density measure',
POSITIVE_RATIO_MEASURE(7850.),#28829) ;
#28875 = MEASURE_REPRESENTATION_ITEM('density measure',
POSITIVE_RATIO_MEASURE(7850.),#28830) ;
#28876 = MEASURE_REPRESENTATION_ITEM('density measure',
POSITIVE_RATIO_MEASURE(7850.),#28831) ;
#28877 = MEASURE_REPRESENTATION_ITEM('density measure',
POSITIVE_RATIO_MEASURE(7850.),#28832) ;
#28878 = MEASURE_REPRESENTATION_ITEM('density measure',
POSITIVE_RATIO_MEASURE(7850.),#28833) ;
#28879 = MEASURE_REPRESENTATION_ITEM('density measure',
POSITIVE_RATIO_MEASURE(7850.),#28834) ;
#28880 = MEASURE_REPRESENTATION_ITEM('density measure',
POSITIVE_RATIO_MEASURE(7850.),#28835) ;
#28881 = MEASURE_REPRESENTATION_ITEM('density measure',
POSITIVE_RATIO_MEASURE(7850.),#28836) ;
#28882 = MEASURE_REPRESENTATION_ITEM('density measure',
POSITIVE_RATIO_MEASURE(7850.),#28837) ;
#28883 = MEASURE_REPRESENTATION_ITEM('density measure',
POSITIVE_RATIO_MEASURE(7850.),#28838) ;
#28884 = MEASURE_REPRESENTATION_ITEM('density measure',
POSITIVE_RATIO_MEASURE(7850.),#28839) ;
#28885 = MEASURE_REPRESENTATION_ITEM('density measure',
POSITIVE_RATIO_MEASURE(7850.),#28840) ;
#28886 = MEASURE_REPRESENTATION_ITEM('density measure',
POSITIVE_RATIO_MEASURE(7850.),#28841) ;
#28887 = MEASURE_REPRESENTATION_ITEM('density measure',
POSITIVE_RATIO_MEASURE(7850.),#28842) ;
#28888 = MEASURE_REPRESENTATION_ITEM('density measure',
POSITIVE_RATIO_MEASURE(7850.),#28843) ;
#28889 = MEASURE_REPRESENTATION_ITEM('density measure',
POSITIVE_RATIO_MEASURE(7850.),#28844) ;
#28890 = MEASURE_REPRESENTATION_ITEM('density measure',
POSITIVE_RATIO_MEASURE(7850.),#28845) ;
#28891 = MEASURE_REPRESENTATION_ITEM('density measure',
POSITIVE_RATIO_MEASURE(7850.),#28846) ;
#28892 = MEASURE_REPRESENTATION_ITEM('density measure',
POSITIVE_RATIO_MEASURE(7850.),#28847) ;
#28893 = MEASURE_REPRESENTATION_ITEM('density measure',
POSITIVE_RATIO_MEASURE(7850.),#28848) ;
#28894 = MEASURE_REPRESENTATION_ITEM('density measure',
POSITIVE_RATIO_MEASURE(7850.),#28849) ;
#28895 = MEASURE_REPRESENTATION_ITEM('density measure',
POSITIVE_RATIO_MEASURE(7850.),#28850) ;
#28896 = PROPERTY_DEFINITION_REPRESENTATION(#29121,#28986) ;
#28897 = PROPERTY_DEFINITION_REPRESENTATION(#29122,#28987) ;
#28898 = PROPERTY_DEFINITION_REPRESENTATION(#29123,#28988) ;
#28899 = PROPERTY_DEFINITION_REPRESENTATION(#29124,#28989) ;
#28900 = PROPERTY_DEFINITION_REPRESENTATION(#29125,#28990) ;
#28901 = PROPERTY_DEFINITION_REPRESENTATION(#29126,#28991) ;
#28902 = PROPERTY_DEFINITION_REPRESENTATION(#29127,#28992) ;
#28903 = PROPERTY_DEFINITION_REPRESENTATION(#29128,#28993) ;
#28904 = PROPERTY_DEFINITION_REPRESENTATION(#29129,#28994) ;
#28905 = PROPERTY_DEFINITION_REPRESENTATION(#29130,#28995) ;
#28906 = PROPERTY_DEFINITION_REPRESENTATION(#29131,#28996) ;
#28907 = PROPERTY_DEFINITION_REPRESENTATION(#29132,#28997) ;
#28908 = PROPERTY_DEFINITION_REPRESENTATION(#29133,#28998) ;
#28909 = PROPERTY_DEFINITION_REPRESENTATION(#29134,#28999) ;
#28910 = PROPERTY_DEFINITION_REPRESENTATION(#29135,#29000) ;
#28911 = PROPERTY_DEFINITION_REPRESENTATION(#29136,#29001) ;
#28912 = PROPERTY_DEFINITION_REPRESENTATION(#29137,#29002) ;
#28913 = PROPERTY_DEFINITION_REPRESENTATION(#29138,#29003) ;
#28914 = PROPERTY_DEFINITION_REPRESENTATION(#29139,#29004) ;
#28915 = PROPERTY_DEFINITION_REPRESENTATION(#29140,#29005) ;
#28916 = PROPERTY_DEFINITION_REPRESENTATION(#29141,#29006) ;
#28917 = PROPERTY_DEFINITION_REPRESENTATION(#29142,#29007) ;
#28918 = PROPERTY_DEFINITION_REPRESENTATION(#29143,#29008) ;
#28919 = PROPERTY_DEFINITION_REPRESENTATION(#29144,#29009) ;
#28920 = PROPERTY_DEFINITION_REPRESENTATION(#29145,#29010) ;
#28921 = PROPERTY_DEFINITION_REPRESENTATION(#29146,#29011) ;
#28922 = PROPERTY_DEFINITION_REPRESENTATION(#29147,#29012) ;
#28923 = PROPERTY_DEFINITION_REPRESENTATION(#29148,#29013) ;
#28924 = PROPERTY_DEFINITION_REPRESENTATION(#29149,#29014) ;
#28925 = PROPERTY_DEFINITION_REPRESENTATION(#29150,#29015) ;
#28926 = PROPERTY_DEFINITION_REPRESENTATION(#29151,#29016) ;
#28927 = PROPERTY_DEFINITION_REPRESENTATION(#29152,#29017) ;
#28928 = PROPERTY_DEFINITION_REPRESENTATION(#29153,#29018) ;
#28929 = PROPERTY_DEFINITION_REPRESENTATION(#29154,#29019) ;
#28930 = PROPERTY_DEFINITION_REPRESENTATION(#29155,#29020) ;
#28931 = PROPERTY_DEFINITION_REPRESENTATION(#29156,#29021) ;
#28932 = PROPERTY_DEFINITION_REPRESENTATION(#29157,#29022) ;
#28933 = PROPERTY_DEFINITION_REPRESENTATION(#29158,#29023) ;
#28934 = PROPERTY_DEFINITION_REPRESENTATION(#29159,#29024) ;
#28935 = PROPERTY_DEFINITION_REPRESENTATION(#29160,#29025) ;
#28936 = PROPERTY_DEFINITION_REPRESENTATION(#29161,#29026) ;
#28937 = PROPERTY_DEFINITION_REPRESENTATION(#29162,#29027) ;
#28938 = PROPERTY_DEFINITION_REPRESENTATION(#29163,#29028) ;
#28939 = PROPERTY_DEFINITION_REPRESENTATION(#29164,#29029) ;
#28940 = PROPERTY_DEFINITION_REPRESENTATION(#29165,#29030) ;
#28941 = PROPERTY_DEFINITION_REPRESENTATION(#29166,#29031) ;
#28942 = PROPERTY_DEFINITION_REPRESENTATION(#29167,#29032) ;
#28943 = PROPERTY_DEFINITION_REPRESENTATION(#29168,#29033) ;
#28944 = PROPERTY_DEFINITION_REPRESENTATION(#29169,#29034) ;
#28945 = PROPERTY_DEFINITION_REPRESENTATION(#29170,#29035) ;
#28946 = PROPERTY_DEFINITION_REPRESENTATION(#29171,#29036) ;
#28947 = PROPERTY_DEFINITION_REPRESENTATION(#29172,#29037) ;
#28948 = PROPERTY_DEFINITION_REPRESENTATION(#29173,#29038) ;
#28949 = PROPERTY_DEFINITION_REPRESENTATION(#29174,#29039) ;
#28950 = PROPERTY_DEFINITION_REPRESENTATION(#29175,#29040) ;
#28951 = PROPERTY_DEFINITION_REPRESENTATION(#29176,#29041) ;
#28952 = PROPERTY_DEFINITION_REPRESENTATION(#29177,#29042) ;
#28953 = PROPERTY_DEFINITION_REPRESENTATION(#29178,#29043) ;
#28954 = PROPERTY_DEFINITION_REPRESENTATION(#29179,#29044) ;
#28955 = PROPERTY_DEFINITION_REPRESENTATION(#29180,#29045) ;
#28956 = PROPERTY_DEFINITION_REPRESENTATION(#29181,#29046) ;
#28957 = PROPERTY_DEFINITION_REPRESENTATION(#29182,#29047) ;
#28958 = PROPERTY_DEFINITION_REPRESENTATION(#29183,#29048) ;
#28959 = PROPERTY_DEFINITION_REPRESENTATION(#29184,#29049) ;
#28960 = PROPERTY_DEFINITION_REPRESENTATION(#29185,#29050) ;
#28961 = PROPERTY_DEFINITION_REPRESENTATION(#29186,#29051) ;
#28962 = PROPERTY_DEFINITION_REPRESENTATION(#29187,#29052) ;
#28963 = PROPERTY_DEFINITION_REPRESENTATION(#29188,#29053) ;
#28964 = PROPERTY_DEFINITION_REPRESENTATION(#29189,#29054) ;
#28965 = PROPERTY_DEFINITION_REPRESENTATION(#29190,#29055) ;
#28966 = PROPERTY_DEFINITION_REPRESENTATION(#29191,#29056) ;
#28967 = PROPERTY_DEFINITION_REPRESENTATION(#29192,#29057) ;
#28968 = PROPERTY_DEFINITION_REPRESENTATION(#29193,#29058) ;
#28969 = PROPERTY_DEFINITION_REPRESENTATION(#29194,#29059) ;
#28970 = PROPERTY_DEFINITION_REPRESENTATION(#29195,#29060) ;
#28971 = PROPERTY_DEFINITION_REPRESENTATION(#29196,#29061) ;
#28972 = PROPERTY_DEFINITION_REPRESENTATION(#29197,#29062) ;
#28973 = PROPERTY_DEFINITION_REPRESENTATION(#29198,#29063) ;
#28974 = PROPERTY_DEFINITION_REPRESENTATION(#29199,#29064) ;
#28975 = PROPERTY_DEFINITION_REPRESENTATION(#29200,#29065) ;
#28976 = PROPERTY_DEFINITION_REPRESENTATION(#29201,#29066) ;
#28977 = PROPERTY_DEFINITION_REPRESENTATION(#29202,#29067) ;
#28978 = PROPERTY_DEFINITION_REPRESENTATION(#29203,#29068) ;
#28979 = PROPERTY_DEFINITION_REPRESENTATION(#29204,#29069) ;
#28980 = PROPERTY_DEFINITION_REPRESENTATION(#29205,#29070) ;
#28981 = PROPERTY_DEFINITION_REPRESENTATION(#29206,#29071) ;
#28982 = PROPERTY_DEFINITION_REPRESENTATION(#29207,#29072) ;
#28983 = PROPERTY_DEFINITION_REPRESENTATION(#29208,#29073) ;
#28984 = PROPERTY_DEFINITION_REPRESENTATION(#29209,#29074) ;
#28985 = PROPERTY_DEFINITION_REPRESENTATION(#29210,#29075) ;
#28986 = REPRESENTATION('material name',(#29076),#50390) ;
#28987 = REPRESENTATION('density',(#28851),#50390) ;
#28988 = REPRESENTATION('material name',(#29077),#50391) ;
#28989 = REPRESENTATION('density',(#28852),#50391) ;
#28990 = REPRESENTATION('material name',(#29078),#50392) ;
#28991 = REPRESENTATION('density',(#28853),#50392) ;
#28992 = REPRESENTATION('material name',(#29079),#50393) ;
#28993 = REPRESENTATION('density',(#28854),#50393) ;
#28994 = REPRESENTATION('material name',(#29080),#50394) ;
#28995 = REPRESENTATION('density',(#28855),#50394) ;
#28996 = REPRESENTATION('material name',(#29081),#50396) ;
#28997 = REPRESENTATION('density',(#28856),#50396) ;
#28998 = REPRESENTATION('material name',(#29082),#50397) ;
#28999 = REPRESENTATION('density',(#28857),#50397) ;
#29000 = REPRESENTATION('material name',(#29083),#50398) ;
#29001 = REPRESENTATION('density',(#28858),#50398) ;
#29002 = REPRESENTATION('material name',(#29084),#50399) ;
#29003 = REPRESENTATION('density',(#28859),#50399) ;
#29004 = REPRESENTATION('material name',(#29085),#50401) ;
#29005 = REPRESENTATION('density',(#28860),#50401) ;
#29006 = REPRESENTATION('material name',(#29086),#50402) ;
#29007 = REPRESENTATION('density',(#28861),#50402) ;
#29008 = REPRESENTATION('material name',(#29087),#50403) ;
#29009 = REPRESENTATION('density',(#28862),#50403) ;
#29010 = REPRESENTATION('material name',(#29088),#50404) ;
#29011 = REPRESENTATION('density',(#28863),#50404) ;
#29012 = REPRESENTATION('material name',(#29089),#50405) ;
#29013 = REPRESENTATION('density',(#28864),#50405) ;
#29014 = REPRESENTATION('material name',(#29090),#50406) ;
#29015 = REPRESENTATION('density',(#28865),#50406) ;
#29016 = REPRESENTATION('material name',(#29091),#50407) ;
#29017 = REPRESENTATION('density',(#28866),#50407) ;
#29018 = REPRESENTATION('material name',(#29092),#50408) ;
#29019 = REPRESENTATION('density',(#28867),#50408) ;
#29020 = REPRESENTATION('material name',(#29093),#50409) ;
#29021 = REPRESENTATION('density',(#28868),#50409) ;
#29022 = REPRESENTATION('material name',(#29094),#50410) ;
#29023 = REPRESENTATION('density',(#28869),#50410) ;
#29024 = REPRESENTATION('material name',(#29095),#50412) ;
#29025 = REPRESENTATION('density',(#28870),#50412) ;
#29026 = REPRESENTATION('material name',(#29096),#50413) ;
#29027 = REPRESENTATION('density',(#28871),#50413) ;
#29028 = REPRESENTATION('material name',(#29097),#50414) ;
#29029 = REPRESENTATION('density',(#28872),#50414) ;
#29030 = REPRESENTATION('material name',(#29098),#50415) ;
#29031 = REPRESENTATION('density',(#28873),#50415) ;
#29032 = REPRESENTATION('material name',(#29099),#50416) ;
#29033 = REPRESENTATION('density',(#28874),#50416) ;
#29034 = REPRESENTATION('material name',(#29100),#50417) ;
#29035 = REPRESENTATION('density',(#28875),#50417) ;
#29036 = REPRESENTATION('material name',(#29101),#50418) ;
#29037 = REPRESENTATION('density',(#28876),#50418) ;
#29038 = REPRESENTATION('material name',(#29102),#50419) ;
#29039 = REPRESENTATION('density',(#28877),#50419) ;
#29040 = REPRESENTATION('material name',(#29103),#50420) ;
#29041 = REPRESENTATION('density',(#28878),#50420) ;
#29042 = REPRESENTATION('material name',(#29104),#50421) ;
#29043 = REPRESENTATION('density',(#28879),#50421) ;
#29044 = REPRESENTATION('material name',(#29105),#50422) ;
#29045 = REPRESENTATION('density',(#28880),#50422) ;
#29046 = REPRESENTATION('material name',(#29106),#50423) ;
#29047 = REPRESENTATION('density',(#28881),#50423) ;
#29048 = REPRESENTATION('material name',(#29107),#50424) ;
#29049 = REPRESENTATION('density',(#28882),#50424) ;
#29050 = REPRESENTATION('material name',(#29108),#50425) ;
#29051 = REPRESENTATION('density',(#28883),#50425) ;
#29052 = REPRESENTATION('material name',(#29109),#50427) ;
#29053 = REPRESENTATION('density',(#28884),#50427) ;
#29054 = REPRESENTATION('material name',(#29110),#50428) ;
#29055 = REPRESENTATION('density',(#28885),#50428) ;
#29056 = REPRESENTATION('material name',(#29111),#50429) ;
#29057 = REPRESENTATION('density',(#28886),#50429) ;
#29058 = REPRESENTATION('material name',(#29112),#50430) ;
#29059 = REPRESENTATION('density',(#28887),#50430) ;
#29060 = REPRESENTATION('material name',(#29113),#50431) ;
#29061 = REPRESENTATION('density',(#28888),#50431) ;
#29062 = REPRESENTATION('material name',(#29114),#50433) ;
#29063 = REPRESENTATION('density',(#28889),#50433) ;
#29064 = REPRESENTATION('material name',(#29115),#50434) ;
#29065 = REPRESENTATION('density',(#28890),#50434) ;
#29066 = REPRESENTATION('material name',(#29116),#50435) ;
#29067 = REPRESENTATION('density',(#28891),#50435) ;
#29068 = REPRESENTATION('material name',(#29117),#50436) ;
#29069 = REPRESENTATION('density',(#28892),#50436) ;
#29070 = REPRESENTATION('material name',(#29118),#50437) ;
#29071 = REPRESENTATION('density',(#28893),#50437) ;
#29072 = REPRESENTATION('material name',(#29119),#50438) ;
#29073 = REPRESENTATION('density',(#28894),#50438) ;
#29074 = REPRESENTATION('material name',(#29120),#50439) ;
#29075 = REPRESENTATION('density',(#28895),#50439) ;
#29076 = DESCRIPTIVE_REPRESENTATION_ITEM('Steel','Steel') ;
#29077 = DESCRIPTIVE_REPRESENTATION_ITEM('Steel','Steel') ;
#29078 = DESCRIPTIVE_REPRESENTATION_ITEM('Steel','Steel') ;
#29079 = DESCRIPTIVE_REPRESENTATION_ITEM('Steel','Steel') ;
#29080 = DESCRIPTIVE_REPRESENTATION_ITEM('Steel','Steel') ;
#29081 = DESCRIPTIVE_REPRESENTATION_ITEM('Steel','Steel') ;
#29082 = DESCRIPTIVE_REPRESENTATION_ITEM('Steel','Steel') ;
#29083 = DESCRIPTIVE_REPRESENTATION_ITEM('Steel','Steel') ;
#29084 = DESCRIPTIVE_REPRESENTATION_ITEM('Steel','Steel') ;
#29085 = DESCRIPTIVE_REPRESENTATION_ITEM('Steel','Steel') ;
#29086 = DESCRIPTIVE_REPRESENTATION_ITEM('Steel','Steel') ;
#29087 = DESCRIPTIVE_REPRESENTATION_ITEM('Steel','Steel') ;
#29088 = DESCRIPTIVE_REPRESENTATION_ITEM('Steel','Steel') ;
#29089 = DESCRIPTIVE_REPRESENTATION_ITEM('Steel','Steel') ;
#29090 = DESCRIPTIVE_REPRESENTATION_ITEM('Steel','Steel') ;
#29091 = DESCRIPTIVE_REPRESENTATION_ITEM('Steel','Steel') ;
#29092 = DESCRIPTIVE_REPRESENTATION_ITEM('Steel','Steel') ;
#29093 = DESCRIPTIVE_REPRESENTATION_ITEM('Steel','Steel') ;
#29094 = DESCRIPTIVE_REPRESENTATION_ITEM('Steel','Steel') ;
#29095 = DESCRIPTIVE_REPRESENTATION_ITEM('Steel','Steel') ;
#29096 = DESCRIPTIVE_REPRESENTATION_ITEM('Steel','Steel') ;
#29097 = DESCRIPTIVE_REPRESENTATION_ITEM('Steel','Steel') ;
#29098 = DESCRIPTIVE_REPRESENTATION_ITEM('Steel','Steel') ;
#29099 = DESCRIPTIVE_REPRESENTATION_ITEM('Steel','Steel') ;
#29100 = DESCRIPTIVE_REPRESENTATION_ITEM('Steel','Steel') ;
#29101 = DESCRIPTIVE_REPRESENTATION_ITEM('Steel','Steel') ;
#29102 = DESCRIPTIVE_REPRESENTATION_ITEM('Steel','Steel') ;
#29103 = DESCRIPTIVE_REPRESENTATION_ITEM('Steel','Steel') ;
#29104 = DESCRIPTIVE_REPRESENTATION_ITEM('Steel','Steel') ;
#29105 = DESCRIPTIVE_REPRESENTATION_ITEM('Steel','Steel') ;
#29106 = DESCRIPTIVE_REPRESENTATION_ITEM('Steel','Steel') ;
#29107 = DESCRIPTIVE_REPRESENTATION_ITEM('Steel','Steel') ;
#29108 = DESCRIPTIVE_REPRESENTATION_ITEM('Steel','Steel') ;
#29109 = DESCRIPTIVE_REPRESENTATION_ITEM('Steel','Steel') ;
#29110 = DESCRIPTIVE_REPRESENTATION_ITEM('Steel','Steel') ;
#29111 = DESCRIPTIVE_REPRESENTATION_ITEM('Steel','Steel') ;
#29112 = DESCRIPTIVE_REPRESENTATION_ITEM('Steel','Steel') ;
#29113 = DESCRIPTIVE_REPRESENTATION_ITEM('Steel','Steel') ;
#29114 = DESCRIPTIVE_REPRESENTATION_ITEM('Steel','Steel') ;
#29115 = DESCRIPTIVE_REPRESENTATION_ITEM('Steel','Steel') ;
#29116 = DESCRIPTIVE_REPRESENTATION_ITEM('Steel','Steel') ;
#29117 = DESCRIPTIVE_REPRESENTATION_ITEM('Steel','Steel') ;
#29118 = DESCRIPTIVE_REPRESENTATION_ITEM('Steel','Steel') ;
#29119 = DESCRIPTIVE_REPRESENTATION_ITEM('Steel','Steel') ;
#29120 = DESCRIPTIVE_REPRESENTATION_ITEM('Steel','Steel') ;
#29121 = PROPERTY_DEFINITION('material property','material name',#50674) ;
#29122 = PROPERTY_DEFINITION('material property','density of part',#50674) ;
#29123 = PROPERTY_DEFINITION('material property','material name',#50675) ;
#29124 = PROPERTY_DEFINITION('material property','density of part',#50675) ;
#29125 = PROPERTY_DEFINITION('material property','material name',#50676) ;
#29126 = PROPERTY_DEFINITION('material property','density of part',#50676) ;
#29127 = PROPERTY_DEFINITION('material property','material name',#50677) ;
#29128 = PROPERTY_DEFINITION('material property','density of part',#50677) ;
#29129 = PROPERTY_DEFINITION('material property','material name',#50678) ;
#29130 = PROPERTY_DEFINITION('material property','density of part',#50678) ;
#29131 = PROPERTY_DEFINITION('material property','material name',#50680) ;
#29132 = PROPERTY_DEFINITION('material property','density of part',#50680) ;
#29133 = PROPERTY_DEFINITION('material property','material name',#50681) ;
#29134 = PROPERTY_DEFINITION('material property','density of part',#50681) ;
#29135 = PROPERTY_DEFINITION('material property','material name',#50682) ;
#29136 = PROPERTY_DEFINITION('material property','density of part',#50682) ;
#29137 = PROPERTY_DEFINITION('material property','material name',#50683) ;
#29138 = PROPERTY_DEFINITION('material property','density of part',#50683) ;
#29139 = PROPERTY_DEFINITION('material property','material name',#50685) ;
#29140 = PROPERTY_DEFINITION('material property','density of part',#50685) ;
#29141 = PROPERTY_DEFINITION('material property','material name',#50686) ;
#29142 = PROPERTY_DEFINITION('material property','density of part',#50686) ;
#29143 = PROPERTY_DEFINITION('material property','material name',#50687) ;
#29144 = PROPERTY_DEFINITION('material property','density of part',#50687) ;
#29145 = PROPERTY_DEFINITION('material property','material name',#50688) ;
#29146 = PROPERTY_DEFINITION('material property','density of part',#50688) ;
#29147 = PROPERTY_DEFINITION('material property','material name',#50689) ;
#29148 = PROPERTY_DEFINITION('material property','density of part',#50689) ;
#29149 = PROPERTY_DEFINITION('material property','material name',#50690) ;
#29150 = PROPERTY_DEFINITION('material property','density of part',#50690) ;
#29151 = PROPERTY_DEFINITION('material property','material name',#50691) ;
#29152 = PROPERTY_DEFINITION('material property','density of part',#50691) ;
#29153 = PROPERTY_DEFINITION('material property','material name',#50692) ;
#29154 = PROPERTY_DEFINITION('material property','density of part',#50692) ;
#29155 = PROPERTY_DEFINITION('material property','material name',#50693) ;
#29156 = PROPERTY_DEFINITION('material property','density of part',#50693) ;
#29157 = PROPERTY_DEFINITION('material property','material name',#50694) ;
#29158 = PROPERTY_DEFINITION('material property','density of part',#50694) ;
#29159 = PROPERTY_DEFINITION('material property','material name',#50696) ;
#29160 = PROPERTY_DEFINITION('material property','density of part',#50696) ;
#29161 = PROPERTY_DEFINITION('material property','material name',#50697) ;
#29162 = PROPERTY_DEFINITION('material property','density of part',#50697) ;
#29163 = PROPERTY_DEFINITION('material property','material name',#50698) ;
#29164 = PROPERTY_DEFINITION('material property','density of part',#50698) ;
#29165 = PROPERTY_DEFINITION('material property','material name',#50699) ;
#29166 = PROPERTY_DEFINITION('material property','density of part',#50699) ;
#29167 = PROPERTY_DEFINITION('material property','material name',#50700) ;
#29168 = PROPERTY_DEFINITION('material property','density of part',#50700) ;
#29169 = PROPERTY_DEFINITION('material property','material name',#50701) ;
#29170 = PROPERTY_DEFINITION('material property','density of part',#50701) ;
#29171 = PROPERTY_DEFINITION('material property','material name',#50702) ;
#29172 = PROPERTY_DEFINITION('material property','density of part',#50702) ;
#29173 = PROPERTY_DEFINITION('material property','material name',#50703) ;
#29174 = PROPERTY_DEFINITION('material property','density of part',#50703) ;
#29175 = PROPERTY_DEFINITION('material property','material name',#50704) ;
#29176 = PROPERTY_DEFINITION('material property','density of part',#50704) ;
#29177 = PROPERTY_DEFINITION('material property','material name',#50705) ;
#29178 = PROPERTY_DEFINITION('material property','density of part',#50705) ;
#29179 = PROPERTY_DEFINITION('material property','material name',#50706) ;
#29180 = PROPERTY_DEFINITION('material property','density of part',#50706) ;
#29181 = PROPERTY_DEFINITION('material property','material name',#50707) ;
#29182 = PROPERTY_DEFINITION('material property','density of part',#50707) ;
#29183 = PROPERTY_DEFINITION('material property','material name',#50708) ;
#29184 = PROPERTY_DEFINITION('material property','density of part',#50708) ;
#29185 = PROPERTY_DEFINITION('material property','material name',#50709) ;
#29186 = PROPERTY_DEFINITION('material property','density of part',#50709) ;
#29187 = PROPERTY_DEFINITION('material property','material name',#50711) ;
#29188 = PROPERTY_DEFINITION('material property','density of part',#50711) ;
#29189 = PROPERTY_DEFINITION('material property','material name',#50712) ;
#29190 = PROPERTY_DEFINITION('material property','density of part',#50712) ;
#29191 = PROPERTY_DEFINITION('material property','material name',#50713) ;
#29192 = PROPERTY_DEFINITION('material property','density of part',#50713) ;
#29193 = PROPERTY_DEFINITION('material property','material name',#50714) ;
#29194 = PROPERTY_DEFINITION('material property','density of part',#50714) ;
#29195 = PROPERTY_DEFINITION('material property','material name',#50715) ;
#29196 = PROPERTY_DEFINITION('material property','density of part',#50715) ;
#29197 = PROPERTY_DEFINITION('material property','material name',#50717) ;
#29198 = PROPERTY_DEFINITION('material property','density of part',#50717) ;
#29199 = PROPERTY_DEFINITION('material property','material name',#50718) ;
#29200 = PROPERTY_DEFINITION('material property','density of part',#50718) ;
#29201 = PROPERTY_DEFINITION('material property','material name',#50719) ;
#29202 = PROPERTY_DEFINITION('material property','density of part',#50719) ;
#29203 = PROPERTY_DEFINITION('material property','material name',#50720) ;
#29204 = PROPERTY_DEFINITION('material property','density of part',#50720) ;
#29205 = PROPERTY_DEFINITION('material property','material name',#50721) ;
#29206 = PROPERTY_DEFINITION('material property','density of part',#50721) ;
#29207 = PROPERTY_DEFINITION('material property','material name',#50722) ;
#29208 = PROPERTY_DEFINITION('material property','density of part',#50722) ;
#29209 = PROPERTY_DEFINITION('material property','material name',#50723) ;
#29210 = PROPERTY_DEFINITION('material property','density of part',#50723) ;
#29211 = AXIS2_PLACEMENT_3D('',#41223,#32391,#32392) ;
#29212 = AXIS2_PLACEMENT_3D('',#41224,#32393,#32394) ;
#29213 = AXIS2_PLACEMENT_3D('',#41225,#32395,#32396) ;
#29214 = AXIS2_PLACEMENT_3D('',#41226,#32397,#32398) ;
#29215 = AXIS2_PLACEMENT_3D('',#41228,#32399,#32400) ;
#29216 = AXIS2_PLACEMENT_3D('',#41231,#32402,#32403) ;
#29217 = AXIS2_PLACEMENT_3D('',#41232,#32404,#32405) ;
#29218 = AXIS2_PLACEMENT_3D('',#41249,#32414,#32415) ;
#29219 = AXIS2_PLACEMENT_3D('',#41255,#32419,#32420) ;
#29220 = AXIS2_PLACEMENT_3D('',#41261,#32424,#32425) ;
#29221 = AXIS2_PLACEMENT_3D('',#41265,#32428,#32429) ;
#29222 = AXIS2_PLACEMENT_3D('',#41267,#32430,#32431) ;
#29223 = AXIS2_PLACEMENT_3D('',#41269,#32433,#32434) ;
#29224 = AXIS2_PLACEMENT_3D('',#41273,#32437,#32438) ;
#29225 = AXIS2_PLACEMENT_3D('',#41278,#32442,#32443) ;
#29226 = AXIS2_PLACEMENT_3D('',#41279,#32444,#32445) ;
#29227 = AXIS2_PLACEMENT_3D('',#41281,#32446,#32447) ;
#29228 = AXIS2_PLACEMENT_3D('',#41285,#32449,#32450) ;
#29229 = AXIS2_PLACEMENT_3D('',#41289,#32452,#32453) ;
#29230 = AXIS2_PLACEMENT_3D('',#41292,#32455,#32456) ;
#29231 = AXIS2_PLACEMENT_3D('',#41293,#32457,#32458) ;
#29232 = AXIS2_PLACEMENT_3D('',#41294,#32459,#32460) ;
#29233 = AXIS2_PLACEMENT_3D('',#41296,#32461,#32462) ;
#29234 = AXIS2_PLACEMENT_3D('',#41299,#32464,#32465) ;
#29235 = AXIS2_PLACEMENT_3D('',#41300,#32466,#32467) ;
#29236 = AXIS2_PLACEMENT_3D('',#41314,#32475,#32476) ;
#29237 = AXIS2_PLACEMENT_3D('',#41320,#32480,#32481) ;
#29238 = AXIS2_PLACEMENT_3D('',#41326,#32485,#32486) ;
#29239 = AXIS2_PLACEMENT_3D('',#41330,#32489,#32490) ;
#29240 = AXIS2_PLACEMENT_3D('',#41332,#32492,#32493) ;
#29241 = AXIS2_PLACEMENT_3D('',#41336,#32496,#32497) ;
#29242 = AXIS2_PLACEMENT_3D('',#41339,#32500,#32501) ;
#29243 = AXIS2_PLACEMENT_3D('',#41340,#32502,#32503) ;
#29244 = AXIS2_PLACEMENT_3D('',#41343,#32504,#32505) ;
#29245 = AXIS2_PLACEMENT_3D('',#41349,#32509,#32510) ;
#29246 = AXIS2_PLACEMENT_3D('',#41357,#32513,#32514) ;
#29247 = AXIS2_PLACEMENT_3D('',#41365,#32517,#32518) ;
#29248 = AXIS2_PLACEMENT_3D('',#41376,#32522,#32523) ;
#29249 = AXIS2_PLACEMENT_3D('',#41377,#32524,#32525) ;
#29250 = AXIS2_PLACEMENT_3D('',#41379,#32527,#32528) ;
#29251 = AXIS2_PLACEMENT_3D('',#41381,#32529,#32530) ;
#29252 = AXIS2_PLACEMENT_3D('',#41385,#32533,#32534) ;
#29253 = AXIS2_PLACEMENT_3D('',#41387,#32535,#32536) ;
#29254 = AXIS2_PLACEMENT_3D('',#41391,#32539,#32540) ;
#29255 = AXIS2_PLACEMENT_3D('',#41396,#32542,#32543) ;
#29256 = AXIS2_PLACEMENT_3D('',#41397,#32544,#32545) ;
#29257 = AXIS2_PLACEMENT_3D('',#41398,#32546,#32547) ;
#29258 = AXIS2_PLACEMENT_3D('',#41401,#32548,#32549) ;
#29259 = AXIS2_PLACEMENT_3D('',#41407,#32553,#32554) ;
#29260 = AXIS2_PLACEMENT_3D('',#41415,#32557,#32558) ;
#29261 = AXIS2_PLACEMENT_3D('',#41423,#32561,#32562) ;
#29262 = AXIS2_PLACEMENT_3D('',#41434,#32566,#32567) ;
#29263 = AXIS2_PLACEMENT_3D('',#41435,#32568,#32569) ;
#29264 = AXIS2_PLACEMENT_3D('',#41437,#32571,#32572) ;
#29265 = AXIS2_PLACEMENT_3D('',#41439,#32573,#32574) ;
#29266 = AXIS2_PLACEMENT_3D('',#41443,#32577,#32578) ;
#29267 = AXIS2_PLACEMENT_3D('',#41445,#32579,#32580) ;
#29268 = AXIS2_PLACEMENT_3D('',#41449,#32583,#32584) ;
#29269 = AXIS2_PLACEMENT_3D('',#41454,#32586,#32587) ;
#29270 = AXIS2_PLACEMENT_3D('',#41455,#32588,#32589) ;
#29271 = AXIS2_PLACEMENT_3D('',#41456,#32590,#32591) ;
#29272 = AXIS2_PLACEMENT_3D('',#41459,#32592,#32593) ;
#29273 = AXIS2_PLACEMENT_3D('',#41465,#32597,#32598) ;
#29274 = AXIS2_PLACEMENT_3D('',#41473,#32601,#32602) ;
#29275 = AXIS2_PLACEMENT_3D('',#41481,#32605,#32606) ;
#29276 = AXIS2_PLACEMENT_3D('',#41492,#32610,#32611) ;
#29277 = AXIS2_PLACEMENT_3D('',#41493,#32612,#32613) ;
#29278 = AXIS2_PLACEMENT_3D('',#41495,#32615,#32616) ;
#29279 = AXIS2_PLACEMENT_3D('',#41497,#32617,#32618) ;
#29280 = AXIS2_PLACEMENT_3D('',#41501,#32621,#32622) ;
#29281 = AXIS2_PLACEMENT_3D('',#41503,#32623,#32624) ;
#29282 = AXIS2_PLACEMENT_3D('',#41507,#32627,#32628) ;
#29283 = AXIS2_PLACEMENT_3D('',#41512,#32630,#32631) ;
#29284 = AXIS2_PLACEMENT_3D('',#41513,#32632,#32633) ;
#29285 = AXIS2_PLACEMENT_3D('',#41514,#32634,#32635) ;
#29286 = AXIS2_PLACEMENT_3D('',#41517,#32636,#32637) ;
#29287 = AXIS2_PLACEMENT_3D('',#41523,#32641,#32642) ;
#29288 = AXIS2_PLACEMENT_3D('',#41531,#32645,#32646) ;
#29289 = AXIS2_PLACEMENT_3D('',#41539,#32649,#32650) ;
#29290 = AXIS2_PLACEMENT_3D('',#41550,#32654,#32655) ;
#29291 = AXIS2_PLACEMENT_3D('',#41551,#32656,#32657) ;
#29292 = AXIS2_PLACEMENT_3D('',#41553,#32659,#32660) ;
#29293 = AXIS2_PLACEMENT_3D('',#41555,#32661,#32662) ;
#29294 = AXIS2_PLACEMENT_3D('',#41559,#32665,#32666) ;
#29295 = AXIS2_PLACEMENT_3D('',#41561,#32667,#32668) ;
#29296 = AXIS2_PLACEMENT_3D('',#41565,#32671,#32672) ;
#29297 = AXIS2_PLACEMENT_3D('',#41570,#32674,#32675) ;
#29298 = AXIS2_PLACEMENT_3D('',#41571,#32676,#32677) ;
#29299 = AXIS2_PLACEMENT_3D('',#41572,#32678,#32679) ;
#29300 = AXIS2_PLACEMENT_3D('',#41574,#32680,#32681) ;
#29301 = AXIS2_PLACEMENT_3D('',#41577,#32683,#32684) ;
#29302 = AXIS2_PLACEMENT_3D('',#41578,#32685,#32686) ;
#29303 = AXIS2_PLACEMENT_3D('',#41580,#32687,#32688) ;
#29304 = AXIS2_PLACEMENT_3D('',#41583,#32690,#32691) ;
#29305 = AXIS2_PLACEMENT_3D('',#41584,#32692,#32693) ;
#29306 = AXIS2_PLACEMENT_3D('',#41585,#32694,#32695) ;
#29307 = AXIS2_PLACEMENT_3D('',#41586,#32696,#32697) ;
#29308 = AXIS2_PLACEMENT_3D('',#41588,#32698,#32699) ;
#29309 = AXIS2_PLACEMENT_3D('',#41590,#32701,#32702) ;
#29310 = AXIS2_PLACEMENT_3D('',#41593,#32704,#32705) ;
#29311 = AXIS2_PLACEMENT_3D('',#41594,#32706,#32707) ;
#29312 = AXIS2_PLACEMENT_3D('',#41595,#32708,#32709) ;
#29313 = AXIS2_PLACEMENT_3D('',#41596,#32710,#32711) ;
#29314 = AXIS2_PLACEMENT_3D('',#41605,#32716,#32717) ;
#29315 = AXIS2_PLACEMENT_3D('',#41611,#32721,#32722) ;
#29316 = AXIS2_PLACEMENT_3D('',#41617,#32726,#32727) ;
#29317 = AXIS2_PLACEMENT_3D('',#41627,#32733,#32734) ;
#29318 = AXIS2_PLACEMENT_3D('',#41637,#32740,#32741) ;
#29319 = AXIS2_PLACEMENT_3D('',#41640,#32744,#32745) ;
#29320 = AXIS2_PLACEMENT_3D('',#41642,#32747,#32748) ;
#29321 = AXIS2_PLACEMENT_3D('',#41644,#32750,#32751) ;
#29322 = AXIS2_PLACEMENT_3D('',#41646,#32752,#32753) ;
#29323 = AXIS2_PLACEMENT_3D('',#41649,#32755,#32756) ;
#29324 = AXIS2_PLACEMENT_3D('',#41650,#32757,#32758) ;
#29325 = AXIS2_PLACEMENT_3D('',#41652,#32759,#32760) ;
#29326 = AXIS2_PLACEMENT_3D('',#41653,#32761,#32762) ;
#29327 = AXIS2_PLACEMENT_3D('',#41655,#32763,#32764) ;
#29328 = AXIS2_PLACEMENT_3D('',#41657,#32766,#32767) ;
#29329 = AXIS2_PLACEMENT_3D('',#41658,#32768,#32769) ;
#29330 = AXIS2_PLACEMENT_3D('',#41659,#32770,#32771) ;
#29331 = AXIS2_PLACEMENT_3D('',#41660,#32772,#32773) ;
#29332 = AXIS2_PLACEMENT_3D('',#41669,#32778,#32779) ;
#29333 = AXIS2_PLACEMENT_3D('',#41678,#32784,#32785) ;
#29334 = AXIS2_PLACEMENT_3D('',#41681,#32788,#32789) ;
#29335 = AXIS2_PLACEMENT_3D('',#41682,#32790,#32791) ;
#29336 = AXIS2_PLACEMENT_3D('',#41683,#32792,#32793) ;
#29337 = AXIS2_PLACEMENT_3D('',#41684,#32794,#32795) ;
#29338 = AXIS2_PLACEMENT_3D('',#41685,#32796,#32797) ;
#29339 = AXIS2_PLACEMENT_3D('',#41686,#32798,#32799) ;
#29340 = AXIS2_PLACEMENT_3D('',#41687,#32800,#32801) ;
#29341 = AXIS2_PLACEMENT_3D('',#41696,#32806,#32807) ;
#29342 = AXIS2_PLACEMENT_3D('',#41705,#32812,#32813) ;
#29343 = AXIS2_PLACEMENT_3D('',#41714,#32818,#32819) ;
#29344 = AXIS2_PLACEMENT_3D('',#41723,#32824,#32825) ;
#29345 = AXIS2_PLACEMENT_3D('',#41732,#32830,#32831) ;
#29346 = AXIS2_PLACEMENT_3D('',#41741,#32836,#32837) ;
#29347 = AXIS2_PLACEMENT_3D('',#41750,#32842,#32843) ;
#29348 = AXIS2_PLACEMENT_3D('',#41759,#32848,#32849) ;
#29349 = AXIS2_PLACEMENT_3D('',#41768,#32854,#32855) ;
#29350 = AXIS2_PLACEMENT_3D('',#41777,#32860,#32861) ;
#29351 = AXIS2_PLACEMENT_3D('',#41786,#32866,#32867) ;
#29352 = AXIS2_PLACEMENT_3D('',#41795,#32872,#32873) ;
#29353 = AXIS2_PLACEMENT_3D('',#41801,#32877,#32878) ;
#29354 = AXIS2_PLACEMENT_3D('',#41807,#32882,#32883) ;
#29355 = AXIS2_PLACEMENT_3D('',#41809,#32884,#32885) ;
#29356 = AXIS2_PLACEMENT_3D('',#41812,#32887,#32888) ;
#29357 = AXIS2_PLACEMENT_3D('',#41813,#32889,#32890) ;
#29358 = AXIS2_PLACEMENT_3D('',#41815,#32891,#32892) ;
#29359 = AXIS2_PLACEMENT_3D('',#41818,#32894,#32895) ;
#29360 = AXIS2_PLACEMENT_3D('',#41819,#32896,#32897) ;
#29361 = AXIS2_PLACEMENT_3D('',#41821,#32898,#32899) ;
#29362 = AXIS2_PLACEMENT_3D('',#41824,#32901,#32902) ;
#29363 = AXIS2_PLACEMENT_3D('',#41825,#32903,#32904) ;
#29364 = AXIS2_PLACEMENT_3D('',#41831,#32908,#32909) ;
#29365 = AXIS2_PLACEMENT_3D('',#41837,#32913,#32914) ;
#29366 = AXIS2_PLACEMENT_3D('',#41843,#32918,#32919) ;
#29367 = AXIS2_PLACEMENT_3D('',#41849,#32923,#32924) ;
#29368 = AXIS2_PLACEMENT_3D('',#41855,#32928,#32929) ;
#29369 = AXIS2_PLACEMENT_3D('',#41861,#32933,#32934) ;
#29370 = AXIS2_PLACEMENT_3D('',#41867,#32938,#32939) ;
#29371 = AXIS2_PLACEMENT_3D('',#41873,#32943,#32944) ;
#29372 = AXIS2_PLACEMENT_3D('',#41879,#32947,#32948) ;
#29373 = AXIS2_PLACEMENT_3D('',#41885,#32951,#32952) ;
#29374 = AXIS2_PLACEMENT_3D('',#41891,#32955,#32956) ;
#29375 = AXIS2_PLACEMENT_3D('',#41899,#32960,#32961) ;
#29376 = AXIS2_PLACEMENT_3D('',#41905,#32964,#32965) ;
#29377 = AXIS2_PLACEMENT_3D('',#41911,#32968,#32969) ;
#29378 = AXIS2_PLACEMENT_3D('',#41917,#32972,#32973) ;
#29379 = AXIS2_PLACEMENT_3D('',#41923,#32976,#32977) ;
#29380 = AXIS2_PLACEMENT_3D('',#41929,#32980,#32981) ;
#29381 = AXIS2_PLACEMENT_3D('',#41935,#32984,#32985) ;
#29382 = AXIS2_PLACEMENT_3D('',#41943,#32989,#32990) ;
#29383 = AXIS2_PLACEMENT_3D('',#41949,#32993,#32994) ;
#29384 = AXIS2_PLACEMENT_3D('',#41955,#32997,#32998) ;
#29385 = AXIS2_PLACEMENT_3D('',#41961,#33001,#33002) ;
#29386 = AXIS2_PLACEMENT_3D('',#41967,#33005,#33006) ;
#29387 = AXIS2_PLACEMENT_3D('',#41973,#33009,#33010) ;
#29388 = AXIS2_PLACEMENT_3D('',#41979,#33013,#33014) ;
#29389 = AXIS2_PLACEMENT_3D('',#41987,#33018,#33019) ;
#29390 = AXIS2_PLACEMENT_3D('',#41993,#33022,#33023) ;
#29391 = AXIS2_PLACEMENT_3D('',#41999,#33026,#33027) ;
#29392 = AXIS2_PLACEMENT_3D('',#42004,#33030,#33031) ;
#29393 = AXIS2_PLACEMENT_3D('',#42006,#33032,#33033) ;
#29394 = AXIS2_PLACEMENT_3D('',#42012,#33036,#33037) ;
#29395 = AXIS2_PLACEMENT_3D('',#42018,#33040,#33041) ;
#29396 = AXIS2_PLACEMENT_3D('',#42026,#33045,#33046) ;
#29397 = AXIS2_PLACEMENT_3D('',#42032,#33049,#33050) ;
#29398 = AXIS2_PLACEMENT_3D('',#42038,#33054,#33055) ;
#29399 = AXIS2_PLACEMENT_3D('',#42041,#33057,#33058) ;
#29400 = AXIS2_PLACEMENT_3D('',#42043,#33060,#33061) ;
#29401 = AXIS2_PLACEMENT_3D('',#42060,#33072,#33073) ;
#29402 = AXIS2_PLACEMENT_3D('',#42065,#33075,#33076) ;
#29403 = AXIS2_PLACEMENT_3D('',#42105,#33096,#33097) ;
#29404 = AXIS2_PLACEMENT_3D('',#42113,#33101,#33102) ;
#29405 = AXIS2_PLACEMENT_3D('',#42123,#33107,#33108) ;
#29406 = AXIS2_PLACEMENT_3D('',#42129,#33111,#33112) ;
#29407 = AXIS2_PLACEMENT_3D('',#42133,#33114,#33115) ;
#29408 = AXIS2_PLACEMENT_3D('',#42185,#33141,#33142) ;
#29409 = AXIS2_PLACEMENT_3D('',#42207,#33153,#33154) ;
#29410 = AXIS2_PLACEMENT_3D('',#42215,#33158,#33159) ;
#29411 = AXIS2_PLACEMENT_3D('',#42223,#33163,#33164) ;
#29412 = AXIS2_PLACEMENT_3D('',#42237,#33171,#33172) ;
#29413 = AXIS2_PLACEMENT_3D('',#42245,#33176,#33177) ;
#29414 = AXIS2_PLACEMENT_3D('',#42300,#33205,#33206) ;
#29415 = AXIS2_PLACEMENT_3D('',#42311,#33211,#33212) ;
#29416 = AXIS2_PLACEMENT_3D('',#42390,#33252,#33253) ;
#29417 = AXIS2_PLACEMENT_3D('',#42396,#33257,#33258) ;
#29418 = AXIS2_PLACEMENT_3D('',#42398,#33259,#33260) ;
#29419 = AXIS2_PLACEMENT_3D('',#42400,#33262,#33263) ;
#29420 = AXIS2_PLACEMENT_3D('',#42406,#33266,#33267) ;
#29421 = AXIS2_PLACEMENT_3D('',#42412,#33270,#33271) ;
#29422 = AXIS2_PLACEMENT_3D('',#42420,#33275,#33276) ;
#29423 = AXIS2_PLACEMENT_3D('',#42426,#33279,#33280) ;
#29424 = AXIS2_PLACEMENT_3D('',#42431,#33283,#33284) ;
#29425 = AXIS2_PLACEMENT_3D('',#42433,#33285,#33286) ;
#29426 = AXIS2_PLACEMENT_3D('',#42439,#33289,#33290) ;
#29427 = AXIS2_PLACEMENT_3D('',#42445,#33293,#33294) ;
#29428 = AXIS2_PLACEMENT_3D('',#42451,#33297,#33298) ;
#29429 = AXIS2_PLACEMENT_3D('',#42459,#33302,#33303) ;
#29430 = AXIS2_PLACEMENT_3D('',#42465,#33306,#33307) ;
#29431 = AXIS2_PLACEMENT_3D('',#42471,#33310,#33311) ;
#29432 = AXIS2_PLACEMENT_3D('',#42477,#33314,#33315) ;
#29433 = AXIS2_PLACEMENT_3D('',#42483,#33318,#33319) ;
#29434 = AXIS2_PLACEMENT_3D('',#42489,#33322,#33323) ;
#29435 = AXIS2_PLACEMENT_3D('',#42495,#33326,#33327) ;
#29436 = AXIS2_PLACEMENT_3D('',#42503,#33331,#33332) ;
#29437 = AXIS2_PLACEMENT_3D('',#42509,#33335,#33336) ;
#29438 = AXIS2_PLACEMENT_3D('',#42515,#33339,#33340) ;
#29439 = AXIS2_PLACEMENT_3D('',#42521,#33343,#33344) ;
#29440 = AXIS2_PLACEMENT_3D('',#42527,#33347,#33348) ;
#29441 = AXIS2_PLACEMENT_3D('',#42533,#33351,#33352) ;
#29442 = AXIS2_PLACEMENT_3D('',#42539,#33355,#33356) ;
#29443 = AXIS2_PLACEMENT_3D('',#42547,#33360,#33361) ;
#29444 = AXIS2_PLACEMENT_3D('',#42553,#33364,#33365) ;
#29445 = AXIS2_PLACEMENT_3D('',#42559,#33368,#33369) ;
#29446 = AXIS2_PLACEMENT_3D('',#42576,#33380,#33381) ;
#29447 = AXIS2_PLACEMENT_3D('',#42582,#33385,#33386) ;
#29448 = AXIS2_PLACEMENT_3D('',#42585,#33388,#33389) ;
#29449 = AXIS2_PLACEMENT_3D('',#42586,#33390,#33391) ;
#29450 = AXIS2_PLACEMENT_3D('',#42597,#33397,#33398) ;
#29451 = AXIS2_PLACEMENT_3D('',#42639,#33419,#33420) ;
#29452 = AXIS2_PLACEMENT_3D('',#42696,#33449,#33450) ;
#29453 = AXIS2_PLACEMENT_3D('',#42701,#33452,#33453) ;
#29454 = AXIS2_PLACEMENT_3D('',#42711,#33458,#33459) ;
#29455 = AXIS2_PLACEMENT_3D('',#42719,#33463,#33464) ;
#29456 = AXIS2_PLACEMENT_3D('',#42733,#33471,#33472) ;
#29457 = AXIS2_PLACEMENT_3D('',#42771,#33491,#33492) ;
#29458 = AXIS2_PLACEMENT_3D('',#42782,#33498,#33499) ;
#29459 = AXIS2_PLACEMENT_3D('',#42809,#33512,#33513) ;
#29460 = AXIS2_PLACEMENT_3D('',#42889,#33553,#33554) ;
#29461 = AXIS2_PLACEMENT_3D('',#42895,#33557,#33558) ;
#29462 = AXIS2_PLACEMENT_3D('',#42901,#33561,#33562) ;
#29463 = AXIS2_PLACEMENT_3D('',#42909,#33566,#33567) ;
#29464 = AXIS2_PLACEMENT_3D('',#42921,#33574,#33575) ;
#29465 = AXIS2_PLACEMENT_3D('',#42923,#33577,#33578) ;
#29466 = AXIS2_PLACEMENT_3D('',#42925,#33580,#33581) ;
#29467 = AXIS2_PLACEMENT_3D('',#42927,#33583,#33584) ;
#29468 = AXIS2_PLACEMENT_3D('',#42930,#33587,#33588) ;
#29469 = AXIS2_PLACEMENT_3D('',#42933,#33591,#33592) ;
#29470 = AXIS2_PLACEMENT_3D('',#42936,#33595,#33596) ;
#29471 = AXIS2_PLACEMENT_3D('',#42939,#33599,#33600) ;
#29472 = AXIS2_PLACEMENT_3D('',#42942,#33603,#33604) ;
#29473 = AXIS2_PLACEMENT_3D('',#42945,#33607,#33608) ;
#29474 = AXIS2_PLACEMENT_3D('',#42948,#33611,#33612) ;
#29475 = AXIS2_PLACEMENT_3D('',#42951,#33615,#33616) ;
#29476 = AXIS2_PLACEMENT_3D('',#42954,#33619,#33620) ;
#29477 = AXIS2_PLACEMENT_3D('',#42957,#33623,#33624) ;
#29478 = AXIS2_PLACEMENT_3D('',#42959,#33626,#33627) ;
#29479 = AXIS2_PLACEMENT_3D('',#42961,#33629,#33630) ;
#29480 = AXIS2_PLACEMENT_3D('',#42964,#33633,#33634) ;
#29481 = AXIS2_PLACEMENT_3D('',#42966,#33636,#33637) ;
#29482 = AXIS2_PLACEMENT_3D('',#42968,#33639,#33640) ;
#29483 = AXIS2_PLACEMENT_3D('',#42970,#33642,#33643) ;
#29484 = AXIS2_PLACEMENT_3D('',#42971,#33644,#33645) ;
#29485 = AXIS2_PLACEMENT_3D('',#42973,#33647,#33648) ;
#29486 = AXIS2_PLACEMENT_3D('',#42975,#33650,#33651) ;
#29487 = AXIS2_PLACEMENT_3D('',#42977,#33653,#33654) ;
#29488 = AXIS2_PLACEMENT_3D('',#42979,#33656,#33657) ;
#29489 = AXIS2_PLACEMENT_3D('',#42981,#33659,#33660) ;
#29490 = AXIS2_PLACEMENT_3D('',#42983,#33662,#33663) ;
#29491 = AXIS2_PLACEMENT_3D('',#42985,#33665,#33666) ;
#29492 = AXIS2_PLACEMENT_3D('',#42987,#33668,#33669) ;
#29493 = AXIS2_PLACEMENT_3D('',#42989,#33671,#33672) ;
#29494 = AXIS2_PLACEMENT_3D('',#42992,#33675,#33676) ;
#29495 = AXIS2_PLACEMENT_3D('',#42994,#33678,#33679) ;
#29496 = AXIS2_PLACEMENT_3D('',#42996,#33681,#33682) ;
#29497 = AXIS2_PLACEMENT_3D('',#42999,#33685,#33686) ;
#29498 = AXIS2_PLACEMENT_3D('',#43001,#33688,#33689) ;
#29499 = AXIS2_PLACEMENT_3D('',#43003,#33691,#33692) ;
#29500 = AXIS2_PLACEMENT_3D('',#43005,#33694,#33695) ;
#29501 = AXIS2_PLACEMENT_3D('',#43006,#33696,#33697) ;
#29502 = AXIS2_PLACEMENT_3D('',#43009,#33700,#33701) ;
#29503 = AXIS2_PLACEMENT_3D('',#43012,#33704,#33705) ;
#29504 = AXIS2_PLACEMENT_3D('',#43015,#33708,#33709) ;
#29505 = AXIS2_PLACEMENT_3D('',#43018,#33712,#33713) ;
#29506 = AXIS2_PLACEMENT_3D('',#43021,#33716,#33717) ;
#29507 = AXIS2_PLACEMENT_3D('',#43023,#33719,#33720) ;
#29508 = AXIS2_PLACEMENT_3D('',#43025,#33722,#33723) ;
#29509 = AXIS2_PLACEMENT_3D('',#43026,#33724,#33725) ;
#29510 = AXIS2_PLACEMENT_3D('',#43028,#33727,#33728) ;
#29511 = AXIS2_PLACEMENT_3D('',#43030,#33730,#33731) ;
#29512 = AXIS2_PLACEMENT_3D('',#43031,#33732,#33733) ;
#29513 = AXIS2_PLACEMENT_3D('',#43033,#33735,#33736) ;
#29514 = AXIS2_PLACEMENT_3D('',#43034,#33737,#33738) ;
#29515 = AXIS2_PLACEMENT_3D('',#43036,#33740,#33741) ;
#29516 = AXIS2_PLACEMENT_3D('',#43037,#33742,#33743) ;
#29517 = AXIS2_PLACEMENT_3D('',#43039,#33745,#33746) ;
#29518 = AXIS2_PLACEMENT_3D('',#43040,#33747,#33748) ;
#29519 = AXIS2_PLACEMENT_3D('',#43042,#33750,#33751) ;
#29520 = AXIS2_PLACEMENT_3D('',#43044,#33753,#33754) ;
#29521 = AXIS2_PLACEMENT_3D('',#43046,#33756,#33757) ;
#29522 = AXIS2_PLACEMENT_3D('',#43049,#33760,#33761) ;
#29523 = AXIS2_PLACEMENT_3D('',#43052,#33764,#33765) ;
#29524 = AXIS2_PLACEMENT_3D('',#43054,#33767,#33768) ;
#29525 = AXIS2_PLACEMENT_3D('',#43056,#33770,#33771) ;
#29526 = AXIS2_PLACEMENT_3D('',#43058,#33773,#33774) ;
#29527 = AXIS2_PLACEMENT_3D('',#43059,#33775,#33776) ;
#29528 = AXIS2_PLACEMENT_3D('',#43061,#33778,#33779) ;
#29529 = AXIS2_PLACEMENT_3D('',#43064,#33782,#33783) ;
#29530 = AXIS2_PLACEMENT_3D('',#43067,#33786,#33787) ;
#29531 = AXIS2_PLACEMENT_3D('',#43069,#33789,#33790) ;
#29532 = AXIS2_PLACEMENT_3D('',#43072,#33793,#33794) ;
#29533 = AXIS2_PLACEMENT_3D('',#43075,#33797,#33798) ;
#29534 = AXIS2_PLACEMENT_3D('',#43077,#33800,#33801) ;
#29535 = AXIS2_PLACEMENT_3D('',#43078,#33802,#33803) ;
#29536 = AXIS2_PLACEMENT_3D('',#43080,#33805,#33806) ;
#29537 = AXIS2_PLACEMENT_3D('',#43082,#33808,#33809) ;
#29538 = AXIS2_PLACEMENT_3D('',#43083,#33810,#33811) ;
#29539 = AXIS2_PLACEMENT_3D('',#43085,#33813,#33814) ;
#29540 = AXIS2_PLACEMENT_3D('',#43086,#33815,#33816) ;
#29541 = AXIS2_PLACEMENT_3D('',#43088,#33818,#33819) ;
#29542 = AXIS2_PLACEMENT_3D('',#43090,#33821,#33822) ;
#29543 = AXIS2_PLACEMENT_3D('',#43092,#33824,#33825) ;
#29544 = AXIS2_PLACEMENT_3D('',#43094,#33827,#33828) ;
#29545 = AXIS2_PLACEMENT_3D('',#43095,#33829,#33830) ;
#29546 = AXIS2_PLACEMENT_3D('',#43097,#33832,#33833) ;
#29547 = AXIS2_PLACEMENT_3D('',#43098,#33834,#33835) ;
#29548 = AXIS2_PLACEMENT_3D('',#43100,#33837,#33838) ;
#29549 = AXIS2_PLACEMENT_3D('',#43103,#33841,#33842) ;
#29550 = AXIS2_PLACEMENT_3D('',#43105,#33844,#33845) ;
#29551 = AXIS2_PLACEMENT_3D('',#43108,#33848,#33849) ;
#29552 = AXIS2_PLACEMENT_3D('',#43110,#33851,#33852) ;
#29553 = AXIS2_PLACEMENT_3D('',#43112,#33854,#33855) ;
#29554 = AXIS2_PLACEMENT_3D('',#43114,#33857,#33858) ;
#29555 = AXIS2_PLACEMENT_3D('',#43116,#33860,#33861) ;
#29556 = AXIS2_PLACEMENT_3D('',#43117,#33862,#33863) ;
#29557 = AXIS2_PLACEMENT_3D('',#43120,#33866,#33867) ;
#29558 = AXIS2_PLACEMENT_3D('',#43123,#33870,#33871) ;
#29559 = AXIS2_PLACEMENT_3D('',#43126,#33874,#33875) ;
#29560 = AXIS2_PLACEMENT_3D('',#43129,#33878,#33879) ;
#29561 = AXIS2_PLACEMENT_3D('',#43132,#33882,#33883) ;
#29562 = AXIS2_PLACEMENT_3D('',#43134,#33885,#33886) ;
#29563 = AXIS2_PLACEMENT_3D('',#43136,#33888,#33889) ;
#29564 = AXIS2_PLACEMENT_3D('',#43137,#33890,#33891) ;
#29565 = AXIS2_PLACEMENT_3D('',#43138,#33892,#33893) ;
#29566 = AXIS2_PLACEMENT_3D('',#43140,#33895,#33896) ;
#29567 = AXIS2_PLACEMENT_3D('',#43142,#33898,#33899) ;
#29568 = AXIS2_PLACEMENT_3D('',#43143,#33900,#33901) ;
#29569 = AXIS2_PLACEMENT_3D('',#43145,#33903,#33904) ;
#29570 = AXIS2_PLACEMENT_3D('',#43147,#33906,#33907) ;
#29571 = AXIS2_PLACEMENT_3D('',#43148,#33908,#33909) ;
#29572 = AXIS2_PLACEMENT_3D('',#43150,#33911,#33912) ;
#29573 = AXIS2_PLACEMENT_3D('',#43151,#33913,#33914) ;
#29574 = AXIS2_PLACEMENT_3D('',#43153,#33916,#33917) ;
#29575 = AXIS2_PLACEMENT_3D('',#43154,#33918,#33919) ;
#29576 = AXIS2_PLACEMENT_3D('',#43156,#33921,#33922) ;
#29577 = AXIS2_PLACEMENT_3D('',#43157,#33923,#33924) ;
#29578 = AXIS2_PLACEMENT_3D('',#43159,#33926,#33927) ;
#29579 = AXIS2_PLACEMENT_3D('',#43162,#33930,#33931) ;
#29580 = AXIS2_PLACEMENT_3D('',#43165,#33934,#33935) ;
#29581 = AXIS2_PLACEMENT_3D('',#43168,#33938,#33939) ;
#29582 = AXIS2_PLACEMENT_3D('',#43171,#33942,#33943) ;
#29583 = AXIS2_PLACEMENT_3D('',#43173,#33945,#33946) ;
#29584 = AXIS2_PLACEMENT_3D('',#43176,#33949,#33950) ;
#29585 = AXIS2_PLACEMENT_3D('',#43178,#33952,#33953) ;
#29586 = AXIS2_PLACEMENT_3D('',#43181,#33956,#33957) ;
#29587 = AXIS2_PLACEMENT_3D('',#43183,#33959,#33960) ;
#29588 = AXIS2_PLACEMENT_3D('',#43185,#33962,#33963) ;
#29589 = AXIS2_PLACEMENT_3D('',#43187,#33965,#33966) ;
#29590 = AXIS2_PLACEMENT_3D('',#43188,#33967,#33968) ;
#29591 = AXIS2_PLACEMENT_3D('',#43190,#33970,#33971) ;
#29592 = AXIS2_PLACEMENT_3D('',#43191,#33972,#33973) ;
#29593 = AXIS2_PLACEMENT_3D('',#43193,#33975,#33976) ;
#29594 = AXIS2_PLACEMENT_3D('',#43195,#33978,#33979) ;
#29595 = AXIS2_PLACEMENT_3D('',#43196,#33980,#33981) ;
#29596 = AXIS2_PLACEMENT_3D('',#43198,#33983,#33984) ;
#29597 = AXIS2_PLACEMENT_3D('',#43200,#33986,#33987) ;
#29598 = AXIS2_PLACEMENT_3D('',#43201,#33988,#33989) ;
#29599 = AXIS2_PLACEMENT_3D('',#43203,#33991,#33992) ;
#29600 = AXIS2_PLACEMENT_3D('',#43204,#33993,#33994) ;
#29601 = AXIS2_PLACEMENT_3D('',#43206,#33996,#33997) ;
#29602 = AXIS2_PLACEMENT_3D('',#43207,#33998,#33999) ;
#29603 = AXIS2_PLACEMENT_3D('',#43209,#34001,#34002) ;
#29604 = AXIS2_PLACEMENT_3D('',#43211,#34004,#34005) ;
#29605 = AXIS2_PLACEMENT_3D('',#43213,#34007,#34008) ;
#29606 = AXIS2_PLACEMENT_3D('',#43215,#34010,#34011) ;
#29607 = AXIS2_PLACEMENT_3D('',#43217,#34013,#34014) ;
#29608 = AXIS2_PLACEMENT_3D('',#43219,#34016,#34017) ;
#29609 = AXIS2_PLACEMENT_3D('',#43222,#34020,#34021) ;
#29610 = AXIS2_PLACEMENT_3D('',#43224,#34023,#34024) ;
#29611 = AXIS2_PLACEMENT_3D('',#43225,#34025,#34026) ;
#29612 = AXIS2_PLACEMENT_3D('',#43227,#34028,#34029) ;
#29613 = AXIS2_PLACEMENT_3D('',#43230,#34032,#34033) ;
#29614 = AXIS2_PLACEMENT_3D('',#43233,#34036,#34037) ;
#29615 = AXIS2_PLACEMENT_3D('',#43236,#34040,#34041) ;
#29616 = AXIS2_PLACEMENT_3D('',#43239,#34044,#34045) ;
#29617 = AXIS2_PLACEMENT_3D('',#43242,#34048,#34049) ;
#29618 = AXIS2_PLACEMENT_3D('',#43245,#34052,#34053) ;
#29619 = AXIS2_PLACEMENT_3D('',#43246,#34054,#34055) ;
#29620 = AXIS2_PLACEMENT_3D('',#43247,#34056,#34057) ;
#29621 = AXIS2_PLACEMENT_3D('',#43249,#34059,#34060) ;
#29622 = AXIS2_PLACEMENT_3D('',#43251,#34062,#34063) ;
#29623 = AXIS2_PLACEMENT_3D('',#43252,#34064,#34065) ;
#29624 = AXIS2_PLACEMENT_3D('',#43253,#34066,#34067) ;
#29625 = AXIS2_PLACEMENT_3D('',#43255,#34069,#34070) ;
#29626 = AXIS2_PLACEMENT_3D('',#43256,#34071,#34072) ;
#29627 = AXIS2_PLACEMENT_3D('',#43258,#34074,#34075) ;
#29628 = AXIS2_PLACEMENT_3D('',#43259,#34076,#34077) ;
#29629 = AXIS2_PLACEMENT_3D('',#43261,#34079,#34080) ;
#29630 = AXIS2_PLACEMENT_3D('',#43263,#34082,#34083) ;
#29631 = AXIS2_PLACEMENT_3D('',#43264,#34084,#34085) ;
#29632 = AXIS2_PLACEMENT_3D('',#43266,#34087,#34088) ;
#29633 = AXIS2_PLACEMENT_3D('',#43267,#34089,#34090) ;
#29634 = AXIS2_PLACEMENT_3D('',#43269,#34092,#34093) ;
#29635 = AXIS2_PLACEMENT_3D('',#43271,#34095,#34096) ;
#29636 = AXIS2_PLACEMENT_3D('',#43273,#34098,#34099) ;
#29637 = AXIS2_PLACEMENT_3D('',#43275,#34101,#34102) ;
#29638 = AXIS2_PLACEMENT_3D('',#43277,#34104,#34105) ;
#29639 = AXIS2_PLACEMENT_3D('',#43279,#34107,#34108) ;
#29640 = AXIS2_PLACEMENT_3D('',#43280,#34109,#34110) ;
#29641 = AXIS2_PLACEMENT_3D('',#43283,#34113,#34114) ;
#29642 = AXIS2_PLACEMENT_3D('',#43286,#34117,#34118) ;
#29643 = AXIS2_PLACEMENT_3D('',#43289,#34121,#34122) ;
#29644 = AXIS2_PLACEMENT_3D('',#43292,#34125,#34126) ;
#29645 = AXIS2_PLACEMENT_3D('',#43295,#34129,#34130) ;
#29646 = AXIS2_PLACEMENT_3D('',#43296,#34131,#34132) ;
#29647 = AXIS2_PLACEMENT_3D('',#43297,#34133,#34134) ;
#29648 = AXIS2_PLACEMENT_3D('',#43299,#34136,#34137) ;
#29649 = AXIS2_PLACEMENT_3D('',#43300,#34138,#34139) ;
#29650 = AXIS2_PLACEMENT_3D('',#43301,#34140,#34141) ;
#29651 = AXIS2_PLACEMENT_3D('',#43302,#34142,#34143) ;
#29652 = AXIS2_PLACEMENT_3D('',#43304,#34145,#34146) ;
#29653 = AXIS2_PLACEMENT_3D('',#43306,#34148,#34149) ;
#29654 = AXIS2_PLACEMENT_3D('',#43307,#34150,#34151) ;
#29655 = AXIS2_PLACEMENT_3D('',#43309,#34153,#34154) ;
#29656 = AXIS2_PLACEMENT_3D('',#43311,#34156,#34157) ;
#29657 = AXIS2_PLACEMENT_3D('',#43312,#34158,#34159) ;
#29658 = AXIS2_PLACEMENT_3D('',#43314,#34161,#34162) ;
#29659 = AXIS2_PLACEMENT_3D('',#43316,#34164,#34165) ;
#29660 = AXIS2_PLACEMENT_3D('',#43319,#34168,#34169) ;
#29661 = AXIS2_PLACEMENT_3D('',#43322,#34172,#34173) ;
#29662 = AXIS2_PLACEMENT_3D('',#43325,#34176,#34177) ;
#29663 = AXIS2_PLACEMENT_3D('',#43327,#34179,#34180) ;
#29664 = AXIS2_PLACEMENT_3D('',#43330,#34183,#34184) ;
#29665 = AXIS2_PLACEMENT_3D('',#43331,#34185,#34186) ;
#29666 = AXIS2_PLACEMENT_3D('',#43333,#34188,#34189) ;
#29667 = AXIS2_PLACEMENT_3D('',#43335,#34191,#34192) ;
#29668 = AXIS2_PLACEMENT_3D('',#43336,#34193,#34194) ;
#29669 = AXIS2_PLACEMENT_3D('',#43338,#34196,#34197) ;
#29670 = AXIS2_PLACEMENT_3D('',#43339,#34198,#34199) ;
#29671 = AXIS2_PLACEMENT_3D('',#43340,#34200,#34201) ;
#29672 = AXIS2_PLACEMENT_3D('',#43342,#34203,#34204) ;
#29673 = AXIS2_PLACEMENT_3D('',#43343,#34205,#34206) ;
#29674 = AXIS2_PLACEMENT_3D('',#43345,#34208,#34209) ;
#29675 = AXIS2_PLACEMENT_3D('',#43347,#34211,#34212) ;
#29676 = AXIS2_PLACEMENT_3D('',#43349,#34214,#34215) ;
#29677 = AXIS2_PLACEMENT_3D('',#43350,#34216,#34217) ;
#29678 = AXIS2_PLACEMENT_3D('',#43352,#34219,#34220) ;
#29679 = AXIS2_PLACEMENT_3D('',#43354,#34222,#34223) ;
#29680 = AXIS2_PLACEMENT_3D('',#43356,#34225,#34226) ;
#29681 = AXIS2_PLACEMENT_3D('',#43357,#34227,#34228) ;
#29682 = AXIS2_PLACEMENT_3D('',#43359,#34230,#34231) ;
#29683 = AXIS2_PLACEMENT_3D('',#43361,#34233,#34234) ;
#29684 = AXIS2_PLACEMENT_3D('',#43364,#34237,#34238) ;
#29685 = AXIS2_PLACEMENT_3D('',#43367,#34241,#34242) ;
#29686 = AXIS2_PLACEMENT_3D('',#43370,#34245,#34246) ;
#29687 = AXIS2_PLACEMENT_3D('',#43372,#34248,#34249) ;
#29688 = AXIS2_PLACEMENT_3D('',#43374,#34251,#34252) ;
#29689 = AXIS2_PLACEMENT_3D('',#43375,#34253,#34254) ;
#29690 = AXIS2_PLACEMENT_3D('',#43377,#34256,#34257) ;
#29691 = AXIS2_PLACEMENT_3D('',#43378,#34258,#34259) ;
#29692 = AXIS2_PLACEMENT_3D('',#43380,#34261,#34262) ;
#29693 = AXIS2_PLACEMENT_3D('',#43381,#34263,#34264) ;
#29694 = AXIS2_PLACEMENT_3D('',#43382,#34265,#34266) ;
#29695 = AXIS2_PLACEMENT_3D('',#43384,#34268,#34269) ;
#29696 = AXIS2_PLACEMENT_3D('',#43386,#34271,#34272) ;
#29697 = AXIS2_PLACEMENT_3D('',#43387,#34273,#34274) ;
#29698 = AXIS2_PLACEMENT_3D('',#43389,#34276,#34277) ;
#29699 = AXIS2_PLACEMENT_3D('',#43390,#34278,#34279) ;
#29700 = AXIS2_PLACEMENT_3D('',#43393,#34282,#34283) ;
#29701 = AXIS2_PLACEMENT_3D('',#43394,#34284,#34285) ;
#29702 = AXIS2_PLACEMENT_3D('',#43397,#34288,#34289) ;
#29703 = AXIS2_PLACEMENT_3D('',#43398,#34290,#34291) ;
#29704 = AXIS2_PLACEMENT_3D('',#43400,#34293,#34294) ;
#29705 = AXIS2_PLACEMENT_3D('',#43401,#34295,#34296) ;
#29706 = AXIS2_PLACEMENT_3D('',#43403,#34298,#34299) ;
#29707 = AXIS2_PLACEMENT_3D('',#43404,#34300,#34301) ;
#29708 = AXIS2_PLACEMENT_3D('',#43406,#34303,#34304) ;
#29709 = AXIS2_PLACEMENT_3D('',#43408,#34306,#34307) ;
#29710 = AXIS2_PLACEMENT_3D('',#43410,#34309,#34310) ;
#29711 = AXIS2_PLACEMENT_3D('',#43412,#34312,#34313) ;
#29712 = AXIS2_PLACEMENT_3D('',#43414,#34315,#34316) ;
#29713 = AXIS2_PLACEMENT_3D('',#43416,#34318,#34319) ;
#29714 = AXIS2_PLACEMENT_3D('',#43417,#34320,#34321) ;
#29715 = AXIS2_PLACEMENT_3D('',#43419,#34323,#34324) ;
#29716 = AXIS2_PLACEMENT_3D('',#43420,#34325,#34326) ;
#29717 = AXIS2_PLACEMENT_3D('',#43422,#34328,#34329) ;
#29718 = AXIS2_PLACEMENT_3D('',#43424,#34331,#34332) ;
#29719 = AXIS2_PLACEMENT_3D('',#43425,#34333,#34334) ;
#29720 = AXIS2_PLACEMENT_3D('',#43426,#34335,#34336) ;
#29721 = AXIS2_PLACEMENT_3D('',#43428,#34338,#34339) ;
#29722 = AXIS2_PLACEMENT_3D('',#43430,#34341,#34342) ;
#29723 = AXIS2_PLACEMENT_3D('',#43432,#34344,#34345) ;
#29724 = AXIS2_PLACEMENT_3D('',#43433,#34346,#34347) ;
#29725 = AXIS2_PLACEMENT_3D('',#43434,#34348,#34349) ;
#29726 = AXIS2_PLACEMENT_3D('',#43436,#34351,#34352) ;
#29727 = AXIS2_PLACEMENT_3D('',#43438,#34354,#34355) ;
#29728 = AXIS2_PLACEMENT_3D('',#43439,#34356,#34357) ;
#29729 = AXIS2_PLACEMENT_3D('',#43440,#34358,#34359) ;
#29730 = AXIS2_PLACEMENT_3D('',#43441,#34360,#34361) ;
#29731 = AXIS2_PLACEMENT_3D('',#43442,#34362,#34363) ;
#29732 = AXIS2_PLACEMENT_3D('',#43445,#34364,#34365) ;
#29733 = AXIS2_PLACEMENT_3D('',#43446,#34366,#34367) ;
#29734 = AXIS2_PLACEMENT_3D('',#43447,#34368,#34369) ;
#29735 = AXIS2_PLACEMENT_3D('',#43450,#34370,#34371) ;
#29736 = AXIS2_PLACEMENT_3D('',#43451,#34372,#34373) ;
#29737 = AXIS2_PLACEMENT_3D('',#43452,#34374,#34375) ;
#29738 = AXIS2_PLACEMENT_3D('',#43455,#34376,#34377) ;
#29739 = AXIS2_PLACEMENT_3D('',#43456,#34378,#34379) ;
#29740 = AXIS2_PLACEMENT_3D('',#43457,#34380,#34381) ;
#29741 = AXIS2_PLACEMENT_3D('',#43460,#34382,#34383) ;
#29742 = AXIS2_PLACEMENT_3D('',#43461,#34384,#34385) ;
#29743 = AXIS2_PLACEMENT_3D('',#43462,#34386,#34387) ;
#29744 = AXIS2_PLACEMENT_3D('',#43465,#34388,#34389) ;
#29745 = AXIS2_PLACEMENT_3D('',#43466,#34390,#34391) ;
#29746 = AXIS2_PLACEMENT_3D('',#43467,#34392,#34393) ;
#29747 = AXIS2_PLACEMENT_3D('',#43470,#34394,#34395) ;
#29748 = AXIS2_PLACEMENT_3D('',#43471,#34396,#34397) ;
#29749 = AXIS2_PLACEMENT_3D('',#43472,#34398,#34399) ;
#29750 = AXIS2_PLACEMENT_3D('',#43475,#34400,#34401) ;
#29751 = AXIS2_PLACEMENT_3D('',#43476,#34402,#34403) ;
#29752 = AXIS2_PLACEMENT_3D('',#43477,#34404,#34405) ;
#29753 = AXIS2_PLACEMENT_3D('',#43480,#34406,#34407) ;
#29754 = AXIS2_PLACEMENT_3D('',#43482,#34408,#34409) ;
#29755 = AXIS2_PLACEMENT_3D('',#43483,#34410,#34411) ;
#29756 = AXIS2_PLACEMENT_3D('',#43484,#34412,#34413) ;
#29757 = AXIS2_PLACEMENT_3D('',#43487,#34414,#34415) ;
#29758 = AXIS2_PLACEMENT_3D('',#43489,#34416,#34417) ;
#29759 = AXIS2_PLACEMENT_3D('',#43491,#34418,#34419) ;
#29760 = AXIS2_PLACEMENT_3D('',#43492,#34420,#34421) ;
#29761 = AXIS2_PLACEMENT_3D('',#43493,#34422,#34423) ;
#29762 = AXIS2_PLACEMENT_3D('',#43496,#34424,#34425) ;
#29763 = AXIS2_PLACEMENT_3D('',#43498,#34426,#34427) ;
#29764 = AXIS2_PLACEMENT_3D('',#43500,#34428,#34429) ;
#29765 = AXIS2_PLACEMENT_3D('',#43501,#34430,#34431) ;
#29766 = AXIS2_PLACEMENT_3D('',#43502,#34432,#34433) ;
#29767 = AXIS2_PLACEMENT_3D('',#43505,#34434,#34435) ;
#29768 = AXIS2_PLACEMENT_3D('',#43507,#34436,#34437) ;
#29769 = AXIS2_PLACEMENT_3D('',#43509,#34438,#34439) ;
#29770 = AXIS2_PLACEMENT_3D('',#43510,#34440,#34441) ;
#29771 = AXIS2_PLACEMENT_3D('',#43511,#34442,#34443) ;
#29772 = AXIS2_PLACEMENT_3D('',#43514,#34444,#34445) ;
#29773 = AXIS2_PLACEMENT_3D('',#43516,#34446,#34447) ;
#29774 = AXIS2_PLACEMENT_3D('',#43518,#34448,#34449) ;
#29775 = AXIS2_PLACEMENT_3D('',#43519,#34450,#34451) ;
#29776 = AXIS2_PLACEMENT_3D('',#43520,#34452,#34453) ;
#29777 = AXIS2_PLACEMENT_3D('',#43523,#34454,#34455) ;
#29778 = AXIS2_PLACEMENT_3D('',#43525,#34456,#34457) ;
#29779 = AXIS2_PLACEMENT_3D('',#43527,#34458,#34459) ;
#29780 = AXIS2_PLACEMENT_3D('',#43528,#34460,#34461) ;
#29781 = AXIS2_PLACEMENT_3D('',#43529,#34462,#34463) ;
#29782 = AXIS2_PLACEMENT_3D('',#43532,#34464,#34465) ;
#29783 = AXIS2_PLACEMENT_3D('',#43534,#34466,#34467) ;
#29784 = AXIS2_PLACEMENT_3D('',#43536,#34468,#34469) ;
#29785 = AXIS2_PLACEMENT_3D('',#43537,#34470,#34471) ;
#29786 = AXIS2_PLACEMENT_3D('',#43538,#34472,#34473) ;
#29787 = AXIS2_PLACEMENT_3D('',#43541,#34474,#34475) ;
#29788 = AXIS2_PLACEMENT_3D('',#43543,#34476,#34477) ;
#29789 = AXIS2_PLACEMENT_3D('',#43545,#34478,#34479) ;
#29790 = AXIS2_PLACEMENT_3D('',#43546,#34480,#34481) ;
#29791 = AXIS2_PLACEMENT_3D('',#43547,#34482,#34483) ;
#29792 = AXIS2_PLACEMENT_3D('',#43550,#34484,#34485) ;
#29793 = AXIS2_PLACEMENT_3D('',#43552,#34486,#34487) ;
#29794 = AXIS2_PLACEMENT_3D('',#43554,#34488,#34489) ;
#29795 = AXIS2_PLACEMENT_3D('',#43555,#34490,#34491) ;
#29796 = AXIS2_PLACEMENT_3D('',#43556,#34492,#34493) ;
#29797 = AXIS2_PLACEMENT_3D('',#43559,#34494,#34495) ;
#29798 = AXIS2_PLACEMENT_3D('',#43561,#34496,#34497) ;
#29799 = AXIS2_PLACEMENT_3D('',#43563,#34498,#34499) ;
#29800 = AXIS2_PLACEMENT_3D('',#43564,#34500,#34501) ;
#29801 = AXIS2_PLACEMENT_3D('',#43565,#34502,#34503) ;
#29802 = AXIS2_PLACEMENT_3D('',#43568,#34504,#34505) ;
#29803 = AXIS2_PLACEMENT_3D('',#43570,#34506,#34507) ;
#29804 = AXIS2_PLACEMENT_3D('',#43572,#34508,#34509) ;
#29805 = AXIS2_PLACEMENT_3D('',#43573,#34510,#34511) ;
#29806 = AXIS2_PLACEMENT_3D('',#43574,#34512,#34513) ;
#29807 = AXIS2_PLACEMENT_3D('',#43577,#34514,#34515) ;
#29808 = AXIS2_PLACEMENT_3D('',#43579,#34516,#34517) ;
#29809 = AXIS2_PLACEMENT_3D('',#43581,#34518,#34519) ;
#29810 = AXIS2_PLACEMENT_3D('',#43582,#34520,#34521) ;
#29811 = AXIS2_PLACEMENT_3D('',#43583,#34522,#34523) ;
#29812 = AXIS2_PLACEMENT_3D('',#43586,#34524,#34525) ;
#29813 = AXIS2_PLACEMENT_3D('',#43588,#34526,#34527) ;
#29814 = AXIS2_PLACEMENT_3D('',#43590,#34528,#34529) ;
#29815 = AXIS2_PLACEMENT_3D('',#43591,#34530,#34531) ;
#29816 = AXIS2_PLACEMENT_3D('',#43592,#34532,#34533) ;
#29817 = AXIS2_PLACEMENT_3D('',#43595,#34534,#34535) ;
#29818 = AXIS2_PLACEMENT_3D('',#43597,#34536,#34537) ;
#29819 = AXIS2_PLACEMENT_3D('',#43599,#34538,#34539) ;
#29820 = AXIS2_PLACEMENT_3D('',#43600,#34540,#34541) ;
#29821 = AXIS2_PLACEMENT_3D('',#43601,#34542,#34543) ;
#29822 = AXIS2_PLACEMENT_3D('',#43604,#34544,#34545) ;
#29823 = AXIS2_PLACEMENT_3D('',#43606,#34546,#34547) ;
#29824 = AXIS2_PLACEMENT_3D('',#43607,#34548,#34549) ;
#29825 = AXIS2_PLACEMENT_3D('',#43608,#34550,#34551) ;
#29826 = AXIS2_PLACEMENT_3D('',#43611,#34552,#34553) ;
#29827 = AXIS2_PLACEMENT_3D('',#43612,#34554,#34555) ;
#29828 = AXIS2_PLACEMENT_3D('',#43613,#34556,#34557) ;
#29829 = AXIS2_PLACEMENT_3D('',#43616,#34558,#34559) ;
#29830 = AXIS2_PLACEMENT_3D('',#43617,#34560,#34561) ;
#29831 = AXIS2_PLACEMENT_3D('',#43618,#34562,#34563) ;
#29832 = AXIS2_PLACEMENT_3D('',#43621,#34564,#34565) ;
#29833 = AXIS2_PLACEMENT_3D('',#43622,#34566,#34567) ;
#29834 = AXIS2_PLACEMENT_3D('',#43623,#34568,#34569) ;
#29835 = AXIS2_PLACEMENT_3D('',#43626,#34570,#34571) ;
#29836 = AXIS2_PLACEMENT_3D('',#43627,#34572,#34573) ;
#29837 = AXIS2_PLACEMENT_3D('',#43628,#34574,#34575) ;
#29838 = AXIS2_PLACEMENT_3D('',#43631,#34576,#34577) ;
#29839 = AXIS2_PLACEMENT_3D('',#43632,#34578,#34579) ;
#29840 = AXIS2_PLACEMENT_3D('',#43633,#34580,#34581) ;
#29841 = AXIS2_PLACEMENT_3D('',#43636,#34582,#34583) ;
#29842 = AXIS2_PLACEMENT_3D('',#43637,#34584,#34585) ;
#29843 = AXIS2_PLACEMENT_3D('',#43638,#34586,#34587) ;
#29844 = AXIS2_PLACEMENT_3D('',#43640,#34588,#34589) ;
#29845 = AXIS2_PLACEMENT_3D('',#43641,#34590,#34591) ;
#29846 = AXIS2_PLACEMENT_3D('',#43644,#34593,#34594) ;
#29847 = AXIS2_PLACEMENT_3D('',#43645,#34595,#34596) ;
#29848 = AXIS2_PLACEMENT_3D('',#43646,#34597,#34598) ;
#29849 = AXIS2_PLACEMENT_3D('',#43649,#34600,#34601) ;
#29850 = AXIS2_PLACEMENT_3D('',#43650,#34602,#34603) ;
#29851 = AXIS2_PLACEMENT_3D('',#43651,#34604,#34605) ;
#29852 = AXIS2_PLACEMENT_3D('',#43654,#34607,#34608) ;
#29853 = AXIS2_PLACEMENT_3D('',#43655,#34609,#34610) ;
#29854 = AXIS2_PLACEMENT_3D('',#43656,#34611,#34612) ;
#29855 = AXIS2_PLACEMENT_3D('',#43659,#34614,#34615) ;
#29856 = AXIS2_PLACEMENT_3D('',#43660,#34616,#34617) ;
#29857 = AXIS2_PLACEMENT_3D('',#43661,#34618,#34619) ;
#29858 = AXIS2_PLACEMENT_3D('',#43664,#34621,#34622) ;
#29859 = AXIS2_PLACEMENT_3D('',#43665,#34623,#34624) ;
#29860 = AXIS2_PLACEMENT_3D('',#43666,#34625,#34626) ;
#29861 = AXIS2_PLACEMENT_3D('',#43669,#34628,#34629) ;
#29862 = AXIS2_PLACEMENT_3D('',#43670,#34630,#34631) ;
#29863 = AXIS2_PLACEMENT_3D('',#43671,#34632,#34633) ;
#29864 = AXIS2_PLACEMENT_3D('',#43674,#34635,#34636) ;
#29865 = AXIS2_PLACEMENT_3D('',#43675,#34637,#34638) ;
#29866 = AXIS2_PLACEMENT_3D('',#43676,#34639,#34640) ;
#29867 = AXIS2_PLACEMENT_3D('',#43678,#34642,#34643) ;
#29868 = AXIS2_PLACEMENT_3D('',#43679,#34644,#34645) ;
#29869 = AXIS2_PLACEMENT_3D('',#43681,#34647,#34648) ;
#29870 = AXIS2_PLACEMENT_3D('',#43682,#34649,#34650) ;
#29871 = AXIS2_PLACEMENT_3D('',#43684,#34652,#34653) ;
#29872 = AXIS2_PLACEMENT_3D('',#43685,#34654,#34655) ;
#29873 = AXIS2_PLACEMENT_3D('',#43687,#34657,#34658) ;
#29874 = AXIS2_PLACEMENT_3D('',#43688,#34659,#34660) ;
#29875 = AXIS2_PLACEMENT_3D('',#43690,#34662,#34663) ;
#29876 = AXIS2_PLACEMENT_3D('',#43691,#34664,#34665) ;
#29877 = AXIS2_PLACEMENT_3D('',#43693,#34667,#34668) ;
#29878 = AXIS2_PLACEMENT_3D('',#43694,#34669,#34670) ;
#29879 = AXIS2_PLACEMENT_3D('',#43696,#34672,#34673) ;
#29880 = AXIS2_PLACEMENT_3D('',#43697,#34674,#34675) ;
#29881 = AXIS2_PLACEMENT_3D('',#43699,#34677,#34678) ;
#29882 = AXIS2_PLACEMENT_3D('',#43700,#34679,#34680) ;
#29883 = AXIS2_PLACEMENT_3D('',#43702,#34682,#34683) ;
#29884 = AXIS2_PLACEMENT_3D('',#43703,#34684,#34685) ;
#29885 = AXIS2_PLACEMENT_3D('',#43705,#34687,#34688) ;
#29886 = AXIS2_PLACEMENT_3D('',#43706,#34689,#34690) ;
#29887 = AXIS2_PLACEMENT_3D('',#43708,#34692,#34693) ;
#29888 = AXIS2_PLACEMENT_3D('',#43709,#34694,#34695) ;
#29889 = AXIS2_PLACEMENT_3D('',#43711,#34697,#34698) ;
#29890 = AXIS2_PLACEMENT_3D('',#43712,#34699,#34700) ;
#29891 = AXIS2_PLACEMENT_3D('',#43714,#34702,#34703) ;
#29892 = AXIS2_PLACEMENT_3D('',#43715,#34704,#34705) ;
#29893 = AXIS2_PLACEMENT_3D('',#43718,#34707,#34708) ;
#29894 = AXIS2_PLACEMENT_3D('',#43719,#34709,#34710) ;
#29895 = AXIS2_PLACEMENT_3D('',#43720,#34711,#34712) ;
#29896 = AXIS2_PLACEMENT_3D('',#43723,#34714,#34715) ;
#29897 = AXIS2_PLACEMENT_3D('',#43724,#34716,#34717) ;
#29898 = AXIS2_PLACEMENT_3D('',#43725,#34718,#34719) ;
#29899 = AXIS2_PLACEMENT_3D('',#43728,#34721,#34722) ;
#29900 = AXIS2_PLACEMENT_3D('',#43729,#34723,#34724) ;
#29901 = AXIS2_PLACEMENT_3D('',#43730,#34725,#34726) ;
#29902 = AXIS2_PLACEMENT_3D('',#43733,#34728,#34729) ;
#29903 = AXIS2_PLACEMENT_3D('',#43734,#34730,#34731) ;
#29904 = AXIS2_PLACEMENT_3D('',#43735,#34732,#34733) ;
#29905 = AXIS2_PLACEMENT_3D('',#43738,#34735,#34736) ;
#29906 = AXIS2_PLACEMENT_3D('',#43739,#34737,#34738) ;
#29907 = AXIS2_PLACEMENT_3D('',#43740,#34739,#34740) ;
#29908 = AXIS2_PLACEMENT_3D('',#43743,#34742,#34743) ;
#29909 = AXIS2_PLACEMENT_3D('',#43744,#34744,#34745) ;
#29910 = AXIS2_PLACEMENT_3D('',#43745,#34746,#34747) ;
#29911 = AXIS2_PLACEMENT_3D('',#43748,#34749,#34750) ;
#29912 = AXIS2_PLACEMENT_3D('',#43749,#34751,#34752) ;
#29913 = AXIS2_PLACEMENT_3D('',#43750,#34753,#34754) ;
#29914 = AXIS2_PLACEMENT_3D('',#43752,#34756,#34757) ;
#29915 = AXIS2_PLACEMENT_3D('',#43753,#34758,#34759) ;
#29916 = AXIS2_PLACEMENT_3D('',#43754,#34760,#34761) ;
#29917 = AXIS2_PLACEMENT_3D('',#43755,#34762,#34763) ;
#29918 = AXIS2_PLACEMENT_3D('',#43756,#34764,#34765) ;
#29919 = AXIS2_PLACEMENT_3D('',#43757,#34766,#34767) ;
#29920 = AXIS2_PLACEMENT_3D('',#43758,#34768,#34769) ;
#29921 = AXIS2_PLACEMENT_3D('',#43759,#34770,#34771) ;
#29922 = AXIS2_PLACEMENT_3D('',#43760,#34772,#34773) ;
#29923 = AXIS2_PLACEMENT_3D('',#43762,#34774,#34775) ;
#29924 = AXIS2_PLACEMENT_3D('',#43765,#34777,#34778) ;
#29925 = AXIS2_PLACEMENT_3D('',#43766,#34779,#34780) ;
#29926 = AXIS2_PLACEMENT_3D('',#43768,#34781,#34782) ;
#29927 = AXIS2_PLACEMENT_3D('',#43771,#34784,#34785) ;
#29928 = AXIS2_PLACEMENT_3D('',#43772,#34786,#34787) ;
#29929 = AXIS2_PLACEMENT_3D('',#43774,#34788,#34789) ;
#29930 = AXIS2_PLACEMENT_3D('',#43777,#34791,#34792) ;
#29931 = AXIS2_PLACEMENT_3D('',#43778,#34793,#34794) ;
#29932 = AXIS2_PLACEMENT_3D('',#43780,#34795,#34796) ;
#29933 = AXIS2_PLACEMENT_3D('',#43783,#34798,#34799) ;
#29934 = AXIS2_PLACEMENT_3D('',#43784,#34800,#34801) ;
#29935 = AXIS2_PLACEMENT_3D('',#43786,#34802,#34803) ;
#29936 = AXIS2_PLACEMENT_3D('',#43789,#34805,#34806) ;
#29937 = AXIS2_PLACEMENT_3D('',#43790,#34807,#34808) ;
#29938 = AXIS2_PLACEMENT_3D('',#43792,#34809,#34810) ;
#29939 = AXIS2_PLACEMENT_3D('',#43795,#34812,#34813) ;
#29940 = AXIS2_PLACEMENT_3D('',#43796,#34814,#34815) ;
#29941 = AXIS2_PLACEMENT_3D('',#43801,#34817,#34818) ;
#29942 = AXIS2_PLACEMENT_3D('',#43804,#34820,#34821) ;
#29943 = AXIS2_PLACEMENT_3D('',#43805,#34822,#34823) ;
#29944 = AXIS2_PLACEMENT_3D('',#43814,#34828,#34829) ;
#29945 = AXIS2_PLACEMENT_3D('',#43821,#34834,#34835) ;
#29946 = AXIS2_PLACEMENT_3D('',#43827,#34839,#34840) ;
#29947 = AXIS2_PLACEMENT_3D('',#43829,#34842,#34843) ;
#29948 = AXIS2_PLACEMENT_3D('',#43831,#34845,#34846) ;
#29949 = AXIS2_PLACEMENT_3D('',#43833,#34848,#34849) ;
#29950 = AXIS2_PLACEMENT_3D('',#43834,#34850,#34851) ;
#29951 = AXIS2_PLACEMENT_3D('',#43836,#34852,#34853) ;
#29952 = AXIS2_PLACEMENT_3D('',#43839,#34855,#34856) ;
#29953 = AXIS2_PLACEMENT_3D('',#43840,#34857,#34858) ;
#29954 = AXIS2_PLACEMENT_3D('',#43842,#34859,#34860) ;
#29955 = AXIS2_PLACEMENT_3D('',#43845,#34862,#34863) ;
#29956 = AXIS2_PLACEMENT_3D('',#43846,#34864,#34865) ;
#29957 = AXIS2_PLACEMENT_3D('',#43851,#34867,#34868) ;
#29958 = AXIS2_PLACEMENT_3D('',#43854,#34870,#34871) ;
#29959 = AXIS2_PLACEMENT_3D('',#43855,#34872,#34873) ;
#29960 = AXIS2_PLACEMENT_3D('',#43864,#34878,#34879) ;
#29961 = AXIS2_PLACEMENT_3D('',#43871,#34884,#34885) ;
#29962 = AXIS2_PLACEMENT_3D('',#43877,#34889,#34890) ;
#29963 = AXIS2_PLACEMENT_3D('',#43879,#34892,#34893) ;
#29964 = AXIS2_PLACEMENT_3D('',#43881,#34895,#34896) ;
#29965 = AXIS2_PLACEMENT_3D('',#43883,#34898,#34899) ;
#29966 = AXIS2_PLACEMENT_3D('',#43884,#34900,#34901) ;
#29967 = AXIS2_PLACEMENT_3D('',#43886,#34902,#34903) ;
#29968 = AXIS2_PLACEMENT_3D('',#43889,#34905,#34906) ;
#29969 = AXIS2_PLACEMENT_3D('',#43890,#34907,#34908) ;
#29970 = AXIS2_PLACEMENT_3D('',#43892,#34909,#34910) ;
#29971 = AXIS2_PLACEMENT_3D('',#43895,#34912,#34913) ;
#29972 = AXIS2_PLACEMENT_3D('',#43896,#34914,#34915) ;
#29973 = AXIS2_PLACEMENT_3D('',#43898,#34916,#34917) ;
#29974 = AXIS2_PLACEMENT_3D('',#43901,#34919,#34920) ;
#29975 = AXIS2_PLACEMENT_3D('',#43902,#34921,#34922) ;
#29976 = AXIS2_PLACEMENT_3D('',#43904,#34923,#34924) ;
#29977 = AXIS2_PLACEMENT_3D('',#43907,#34926,#34927) ;
#29978 = AXIS2_PLACEMENT_3D('',#43908,#34928,#34929) ;
#29979 = AXIS2_PLACEMENT_3D('',#43909,#34930,#34931) ;
#29980 = AXIS2_PLACEMENT_3D('',#43921,#34937,#34938) ;
#29981 = AXIS2_PLACEMENT_3D('',#43922,#34939,#34940) ;
#29982 = AXIS2_PLACEMENT_3D('',#43924,#34941,#34942) ;
#29983 = AXIS2_PLACEMENT_3D('',#43927,#34944,#34945) ;
#29984 = AXIS2_PLACEMENT_3D('',#43928,#34946,#34947) ;
#29985 = AXIS2_PLACEMENT_3D('',#43930,#34948,#34949) ;
#29986 = AXIS2_PLACEMENT_3D('',#43932,#34951,#34952) ;
#29987 = AXIS2_PLACEMENT_3D('',#43933,#34953,#34954) ;
#29988 = AXIS2_PLACEMENT_3D('',#43934,#34955,#34956) ;
#29989 = AXIS2_PLACEMENT_3D('',#43943,#34961,#34962) ;
#29990 = AXIS2_PLACEMENT_3D('',#43949,#34966,#34967) ;
#29991 = AXIS2_PLACEMENT_3D('',#43955,#34971,#34972) ;
#29992 = AXIS2_PLACEMENT_3D('',#43958,#34975,#34976) ;
#29993 = AXIS2_PLACEMENT_3D('',#43967,#34981,#34982) ;
#29994 = AXIS2_PLACEMENT_3D('',#43973,#34986,#34987) ;
#29995 = AXIS2_PLACEMENT_3D('',#43979,#34991,#34992) ;
#29996 = AXIS2_PLACEMENT_3D('',#43987,#34997,#34998) ;
#29997 = AXIS2_PLACEMENT_3D('',#43988,#34999,#35000) ;
#29998 = AXIS2_PLACEMENT_3D('',#43997,#35005,#35006) ;
#29999 = AXIS2_PLACEMENT_3D('',#43999,#35007,#35008) ;
#30000 = AXIS2_PLACEMENT_3D('',#44000,#35009,#35010) ;
#30001 = AXIS2_PLACEMENT_3D('',#44009,#35015,#35016) ;
#30002 = AXIS2_PLACEMENT_3D('',#44011,#35017,#35018) ;
#30003 = AXIS2_PLACEMENT_3D('',#44024,#35026,#35027) ;
#30004 = AXIS2_PLACEMENT_3D('',#44038,#35035,#35036) ;
#30005 = AXIS2_PLACEMENT_3D('',#44040,#35038,#35039) ;
#30006 = AXIS2_PLACEMENT_3D('',#44044,#35041,#35042) ;
#30007 = AXIS2_PLACEMENT_3D('',#44048,#35045,#35046) ;
#30008 = AXIS2_PLACEMENT_3D('',#44053,#35049,#35050) ;
#30009 = AXIS2_PLACEMENT_3D('',#44054,#35051,#35052) ;
#30010 = AXIS2_PLACEMENT_3D('',#44060,#35056,#35057) ;
#30011 = AXIS2_PLACEMENT_3D('',#44069,#35062,#35063) ;
#30012 = AXIS2_PLACEMENT_3D('',#44078,#35068,#35069) ;
#30013 = AXIS2_PLACEMENT_3D('',#44087,#35074,#35075) ;
#30014 = AXIS2_PLACEMENT_3D('',#44093,#35079,#35080) ;
#30015 = AXIS2_PLACEMENT_3D('',#44101,#35084,#35085) ;
#30016 = AXIS2_PLACEMENT_3D('',#44102,#35086,#35087) ;
#30017 = AXIS2_PLACEMENT_3D('',#44108,#35091,#35092) ;
#30018 = AXIS2_PLACEMENT_3D('',#44109,#35093,#35094) ;
#30019 = AXIS2_PLACEMENT_3D('',#44150,#35117,#35118) ;
#30020 = AXIS2_PLACEMENT_3D('',#44152,#35119,#35120) ;
#30021 = AXIS2_PLACEMENT_3D('',#44156,#35123,#35124) ;
#30022 = AXIS2_PLACEMENT_3D('',#44160,#35127,#35128) ;
#30023 = AXIS2_PLACEMENT_3D('',#44164,#35131,#35132) ;
#30024 = AXIS2_PLACEMENT_3D('',#44170,#35136,#35137) ;
#30025 = AXIS2_PLACEMENT_3D('',#44174,#35140,#35141) ;
#30026 = AXIS2_PLACEMENT_3D('',#44180,#35145,#35146) ;
#30027 = AXIS2_PLACEMENT_3D('',#44184,#35149,#35150) ;
#30028 = AXIS2_PLACEMENT_3D('',#44189,#35154,#35155) ;
#30029 = AXIS2_PLACEMENT_3D('',#44193,#35158,#35159) ;
#30030 = AXIS2_PLACEMENT_3D('',#44195,#35160,#35161) ;
#30031 = AXIS2_PLACEMENT_3D('',#44196,#35162,#35163) ;
#30032 = AXIS2_PLACEMENT_3D('',#44198,#35164,#35165) ;
#30033 = AXIS2_PLACEMENT_3D('',#44199,#35166,#35167) ;
#30034 = AXIS2_PLACEMENT_3D('',#44206,#35172,#35173) ;
#30035 = AXIS2_PLACEMENT_3D('',#44212,#35177,#35178) ;
#30036 = AXIS2_PLACEMENT_3D('',#44215,#35181,#35182) ;
#30037 = AXIS2_PLACEMENT_3D('',#44217,#35184,#35185) ;
#30038 = AXIS2_PLACEMENT_3D('',#44218,#35186,#35187) ;
#30039 = AXIS2_PLACEMENT_3D('',#44220,#35189,#35190) ;
#30040 = AXIS2_PLACEMENT_3D('',#44221,#35191,#35192) ;
#30041 = AXIS2_PLACEMENT_3D('',#44223,#35194,#35195) ;
#30042 = AXIS2_PLACEMENT_3D('',#44224,#35196,#35197) ;
#30043 = AXIS2_PLACEMENT_3D('',#44226,#35198,#35199) ;
#30044 = AXIS2_PLACEMENT_3D('',#44228,#35200,#35201) ;
#30045 = AXIS2_PLACEMENT_3D('',#44229,#35202,#35203) ;
#30046 = AXIS2_PLACEMENT_3D('',#44231,#35204,#35205) ;
#30047 = AXIS2_PLACEMENT_3D('',#44233,#35206,#35207) ;
#30048 = AXIS2_PLACEMENT_3D('',#44234,#35208,#35209) ;
#30049 = AXIS2_PLACEMENT_3D('',#44236,#35211,#35212) ;
#30050 = AXIS2_PLACEMENT_3D('',#44238,#35214,#35215) ;
#30051 = AXIS2_PLACEMENT_3D('',#44240,#35217,#35218) ;
#30052 = AXIS2_PLACEMENT_3D('',#44242,#35220,#35221) ;
#30053 = AXIS2_PLACEMENT_3D('',#44248,#35225,#35226) ;
#30054 = AXIS2_PLACEMENT_3D('',#44257,#35231,#35232) ;
#30055 = AXIS2_PLACEMENT_3D('',#44266,#35237,#35238) ;
#30056 = AXIS2_PLACEMENT_3D('',#44269,#35241,#35242) ;
#30057 = AXIS2_PLACEMENT_3D('',#44275,#35246,#35247) ;
#30058 = AXIS2_PLACEMENT_3D('',#44278,#35250,#35251) ;
#30059 = AXIS2_PLACEMENT_3D('',#44280,#35253,#35254) ;
#30060 = AXIS2_PLACEMENT_3D('',#44282,#35256,#35257) ;
#30061 = AXIS2_PLACEMENT_3D('',#44291,#35262,#35263) ;
#30062 = AXIS2_PLACEMENT_3D('',#44294,#35266,#35267) ;
#30063 = AXIS2_PLACEMENT_3D('',#44296,#35269,#35270) ;
#30064 = AXIS2_PLACEMENT_3D('',#44298,#35272,#35273) ;
#30065 = AXIS2_PLACEMENT_3D('',#44307,#35278,#35279) ;
#30066 = AXIS2_PLACEMENT_3D('',#44310,#35282,#35283) ;
#30067 = AXIS2_PLACEMENT_3D('',#44312,#35285,#35286) ;
#30068 = AXIS2_PLACEMENT_3D('',#44314,#35288,#35289) ;
#30069 = AXIS2_PLACEMENT_3D('',#44315,#35290,#35291) ;
#30070 = AXIS2_PLACEMENT_3D('',#44317,#35292,#35293) ;
#30071 = AXIS2_PLACEMENT_3D('',#44318,#35294,#35295) ;
#30072 = AXIS2_PLACEMENT_3D('',#44320,#35296,#35297) ;
#30073 = AXIS2_PLACEMENT_3D('',#44322,#35298,#35299) ;
#30074 = AXIS2_PLACEMENT_3D('',#44323,#35300,#35301) ;
#30075 = AXIS2_PLACEMENT_3D('',#44326,#35303,#35304) ;
#30076 = AXIS2_PLACEMENT_3D('',#44327,#35305,#35306) ;
#30077 = AXIS2_PLACEMENT_3D('',#44329,#35308,#35309) ;
#30078 = AXIS2_PLACEMENT_3D('',#44331,#35310,#35311) ;
#30079 = AXIS2_PLACEMENT_3D('',#44332,#35312,#35313) ;
#30080 = AXIS2_PLACEMENT_3D('',#44334,#35314,#35315) ;
#30081 = AXIS2_PLACEMENT_3D('',#44336,#35316,#35317) ;
#30082 = AXIS2_PLACEMENT_3D('',#44337,#35318,#35319) ;
#30083 = AXIS2_PLACEMENT_3D('',#44339,#35321,#35322) ;
#30084 = AXIS2_PLACEMENT_3D('',#44341,#35324,#35325) ;
#30085 = AXIS2_PLACEMENT_3D('',#44345,#35327,#35328) ;
#30086 = AXIS2_PLACEMENT_3D('',#44346,#35329,#35330) ;
#30087 = AXIS2_PLACEMENT_3D('',#44347,#35331,#35332) ;
#30088 = AXIS2_PLACEMENT_3D('',#44348,#35333,#35334) ;
#30089 = AXIS2_PLACEMENT_3D('',#44350,#35336,#35337) ;
#30090 = AXIS2_PLACEMENT_3D('',#44352,#35339,#35340) ;
#30091 = AXIS2_PLACEMENT_3D('',#44354,#35342,#35343) ;
#30092 = AXIS2_PLACEMENT_3D('',#44360,#35347,#35348) ;
#30093 = AXIS2_PLACEMENT_3D('',#44363,#35351,#35352) ;
#30094 = AXIS2_PLACEMENT_3D('',#44364,#35353,#35354) ;
#30095 = AXIS2_PLACEMENT_3D('',#44365,#35355,#35356) ;
#30096 = AXIS2_PLACEMENT_3D('',#44367,#35358,#35359) ;
#30097 = AXIS2_PLACEMENT_3D('',#44369,#35361,#35362) ;
#30098 = AXIS2_PLACEMENT_3D('',#44373,#35365,#35366) ;
#30099 = AXIS2_PLACEMENT_3D('',#44379,#35370,#35371) ;
#30100 = AXIS2_PLACEMENT_3D('',#44388,#35376,#35377) ;
#30101 = AXIS2_PLACEMENT_3D('',#44397,#35382,#35383) ;
#30102 = AXIS2_PLACEMENT_3D('',#44401,#35387,#35388) ;
#30103 = AXIS2_PLACEMENT_3D('',#44403,#35390,#35391) ;
#30104 = AXIS2_PLACEMENT_3D('',#44405,#35393,#35394) ;
#30105 = AXIS2_PLACEMENT_3D('',#44407,#35396,#35397) ;
#30106 = AXIS2_PLACEMENT_3D('',#44408,#35398,#35399) ;
#30107 = AXIS2_PLACEMENT_3D('',#44411,#35400,#35401) ;
#30108 = AXIS2_PLACEMENT_3D('',#44415,#35403,#35404) ;
#30109 = AXIS2_PLACEMENT_3D('',#44417,#35406,#35407) ;
#30110 = AXIS2_PLACEMENT_3D('',#44423,#35411,#35412) ;
#30111 = AXIS2_PLACEMENT_3D('',#44427,#35415,#35416) ;
#30112 = AXIS2_PLACEMENT_3D('',#44431,#35419,#35420) ;
#30113 = AXIS2_PLACEMENT_3D('',#44433,#35422,#35423) ;
#30114 = AXIS2_PLACEMENT_3D('',#44434,#35424,#35425) ;
#30115 = AXIS2_PLACEMENT_3D('',#44443,#35430,#35431) ;
#30116 = AXIS2_PLACEMENT_3D('',#44446,#35432,#35433) ;
#30117 = AXIS2_PLACEMENT_3D('',#44449,#35436,#35437) ;
#30118 = AXIS2_PLACEMENT_3D('',#44453,#35440,#35441) ;
#30119 = AXIS2_PLACEMENT_3D('',#44455,#35442,#35443) ;
#30120 = AXIS2_PLACEMENT_3D('',#44457,#35445,#35446) ;
#30121 = AXIS2_PLACEMENT_3D('',#44459,#35448,#35449) ;
#30122 = AXIS2_PLACEMENT_3D('',#44460,#35450,#35451) ;
#30123 = AXIS2_PLACEMENT_3D('',#44463,#35452,#35453) ;
#30124 = AXIS2_PLACEMENT_3D('',#44465,#35455,#35456) ;
#30125 = AXIS2_PLACEMENT_3D('',#44468,#35457,#35458) ;
#30126 = AXIS2_PLACEMENT_3D('',#44470,#35460,#35461) ;
#30127 = AXIS2_PLACEMENT_3D('',#44473,#35464,#35465) ;
#30128 = AXIS2_PLACEMENT_3D('',#44474,#35466,#35467) ;
#30129 = AXIS2_PLACEMENT_3D('',#44483,#35472,#35473) ;
#30130 = AXIS2_PLACEMENT_3D('',#44489,#35477,#35478) ;
#30131 = AXIS2_PLACEMENT_3D('',#44490,#35479,#35480) ;
#30132 = AXIS2_PLACEMENT_3D('',#44491,#35481,#35482) ;
#30133 = AXIS2_PLACEMENT_3D('',#44492,#35483,#35484) ;
#30134 = AXIS2_PLACEMENT_3D('',#44493,#35485,#35486) ;
#30135 = AXIS2_PLACEMENT_3D('',#44494,#35487,#35488) ;
#30136 = AXIS2_PLACEMENT_3D('',#44499,#35490,#35491) ;
#30137 = AXIS2_PLACEMENT_3D('',#44501,#35493,#35494) ;
#30138 = AXIS2_PLACEMENT_3D('',#44507,#35498,#35499) ;
#30139 = AXIS2_PLACEMENT_3D('',#44510,#35501,#35502) ;
#30140 = AXIS2_PLACEMENT_3D('',#44511,#35503,#35504) ;
#30141 = AXIS2_PLACEMENT_3D('',#44513,#35506,#35507) ;
#30142 = AXIS2_PLACEMENT_3D('',#44514,#35508,#35509) ;
#30143 = AXIS2_PLACEMENT_3D('',#44523,#35514,#35515) ;
#30144 = AXIS2_PLACEMENT_3D('',#44529,#35519,#35520) ;
#30145 = AXIS2_PLACEMENT_3D('',#44530,#35521,#35522) ;
#30146 = AXIS2_PLACEMENT_3D('',#44531,#35523,#35524) ;
#30147 = AXIS2_PLACEMENT_3D('',#44532,#35525,#35526) ;
#30148 = AXIS2_PLACEMENT_3D('',#44533,#35527,#35528) ;
#30149 = AXIS2_PLACEMENT_3D('',#44534,#35529,#35530) ;
#30150 = AXIS2_PLACEMENT_3D('',#44540,#35533,#35534) ;
#30151 = AXIS2_PLACEMENT_3D('',#44541,#35535,#35536) ;
#30152 = AXIS2_PLACEMENT_3D('',#44546,#35538,#35539) ;
#30153 = AXIS2_PLACEMENT_3D('',#44548,#35541,#35542) ;
#30154 = AXIS2_PLACEMENT_3D('',#44551,#35545,#35546) ;
#30155 = AXIS2_PLACEMENT_3D('',#44553,#35548,#35549) ;
#30156 = AXIS2_PLACEMENT_3D('',#44554,#35550,#35551) ;
#30157 = AXIS2_PLACEMENT_3D('',#44563,#35556,#35557) ;
#30158 = AXIS2_PLACEMENT_3D('',#44565,#35558,#35559) ;
#30159 = AXIS2_PLACEMENT_3D('',#44568,#35561,#35562) ;
#30160 = AXIS2_PLACEMENT_3D('',#44569,#35563,#35564) ;
#30161 = AXIS2_PLACEMENT_3D('',#44571,#35566,#35567) ;
#30162 = AXIS2_PLACEMENT_3D('',#44573,#35569,#35570) ;
#30163 = AXIS2_PLACEMENT_3D('',#44574,#35571,#35572) ;
#30164 = AXIS2_PLACEMENT_3D('',#44580,#35575,#35576) ;
#30165 = AXIS2_PLACEMENT_3D('',#44581,#35577,#35578) ;
#30166 = AXIS2_PLACEMENT_3D('',#44586,#35580,#35581) ;
#30167 = AXIS2_PLACEMENT_3D('',#44588,#35583,#35584) ;
#30168 = AXIS2_PLACEMENT_3D('',#44591,#35587,#35588) ;
#30169 = AXIS2_PLACEMENT_3D('',#44593,#35590,#35591) ;
#30170 = AXIS2_PLACEMENT_3D('',#44594,#35592,#35593) ;
#30171 = AXIS2_PLACEMENT_3D('',#44603,#35598,#35599) ;
#30172 = AXIS2_PLACEMENT_3D('',#44604,#35600,#35601) ;
#30173 = AXIS2_PLACEMENT_3D('',#44605,#35602,#35603) ;
#30174 = AXIS2_PLACEMENT_3D('',#44606,#35604,#35605) ;
#30175 = AXIS2_PLACEMENT_3D('',#44607,#35606,#35607) ;
#30176 = AXIS2_PLACEMENT_3D('',#44608,#35608,#35609) ;
#30177 = AXIS2_PLACEMENT_3D('',#44613,#35611,#35612) ;
#30178 = AXIS2_PLACEMENT_3D('',#44616,#35614,#35615) ;
#30179 = AXIS2_PLACEMENT_3D('',#44617,#35616,#35617) ;
#30180 = AXIS2_PLACEMENT_3D('',#44619,#35619,#35620) ;
#30181 = AXIS2_PLACEMENT_3D('',#44621,#35622,#35623) ;
#30182 = AXIS2_PLACEMENT_3D('',#44622,#35624,#35625) ;
#30183 = AXIS2_PLACEMENT_3D('',#44631,#35630,#35631) ;
#30184 = AXIS2_PLACEMENT_3D('',#44632,#35632,#35633) ;
#30185 = AXIS2_PLACEMENT_3D('',#44633,#35634,#35635) ;
#30186 = AXIS2_PLACEMENT_3D('',#44634,#35636,#35637) ;
#30187 = AXIS2_PLACEMENT_3D('',#44635,#35638,#35639) ;
#30188 = AXIS2_PLACEMENT_3D('',#44636,#35640,#35641) ;
#30189 = AXIS2_PLACEMENT_3D('',#44641,#35643,#35644) ;
#30190 = AXIS2_PLACEMENT_3D('',#44644,#35646,#35647) ;
#30191 = AXIS2_PLACEMENT_3D('',#44645,#35648,#35649) ;
#30192 = AXIS2_PLACEMENT_3D('',#44647,#35651,#35652) ;
#30193 = AXIS2_PLACEMENT_3D('',#44649,#35654,#35655) ;
#30194 = AXIS2_PLACEMENT_3D('',#44650,#35656,#35657) ;
#30195 = AXIS2_PLACEMENT_3D('',#44659,#35662,#35663) ;
#30196 = AXIS2_PLACEMENT_3D('',#44660,#35664,#35665) ;
#30197 = AXIS2_PLACEMENT_3D('',#44661,#35666,#35667) ;
#30198 = AXIS2_PLACEMENT_3D('',#44662,#35668,#35669) ;
#30199 = AXIS2_PLACEMENT_3D('',#44663,#35670,#35671) ;
#30200 = AXIS2_PLACEMENT_3D('',#44664,#35672,#35673) ;
#30201 = AXIS2_PLACEMENT_3D('',#44673,#35678,#35679) ;
#30202 = AXIS2_PLACEMENT_3D('',#44679,#35683,#35684) ;
#30203 = AXIS2_PLACEMENT_3D('',#44685,#35688,#35689) ;
#30204 = AXIS2_PLACEMENT_3D('',#44688,#35692,#35693) ;
#30205 = AXIS2_PLACEMENT_3D('',#44689,#35694,#35695) ;
#30206 = AXIS2_PLACEMENT_3D('',#44690,#35696,#35697) ;
#30207 = AXIS2_PLACEMENT_3D('',#44699,#35702,#35703) ;
#30208 = AXIS2_PLACEMENT_3D('',#44708,#35708,#35709) ;
#30209 = AXIS2_PLACEMENT_3D('',#44711,#35712,#35713) ;
#30210 = AXIS2_PLACEMENT_3D('',#44713,#35715,#35716) ;
#30211 = AXIS2_PLACEMENT_3D('',#44715,#35718,#35719) ;
#30212 = AXIS2_PLACEMENT_3D('',#44716,#35720,#35721) ;
#30213 = AXIS2_PLACEMENT_3D('',#44725,#35726,#35727) ;
#30214 = AXIS2_PLACEMENT_3D('',#44731,#35731,#35732) ;
#30215 = AXIS2_PLACEMENT_3D('',#44737,#35736,#35737) ;
#30216 = AXIS2_PLACEMENT_3D('',#44755,#35747,#35748) ;
#30217 = AXIS2_PLACEMENT_3D('',#44759,#35751,#35752) ;
#30218 = AXIS2_PLACEMENT_3D('',#44763,#35755,#35756) ;
#30219 = AXIS2_PLACEMENT_3D('',#44777,#35764,#35765) ;
#30220 = AXIS2_PLACEMENT_3D('',#44780,#35768,#35769) ;
#30221 = AXIS2_PLACEMENT_3D('',#44781,#35770,#35771) ;
#30222 = AXIS2_PLACEMENT_3D('',#44783,#35773,#35774) ;
#30223 = AXIS2_PLACEMENT_3D('',#44785,#35776,#35777) ;
#30224 = AXIS2_PLACEMENT_3D('',#44787,#35779,#35780) ;
#30225 = AXIS2_PLACEMENT_3D('',#44789,#35782,#35783) ;
#30226 = AXIS2_PLACEMENT_3D('',#44790,#35784,#35785) ;
#30227 = AXIS2_PLACEMENT_3D('',#44795,#35787,#35788) ;
#30228 = AXIS2_PLACEMENT_3D('',#44798,#35790,#35791) ;
#30229 = AXIS2_PLACEMENT_3D('',#44799,#35792,#35793) ;
#30230 = AXIS2_PLACEMENT_3D('',#44802,#35796,#35797) ;
#30231 = AXIS2_PLACEMENT_3D('',#44803,#35798,#35799) ;
#30232 = AXIS2_PLACEMENT_3D('',#44804,#35800,#35801) ;
#30233 = AXIS2_PLACEMENT_3D('',#44807,#35802,#35803) ;
#30234 = AXIS2_PLACEMENT_3D('',#44809,#35805,#35806) ;
#30235 = AXIS2_PLACEMENT_3D('',#44815,#35810,#35811) ;
#30236 = AXIS2_PLACEMENT_3D('',#44817,#35812,#35813) ;
#30237 = AXIS2_PLACEMENT_3D('',#44821,#35815,#35816) ;
#30238 = AXIS2_PLACEMENT_3D('',#44825,#35818,#35819) ;
#30239 = AXIS2_PLACEMENT_3D('',#44829,#35821,#35822) ;
#30240 = AXIS2_PLACEMENT_3D('',#44832,#35824,#35825) ;
#30241 = AXIS2_PLACEMENT_3D('',#44833,#35826,#35827) ;
#30242 = AXIS2_PLACEMENT_3D('',#44835,#35829,#35830) ;
#30243 = AXIS2_PLACEMENT_3D('',#44837,#35832,#35833) ;
#30244 = AXIS2_PLACEMENT_3D('',#44839,#35835,#35836) ;
#30245 = AXIS2_PLACEMENT_3D('',#44841,#35838,#35839) ;
#30246 = AXIS2_PLACEMENT_3D('',#44842,#35840,#35841) ;
#30247 = AXIS2_PLACEMENT_3D('',#44843,#35842,#35843) ;
#30248 = AXIS2_PLACEMENT_3D('',#44852,#35848,#35849) ;
#30249 = AXIS2_PLACEMENT_3D('',#44861,#35854,#35855) ;
#30250 = AXIS2_PLACEMENT_3D('',#44864,#35858,#35859) ;
#30251 = AXIS2_PLACEMENT_3D('',#44866,#35861,#35862) ;
#30252 = AXIS2_PLACEMENT_3D('',#44868,#35864,#35865) ;
#30253 = AXIS2_PLACEMENT_3D('',#44869,#35866,#35867) ;
#30254 = AXIS2_PLACEMENT_3D('',#44870,#35868,#35869) ;
#30255 = AXIS2_PLACEMENT_3D('',#44948,#35871,#35872) ;
#30256 = AXIS2_PLACEMENT_3D('',#44950,#35873,#35874) ;
#30257 = AXIS2_PLACEMENT_3D('',#44952,#35875,#35876) ;
#30258 = AXIS2_PLACEMENT_3D('',#44953,#35877,#35878) ;
#30259 = AXIS2_PLACEMENT_3D('',#44956,#35880,#35881) ;
#30260 = AXIS2_PLACEMENT_3D('',#44957,#35882,#35883) ;
#30261 = AXIS2_PLACEMENT_3D('',#44958,#35884,#35885) ;
#30262 = AXIS2_PLACEMENT_3D('',#44960,#35886,#35887) ;
#30263 = AXIS2_PLACEMENT_3D('',#44962,#35889,#35890) ;
#30264 = AXIS2_PLACEMENT_3D('',#44963,#35891,#35892) ;
#30265 = AXIS2_PLACEMENT_3D('',#44964,#35893,#35894) ;
#30266 = AXIS2_PLACEMENT_3D('',#45042,#35896,#35897) ;
#30267 = AXIS2_PLACEMENT_3D('',#45044,#35898,#35899) ;
#30268 = AXIS2_PLACEMENT_3D('',#45046,#35900,#35901) ;
#30269 = AXIS2_PLACEMENT_3D('',#45047,#35902,#35903) ;
#30270 = AXIS2_PLACEMENT_3D('',#45050,#35905,#35906) ;
#30271 = AXIS2_PLACEMENT_3D('',#45051,#35907,#35908) ;
#30272 = AXIS2_PLACEMENT_3D('',#45052,#35909,#35910) ;
#30273 = AXIS2_PLACEMENT_3D('',#45054,#35911,#35912) ;
#30274 = AXIS2_PLACEMENT_3D('',#45056,#35914,#35915) ;
#30275 = AXIS2_PLACEMENT_3D('',#45057,#35916,#35917) ;
#30276 = AXIS2_PLACEMENT_3D('',#45058,#35918,#35919) ;
#30277 = AXIS2_PLACEMENT_3D('',#45059,#35920,#35921) ;
#30278 = AXIS2_PLACEMENT_3D('',#45060,#35922,#35923) ;
#30279 = AXIS2_PLACEMENT_3D('',#45061,#35924,#35925) ;
#30280 = AXIS2_PLACEMENT_3D('',#45062,#35926,#35927) ;
#30281 = AXIS2_PLACEMENT_3D('',#45063,#35928,#35929) ;
#30282 = AXIS2_PLACEMENT_3D('',#45064,#35930,#35931) ;
#30283 = AXIS2_PLACEMENT_3D('',#45065,#35932,#35933) ;
#30284 = AXIS2_PLACEMENT_3D('',#45066,#35934,#35935) ;
#30285 = AXIS2_PLACEMENT_3D('',#45067,#35936,#35937) ;
#30286 = AXIS2_PLACEMENT_3D('',#45069,#35938,#35939) ;
#30287 = AXIS2_PLACEMENT_3D('',#45072,#35941,#35942) ;
#30288 = AXIS2_PLACEMENT_3D('',#45073,#35943,#35944) ;
#30289 = AXIS2_PLACEMENT_3D('',#45075,#35945,#35946) ;
#30290 = AXIS2_PLACEMENT_3D('',#45078,#35948,#35949) ;
#30291 = AXIS2_PLACEMENT_3D('',#45079,#35950,#35951) ;
#30292 = AXIS2_PLACEMENT_3D('',#45081,#35952,#35953) ;
#30293 = AXIS2_PLACEMENT_3D('',#45084,#35955,#35956) ;
#30294 = AXIS2_PLACEMENT_3D('',#45085,#35957,#35958) ;
#30295 = AXIS2_PLACEMENT_3D('',#45087,#35959,#35960) ;
#30296 = AXIS2_PLACEMENT_3D('',#45090,#35962,#35963) ;
#30297 = AXIS2_PLACEMENT_3D('',#45091,#35964,#35965) ;
#30298 = AXIS2_PLACEMENT_3D('',#45096,#35967,#35968) ;
#30299 = AXIS2_PLACEMENT_3D('',#45099,#35970,#35971) ;
#30300 = AXIS2_PLACEMENT_3D('',#45100,#35972,#35973) ;
#30301 = AXIS2_PLACEMENT_3D('',#45102,#35975,#35976) ;
#30302 = AXIS2_PLACEMENT_3D('',#45108,#35979,#35980) ;
#30303 = AXIS2_PLACEMENT_3D('',#45110,#35981,#35982) ;
#30304 = AXIS2_PLACEMENT_3D('',#45112,#35983,#35984) ;
#30305 = AXIS2_PLACEMENT_3D('',#45114,#35985,#35986) ;
#30306 = AXIS2_PLACEMENT_3D('',#45115,#35987,#35988) ;
#30307 = AXIS2_PLACEMENT_3D('',#45121,#35991,#35992) ;
#30308 = AXIS2_PLACEMENT_3D('',#45125,#35994,#35995) ;
#30309 = AXIS2_PLACEMENT_3D('',#45133,#35999,#36000) ;
#30310 = AXIS2_PLACEMENT_3D('',#45135,#36002,#36003) ;
#30311 = AXIS2_PLACEMENT_3D('',#45139,#36005,#36006) ;
#30312 = AXIS2_PLACEMENT_3D('',#45140,#36007,#36008) ;
#30313 = AXIS2_PLACEMENT_3D('',#45143,#36011,#36012) ;
#30314 = AXIS2_PLACEMENT_3D('',#45166,#36024,#36025) ;
#30315 = AXIS2_PLACEMENT_3D('',#45167,#36026,#36027) ;
#30316 = AXIS2_PLACEMENT_3D('',#45171,#36029,#36030) ;
#30317 = AXIS2_PLACEMENT_3D('',#45172,#36031,#36032) ;
#30318 = AXIS2_PLACEMENT_3D('',#45175,#36035,#36036) ;
#30319 = AXIS2_PLACEMENT_3D('',#45203,#36051,#36052) ;
#30320 = AXIS2_PLACEMENT_3D('',#45204,#36053,#36054) ;
#30321 = AXIS2_PLACEMENT_3D('',#45205,#36055,#36056) ;
#30322 = AXIS2_PLACEMENT_3D('',#45206,#36057,#36058) ;
#30323 = AXIS2_PLACEMENT_3D('',#45207,#36059,#36060) ;
#30324 = AXIS2_PLACEMENT_3D('',#45209,#36061,#36062) ;
#30325 = AXIS2_PLACEMENT_3D('',#45212,#36064,#36065) ;
#30326 = AXIS2_PLACEMENT_3D('',#45213,#36066,#36067) ;
#30327 = AXIS2_PLACEMENT_3D('',#45214,#36068,#36069) ;
#30328 = AXIS2_PLACEMENT_3D('',#45216,#36070,#36071) ;
#30329 = AXIS2_PLACEMENT_3D('',#45218,#36073,#36074) ;
#30330 = AXIS2_PLACEMENT_3D('',#45219,#36075,#36076) ;
#30331 = AXIS2_PLACEMENT_3D('',#45224,#36078,#36079) ;
#30332 = AXIS2_PLACEMENT_3D('',#45227,#36081,#36082) ;
#30333 = AXIS2_PLACEMENT_3D('',#45228,#36083,#36084) ;
#30334 = AXIS2_PLACEMENT_3D('',#45233,#36086,#36087) ;
#30335 = AXIS2_PLACEMENT_3D('',#45236,#36089,#36090) ;
#30336 = AXIS2_PLACEMENT_3D('',#45237,#36091,#36092) ;
#30337 = AXIS2_PLACEMENT_3D('',#45247,#36098,#36099) ;
#30338 = AXIS2_PLACEMENT_3D('',#45251,#36102,#36103) ;
#30339 = AXIS2_PLACEMENT_3D('',#45255,#36106,#36107) ;
#30340 = AXIS2_PLACEMENT_3D('',#45265,#36113,#36114) ;
#30341 = AXIS2_PLACEMENT_3D('',#45269,#36117,#36118) ;
#30342 = AXIS2_PLACEMENT_3D('',#45273,#36121,#36122) ;
#30343 = AXIS2_PLACEMENT_3D('',#45277,#36125,#36126) ;
#30344 = AXIS2_PLACEMENT_3D('',#45281,#36129,#36130) ;
#30345 = AXIS2_PLACEMENT_3D('',#45283,#36132,#36133) ;
#30346 = AXIS2_PLACEMENT_3D('',#45287,#36136,#36137) ;
#30347 = AXIS2_PLACEMENT_3D('',#45291,#36140,#36141) ;
#30348 = AXIS2_PLACEMENT_3D('',#45293,#36143,#36144) ;
#30349 = AXIS2_PLACEMENT_3D('',#45296,#36145,#36146) ;
#30350 = AXIS2_PLACEMENT_3D('',#45297,#36147,#36148) ;
#30351 = AXIS2_PLACEMENT_3D('',#45298,#36149,#36150) ;
#30352 = AXIS2_PLACEMENT_3D('',#45300,#36151,#36152) ;
#30353 = AXIS2_PLACEMENT_3D('',#45304,#36156,#36157) ;
#30354 = AXIS2_PLACEMENT_3D('',#45306,#36158,#36159) ;
#30355 = AXIS2_PLACEMENT_3D('',#45308,#36161,#36162) ;
#30356 = AXIS2_PLACEMENT_3D('',#45310,#36163,#36164) ;
#30357 = AXIS2_PLACEMENT_3D('',#45313,#36166,#36167) ;
#30358 = AXIS2_PLACEMENT_3D('',#45314,#36168,#36169) ;
#30359 = AXIS2_PLACEMENT_3D('',#45315,#36170,#36171) ;
#30360 = AXIS2_PLACEMENT_3D('',#45316,#36172,#36173) ;
#30361 = AXIS2_PLACEMENT_3D('',#45318,#36174,#36175) ;
#30362 = AXIS2_PLACEMENT_3D('',#45321,#36177,#36178) ;
#30363 = AXIS2_PLACEMENT_3D('',#45322,#36179,#36180) ;
#30364 = AXIS2_PLACEMENT_3D('',#45323,#36181,#36182) ;
#30365 = AXIS2_PLACEMENT_3D('',#45325,#36183,#36184) ;
#30366 = AXIS2_PLACEMENT_3D('',#45328,#36186,#36187) ;
#30367 = AXIS2_PLACEMENT_3D('',#45329,#36188,#36189) ;
#30368 = AXIS2_PLACEMENT_3D('',#45330,#36190,#36191) ;
#30369 = AXIS2_PLACEMENT_3D('',#45332,#36192,#36193) ;
#30370 = AXIS2_PLACEMENT_3D('',#45335,#36195,#36196) ;
#30371 = AXIS2_PLACEMENT_3D('',#45336,#36197,#36198) ;
#30372 = AXIS2_PLACEMENT_3D('',#45337,#36199,#36200) ;
#30373 = AXIS2_PLACEMENT_3D('',#45340,#36202,#36203) ;
#30374 = AXIS2_PLACEMENT_3D('',#45341,#36204,#36205) ;
#30375 = AXIS2_PLACEMENT_3D('',#45342,#36206,#36207) ;
#30376 = AXIS2_PLACEMENT_3D('',#45348,#36211,#36212) ;
#30377 = AXIS2_PLACEMENT_3D('',#45354,#36216,#36217) ;
#30378 = AXIS2_PLACEMENT_3D('',#45356,#36219,#36220) ;
#30379 = AXIS2_PLACEMENT_3D('',#45358,#36222,#36223) ;
#30380 = AXIS2_PLACEMENT_3D('',#45365,#36228,#36229) ;
#30381 = AXIS2_PLACEMENT_3D('',#45371,#36233,#36234) ;
#30382 = AXIS2_PLACEMENT_3D('',#45377,#36238,#36239) ;
#30383 = AXIS2_PLACEMENT_3D('',#45379,#36241,#36242) ;
#30384 = AXIS2_PLACEMENT_3D('',#45381,#36244,#36245) ;
#30385 = AXIS2_PLACEMENT_3D('',#45385,#36248,#36249) ;
#30386 = AXIS2_PLACEMENT_3D('',#45389,#36252,#36253) ;
#30387 = AXIS2_PLACEMENT_3D('',#45391,#36255,#36256) ;
#30388 = AXIS2_PLACEMENT_3D('',#45392,#36257,#36258) ;
#30389 = AXIS2_PLACEMENT_3D('',#45398,#36262,#36263) ;
#30390 = AXIS2_PLACEMENT_3D('',#45404,#36267,#36268) ;
#30391 = AXIS2_PLACEMENT_3D('',#45407,#36271,#36272) ;
#30392 = AXIS2_PLACEMENT_3D('',#45408,#36273,#36274) ;
#30393 = AXIS2_PLACEMENT_3D('',#45410,#36276,#36277) ;
#30394 = AXIS2_PLACEMENT_3D('',#45411,#36278,#36279) ;
#30395 = AXIS2_PLACEMENT_3D('',#45412,#36280,#36281) ;
#30396 = AXIS2_PLACEMENT_3D('',#45414,#36282,#36283) ;
#30397 = AXIS2_PLACEMENT_3D('',#45417,#36285,#36286) ;
#30398 = AXIS2_PLACEMENT_3D('',#45418,#36287,#36288) ;
#30399 = AXIS2_PLACEMENT_3D('',#45419,#36289,#36290) ;
#30400 = AXIS2_PLACEMENT_3D('',#45428,#36295,#36296) ;
#30401 = AXIS2_PLACEMENT_3D('',#45437,#36301,#36302) ;
#30402 = AXIS2_PLACEMENT_3D('',#45444,#36307,#36308) ;
#30403 = AXIS2_PLACEMENT_3D('',#45448,#36311,#36312) ;
#30404 = AXIS2_PLACEMENT_3D('',#45452,#36315,#36316) ;
#30405 = AXIS2_PLACEMENT_3D('',#45454,#36318,#36319) ;
#30406 = AXIS2_PLACEMENT_3D('',#45456,#36321,#36322) ;
#30407 = AXIS2_PLACEMENT_3D('',#45457,#36323,#36324) ;
#30408 = AXIS2_PLACEMENT_3D('',#45458,#36325,#36326) ;
#30409 = AXIS2_PLACEMENT_3D('',#45463,#36328,#36329) ;
#30410 = AXIS2_PLACEMENT_3D('',#45468,#36332,#36333) ;
#30411 = AXIS2_PLACEMENT_3D('',#45469,#36334,#36335) ;
#30412 = AXIS2_PLACEMENT_3D('',#45474,#36337,#36338) ;
#30413 = AXIS2_PLACEMENT_3D('',#45479,#36341,#36342) ;
#30414 = AXIS2_PLACEMENT_3D('',#45480,#36343,#36344) ;
#30415 = AXIS2_PLACEMENT_3D('',#45485,#36346,#36347) ;
#30416 = AXIS2_PLACEMENT_3D('',#45488,#36349,#36350) ;
#30417 = AXIS2_PLACEMENT_3D('',#45489,#36351,#36352) ;
#30418 = AXIS2_PLACEMENT_3D('',#45494,#36354,#36355) ;
#30419 = AXIS2_PLACEMENT_3D('',#45498,#36357,#36358) ;
#30420 = AXIS2_PLACEMENT_3D('',#45500,#36360,#36361) ;
#30421 = AXIS2_PLACEMENT_3D('',#45505,#36363,#36364) ;
#30422 = AXIS2_PLACEMENT_3D('',#45510,#36367,#36368) ;
#30423 = AXIS2_PLACEMENT_3D('',#45511,#36369,#36370) ;
#30424 = AXIS2_PLACEMENT_3D('',#45516,#36372,#36373) ;
#30425 = AXIS2_PLACEMENT_3D('',#45519,#36375,#36376) ;
#30426 = AXIS2_PLACEMENT_3D('',#45520,#36377,#36378) ;
#30427 = AXIS2_PLACEMENT_3D('',#45524,#36380,#36381) ;
#30428 = AXIS2_PLACEMENT_3D('',#45526,#36383,#36384) ;
#30429 = AXIS2_PLACEMENT_3D('',#45530,#36386,#36387) ;
#30430 = AXIS2_PLACEMENT_3D('',#45532,#36389,#36390) ;
#30431 = AXIS2_PLACEMENT_3D('',#45537,#36393,#36394) ;
#30432 = AXIS2_PLACEMENT_3D('',#45538,#36395,#36396) ;
#30433 = AXIS2_PLACEMENT_3D('',#45542,#36398,#36399) ;
#30434 = AXIS2_PLACEMENT_3D('',#45544,#36401,#36402) ;
#30435 = AXIS2_PLACEMENT_3D('',#45548,#36404,#36405) ;
#30436 = AXIS2_PLACEMENT_3D('',#45550,#36407,#36408) ;
#30437 = AXIS2_PLACEMENT_3D('',#45554,#36410,#36411) ;
#30438 = AXIS2_PLACEMENT_3D('',#45556,#36413,#36414) ;
#30439 = AXIS2_PLACEMENT_3D('',#45563,#36418,#36419) ;
#30440 = AXIS2_PLACEMENT_3D('',#45564,#36420,#36421) ;
#30441 = AXIS2_PLACEMENT_3D('',#45568,#36423,#36424) ;
#30442 = AXIS2_PLACEMENT_3D('',#45570,#36425,#36426) ;
#30443 = AXIS2_PLACEMENT_3D('',#45572,#36428,#36429) ;
#30444 = AXIS2_PLACEMENT_3D('',#45578,#36432,#36433) ;
#30445 = AXIS2_PLACEMENT_3D('',#45580,#36435,#36436) ;
#30446 = AXIS2_PLACEMENT_3D('',#45584,#36438,#36439) ;
#30447 = AXIS2_PLACEMENT_3D('',#45588,#36442,#36443) ;
#30448 = AXIS2_PLACEMENT_3D('',#45592,#36445,#36446) ;
#30449 = AXIS2_PLACEMENT_3D('',#45596,#36449,#36450) ;
#30450 = AXIS2_PLACEMENT_3D('',#45600,#36452,#36453) ;
#30451 = AXIS2_PLACEMENT_3D('',#45602,#36455,#36456) ;
#30452 = AXIS2_PLACEMENT_3D('',#45612,#36462,#36463) ;
#30453 = AXIS2_PLACEMENT_3D('',#45622,#36469,#36470) ;
#30454 = AXIS2_PLACEMENT_3D('',#45628,#36474,#36475) ;
#30455 = AXIS2_PLACEMENT_3D('',#45635,#36480,#36481) ;
#30456 = AXIS2_PLACEMENT_3D('',#45639,#36484,#36485) ;
#30457 = AXIS2_PLACEMENT_3D('',#45643,#36488,#36489) ;
#30458 = AXIS2_PLACEMENT_3D('',#45653,#36495,#36496) ;
#30459 = AXIS2_PLACEMENT_3D('',#45659,#36500,#36501) ;
#30460 = AXIS2_PLACEMENT_3D('',#45669,#36507,#36508) ;
#30461 = AXIS2_PLACEMENT_3D('',#45675,#36512,#36513) ;
#30462 = AXIS2_PLACEMENT_3D('',#45681,#36517,#36518) ;
#30463 = AXIS2_PLACEMENT_3D('',#45691,#36524,#36525) ;
#30464 = AXIS2_PLACEMENT_3D('',#45693,#36526,#36527) ;
#30465 = AXIS2_PLACEMENT_3D('',#45695,#36529,#36530) ;
#30466 = AXIS2_PLACEMENT_3D('',#45696,#36531,#36532) ;
#30467 = AXIS2_PLACEMENT_3D('',#45697,#36533,#36534) ;
#30468 = AXIS2_PLACEMENT_3D('',#45699,#36535,#36536) ;
#30469 = AXIS2_PLACEMENT_3D('',#45701,#36538,#36539) ;
#30470 = AXIS2_PLACEMENT_3D('',#45703,#36540,#36541) ;
#30471 = AXIS2_PLACEMENT_3D('',#45705,#36543,#36544) ;
#30472 = AXIS2_PLACEMENT_3D('',#45706,#36545,#36546) ;
#30473 = AXIS2_PLACEMENT_3D('',#45707,#36547,#36548) ;
#30474 = AXIS2_PLACEMENT_3D('',#45710,#36550,#36551) ;
#30475 = AXIS2_PLACEMENT_3D('',#45711,#36552,#36553) ;
#30476 = AXIS2_PLACEMENT_3D('',#45712,#36554,#36555) ;
#30477 = AXIS2_PLACEMENT_3D('',#45713,#36556,#36557) ;
#30478 = AXIS2_PLACEMENT_3D('',#45727,#36567,#36568) ;
#30479 = AXIS2_PLACEMENT_3D('',#45733,#36572,#36573) ;
#30480 = AXIS2_PLACEMENT_3D('',#45735,#36575,#36576) ;
#30481 = AXIS2_PLACEMENT_3D('',#45737,#36578,#36579) ;
#30482 = AXIS2_PLACEMENT_3D('',#45738,#36580,#36581) ;
#30483 = AXIS2_PLACEMENT_3D('',#45739,#36582,#36583) ;
#30484 = AXIS2_PLACEMENT_3D('',#45740,#36584,#36585) ;
#30485 = AXIS2_PLACEMENT_3D('',#45742,#36587,#36588) ;
#30486 = AXIS2_PLACEMENT_3D('',#45743,#36589,#36590) ;
#30487 = AXIS2_PLACEMENT_3D('',#45745,#36591,#36592) ;
#30488 = AXIS2_PLACEMENT_3D('',#45750,#36595,#36596) ;
#30489 = AXIS2_PLACEMENT_3D('',#45754,#36599,#36600) ;
#30490 = AXIS2_PLACEMENT_3D('',#45755,#36601,#36602) ;
#30491 = AXIS2_PLACEMENT_3D('',#45756,#36603,#36604) ;
#30492 = AXIS2_PLACEMENT_3D('',#45760,#36607,#36608) ;
#30493 = AXIS2_PLACEMENT_3D('',#45764,#36611,#36612) ;
#30494 = AXIS2_PLACEMENT_3D('',#45766,#36614,#36615) ;
#30495 = AXIS2_PLACEMENT_3D('',#45767,#36616,#36617) ;
#30496 = AXIS2_PLACEMENT_3D('',#45769,#36619,#36620) ;
#30497 = AXIS2_PLACEMENT_3D('',#45770,#36621,#36622) ;
#30498 = AXIS2_PLACEMENT_3D('',#45774,#36625,#36626) ;
#30499 = AXIS2_PLACEMENT_3D('',#45776,#36628,#36629) ;
#30500 = AXIS2_PLACEMENT_3D('',#45777,#36630,#36631) ;
#30501 = AXIS2_PLACEMENT_3D('',#45779,#36632,#36633) ;
#30502 = AXIS2_PLACEMENT_3D('',#45782,#36635,#36636) ;
#30503 = AXIS2_PLACEMENT_3D('',#45783,#36637,#36638) ;
#30504 = AXIS2_PLACEMENT_3D('',#45784,#36639,#36640) ;
#30505 = AXIS2_PLACEMENT_3D('',#45786,#36641,#36642) ;
#30506 = AXIS2_PLACEMENT_3D('',#45787,#36643,#36644) ;
#30507 = AXIS2_PLACEMENT_3D('',#45789,#36645,#36646) ;
#30508 = AXIS2_PLACEMENT_3D('',#45791,#36648,#36649) ;
#30509 = AXIS2_PLACEMENT_3D('',#45792,#36650,#36651) ;
#30510 = AXIS2_PLACEMENT_3D('',#45793,#36652,#36653) ;
#30511 = AXIS2_PLACEMENT_3D('',#45795,#36654,#36655) ;
#30512 = AXIS2_PLACEMENT_3D('',#45798,#36657,#36658) ;
#30513 = AXIS2_PLACEMENT_3D('',#45799,#36659,#36660) ;
#30514 = AXIS2_PLACEMENT_3D('',#45801,#36661,#36662) ;
#30515 = AXIS2_PLACEMENT_3D('',#45804,#36664,#36665) ;
#30516 = AXIS2_PLACEMENT_3D('',#45805,#36666,#36667) ;
#30517 = AXIS2_PLACEMENT_3D('',#45806,#36668,#36669) ;
#30518 = AXIS2_PLACEMENT_3D('',#45807,#36670,#36671) ;
#30519 = AXIS2_PLACEMENT_3D('',#45808,#36672,#36673) ;
#30520 = AXIS2_PLACEMENT_3D('',#45811,#36674,#36675) ;
#30521 = AXIS2_PLACEMENT_3D('',#45815,#36677,#36678) ;
#30522 = AXIS2_PLACEMENT_3D('',#45817,#36680,#36681) ;
#30523 = AXIS2_PLACEMENT_3D('',#45827,#36687,#36688) ;
#30524 = AXIS2_PLACEMENT_3D('',#45833,#36692,#36693) ;
#30525 = AXIS2_PLACEMENT_3D('',#45840,#36698,#36699) ;
#30526 = AXIS2_PLACEMENT_3D('',#45842,#36700,#36701) ;
#30527 = AXIS2_PLACEMENT_3D('',#45846,#36703,#36704) ;
#30528 = AXIS2_PLACEMENT_3D('',#45849,#36706,#36707) ;
#30529 = AXIS2_PLACEMENT_3D('',#45850,#36708,#36709) ;
#30530 = AXIS2_PLACEMENT_3D('',#45854,#36711,#36712) ;
#30531 = AXIS2_PLACEMENT_3D('',#45856,#36714,#36715) ;
#30532 = AXIS2_PLACEMENT_3D('',#45861,#36719,#36720) ;
#30533 = AXIS2_PLACEMENT_3D('',#45869,#36725,#36726) ;
#30534 = AXIS2_PLACEMENT_3D('',#45875,#36730,#36731) ;
#30535 = AXIS2_PLACEMENT_3D('',#45878,#36734,#36735) ;
#30536 = AXIS2_PLACEMENT_3D('',#45879,#36736,#36737) ;
#30537 = AXIS2_PLACEMENT_3D('',#45881,#36739,#36740) ;
#30538 = AXIS2_PLACEMENT_3D('',#45883,#36742,#36743) ;
#30539 = AXIS2_PLACEMENT_3D('',#45884,#36744,#36745) ;
#30540 = AXIS2_PLACEMENT_3D('',#45885,#36746,#36747) ;
#30541 = AXIS2_PLACEMENT_3D('',#45887,#36748,#36749) ;
#30542 = AXIS2_PLACEMENT_3D('',#45890,#36751,#36752) ;
#30543 = AXIS2_PLACEMENT_3D('',#45891,#36753,#36754) ;
#30544 = AXIS2_PLACEMENT_3D('',#45892,#36755,#36756) ;
#30545 = AXIS2_PLACEMENT_3D('',#45893,#36757,#36758) ;
#30546 = AXIS2_PLACEMENT_3D('',#45894,#36759,#36760) ;
#30547 = AXIS2_PLACEMENT_3D('',#45896,#36761,#36762) ;
#30548 = AXIS2_PLACEMENT_3D('',#45899,#36764,#36765) ;
#30549 = AXIS2_PLACEMENT_3D('',#45900,#36766,#36767) ;
#30550 = AXIS2_PLACEMENT_3D('',#45901,#36768,#36769) ;
#30551 = AXIS2_PLACEMENT_3D('',#45903,#36770,#36771) ;
#30552 = AXIS2_PLACEMENT_3D('',#45906,#36773,#36774) ;
#30553 = AXIS2_PLACEMENT_3D('',#45907,#36775,#36776) ;
#30554 = AXIS2_PLACEMENT_3D('',#45909,#36777,#36778) ;
#30555 = AXIS2_PLACEMENT_3D('',#45912,#36780,#36781) ;
#30556 = AXIS2_PLACEMENT_3D('',#45913,#36782,#36783) ;
#30557 = AXIS2_PLACEMENT_3D('',#45914,#36784,#36785) ;
#30558 = AXIS2_PLACEMENT_3D('',#45915,#36786,#36787) ;
#30559 = AXIS2_PLACEMENT_3D('',#45916,#36788,#36789) ;
#30560 = AXIS2_PLACEMENT_3D('',#45918,#36790,#36791) ;
#30561 = AXIS2_PLACEMENT_3D('',#45921,#36793,#36794) ;
#30562 = AXIS2_PLACEMENT_3D('',#45922,#36795,#36796) ;
#30563 = AXIS2_PLACEMENT_3D('',#45924,#36797,#36798) ;
#30564 = AXIS2_PLACEMENT_3D('',#45927,#36800,#36801) ;
#30565 = AXIS2_PLACEMENT_3D('',#45928,#36802,#36803) ;
#30566 = AXIS2_PLACEMENT_3D('',#45929,#36804,#36805) ;
#30567 = AXIS2_PLACEMENT_3D('',#45930,#36806,#36807) ;
#30568 = AXIS2_PLACEMENT_3D('',#45932,#36808,#36809) ;
#30569 = AXIS2_PLACEMENT_3D('',#45935,#36811,#36812) ;
#30570 = AXIS2_PLACEMENT_3D('',#45936,#36813,#36814) ;
#30571 = AXIS2_PLACEMENT_3D('',#45938,#36815,#36816) ;
#30572 = AXIS2_PLACEMENT_3D('',#45941,#36818,#36819) ;
#30573 = AXIS2_PLACEMENT_3D('',#45942,#36820,#36821) ;
#30574 = AXIS2_PLACEMENT_3D('',#45943,#36822,#36823) ;
#30575 = AXIS2_PLACEMENT_3D('',#45944,#36824,#36825) ;
#30576 = AXIS2_PLACEMENT_3D('',#45946,#36826,#36827) ;
#30577 = AXIS2_PLACEMENT_3D('',#45949,#36829,#36830) ;
#30578 = AXIS2_PLACEMENT_3D('',#45950,#36831,#36832) ;
#30579 = AXIS2_PLACEMENT_3D('',#45951,#36833,#36834) ;
#30580 = AXIS2_PLACEMENT_3D('',#45952,#36835,#36836) ;
#30581 = AXIS2_PLACEMENT_3D('',#45953,#36837,#36838) ;
#30582 = AXIS2_PLACEMENT_3D('',#45955,#36839,#36840) ;
#30583 = AXIS2_PLACEMENT_3D('',#45957,#36841,#36842) ;
#30584 = AXIS2_PLACEMENT_3D('',#45958,#36843,#36844) ;
#30585 = AXIS2_PLACEMENT_3D('',#45960,#36845,#36846) ;
#30586 = AXIS2_PLACEMENT_3D('',#45962,#36847,#36848) ;
#30587 = AXIS2_PLACEMENT_3D('',#45963,#36849,#36850) ;
#30588 = AXIS2_PLACEMENT_3D('',#45965,#36852,#36853) ;
#30589 = AXIS2_PLACEMENT_3D('',#45967,#36854,#36855) ;
#30590 = AXIS2_PLACEMENT_3D('',#45971,#36857,#36858) ;
#30591 = AXIS2_PLACEMENT_3D('',#45975,#36860,#36861) ;
#30592 = AXIS2_PLACEMENT_3D('',#45979,#36863,#36864) ;
#30593 = AXIS2_PLACEMENT_3D('',#45983,#36866,#36867) ;
#30594 = AXIS2_PLACEMENT_3D('',#45986,#36869,#36870) ;
#30595 = AXIS2_PLACEMENT_3D('',#45989,#36872,#36873) ;
#30596 = AXIS2_PLACEMENT_3D('',#45991,#36874,#36875) ;
#30597 = AXIS2_PLACEMENT_3D('',#45994,#36877,#36878) ;
#30598 = AXIS2_PLACEMENT_3D('',#45999,#36880,#36881) ;
#30599 = AXIS2_PLACEMENT_3D('',#46002,#36883,#36884) ;
#30600 = AXIS2_PLACEMENT_3D('',#46007,#36886,#36887) ;
#30601 = AXIS2_PLACEMENT_3D('',#46010,#36889,#36890) ;
#30602 = AXIS2_PLACEMENT_3D('',#46015,#36892,#36893) ;
#30603 = AXIS2_PLACEMENT_3D('',#46018,#36895,#36896) ;
#30604 = AXIS2_PLACEMENT_3D('',#46023,#36898,#36899) ;
#30605 = AXIS2_PLACEMENT_3D('',#46026,#36901,#36902) ;
#30606 = AXIS2_PLACEMENT_3D('',#46031,#36904,#36905) ;
#30607 = AXIS2_PLACEMENT_3D('',#46034,#36907,#36908) ;
#30608 = AXIS2_PLACEMENT_3D('',#46039,#36910,#36911) ;
#30609 = AXIS2_PLACEMENT_3D('',#46042,#36913,#36914) ;
#30610 = AXIS2_PLACEMENT_3D('',#46043,#36915,#36916) ;
#30611 = AXIS2_PLACEMENT_3D('',#46049,#36920,#36921) ;
#30612 = AXIS2_PLACEMENT_3D('',#46053,#36924,#36925) ;
#30613 = AXIS2_PLACEMENT_3D('',#46057,#36928,#36929) ;
#30614 = AXIS2_PLACEMENT_3D('',#46063,#36933,#36934) ;
#30615 = AXIS2_PLACEMENT_3D('',#46065,#36936,#36937) ;
#30616 = AXIS2_PLACEMENT_3D('',#46069,#36940,#36941) ;
#30617 = AXIS2_PLACEMENT_3D('',#46073,#36944,#36945) ;
#30618 = AXIS2_PLACEMENT_3D('',#46074,#36946,#36947) ;
#30619 = AXIS2_PLACEMENT_3D('',#46076,#36949,#36950) ;
#30620 = AXIS2_PLACEMENT_3D('',#46077,#36951,#36952) ;
#30621 = AXIS2_PLACEMENT_3D('',#46083,#36956,#36957) ;
#30622 = AXIS2_PLACEMENT_3D('',#46087,#36960,#36961) ;
#30623 = AXIS2_PLACEMENT_3D('',#46091,#36964,#36965) ;
#30624 = AXIS2_PLACEMENT_3D('',#46097,#36969,#36970) ;
#30625 = AXIS2_PLACEMENT_3D('',#46099,#36972,#36973) ;
#30626 = AXIS2_PLACEMENT_3D('',#46103,#36976,#36977) ;
#30627 = AXIS2_PLACEMENT_3D('',#46107,#36980,#36981) ;
#30628 = AXIS2_PLACEMENT_3D('',#46109,#36983,#36984) ;
#30629 = AXIS2_PLACEMENT_3D('',#46110,#36985,#36986) ;
#30630 = AXIS2_PLACEMENT_3D('',#46111,#36987,#36988) ;
#30631 = AXIS2_PLACEMENT_3D('',#46117,#36992,#36993) ;
#30632 = AXIS2_PLACEMENT_3D('',#46121,#36996,#36997) ;
#30633 = AXIS2_PLACEMENT_3D('',#46125,#37000,#37001) ;
#30634 = AXIS2_PLACEMENT_3D('',#46131,#37005,#37006) ;
#30635 = AXIS2_PLACEMENT_3D('',#46133,#37008,#37009) ;
#30636 = AXIS2_PLACEMENT_3D('',#46137,#37012,#37013) ;
#30637 = AXIS2_PLACEMENT_3D('',#46141,#37016,#37017) ;
#30638 = AXIS2_PLACEMENT_3D('',#46142,#37018,#37019) ;
#30639 = AXIS2_PLACEMENT_3D('',#46144,#37021,#37022) ;
#30640 = AXIS2_PLACEMENT_3D('',#46145,#37023,#37024) ;
#30641 = AXIS2_PLACEMENT_3D('',#46151,#37028,#37029) ;
#30642 = AXIS2_PLACEMENT_3D('',#46155,#37032,#37033) ;
#30643 = AXIS2_PLACEMENT_3D('',#46159,#37036,#37037) ;
#30644 = AXIS2_PLACEMENT_3D('',#46165,#37041,#37042) ;
#30645 = AXIS2_PLACEMENT_3D('',#46167,#37044,#37045) ;
#30646 = AXIS2_PLACEMENT_3D('',#46171,#37048,#37049) ;
#30647 = AXIS2_PLACEMENT_3D('',#46175,#37052,#37053) ;
#30648 = AXIS2_PLACEMENT_3D('',#46177,#37055,#37056) ;
#30649 = AXIS2_PLACEMENT_3D('',#46178,#37057,#37058) ;
#30650 = AXIS2_PLACEMENT_3D('',#46179,#37059,#37060) ;
#30651 = AXIS2_PLACEMENT_3D('',#46182,#37062,#37063) ;
#30652 = AXIS2_PLACEMENT_3D('',#46183,#37064,#37065) ;
#30653 = AXIS2_PLACEMENT_3D('',#46184,#37066,#37067) ;
#30654 = AXIS2_PLACEMENT_3D('',#46185,#37068,#37069) ;
#30655 = AXIS2_PLACEMENT_3D('',#46186,#37070,#37071) ;
#30656 = AXIS2_PLACEMENT_3D('',#46188,#37072,#37073) ;
#30657 = AXIS2_PLACEMENT_3D('',#46191,#37075,#37076) ;
#30658 = AXIS2_PLACEMENT_3D('',#46192,#37077,#37078) ;
#30659 = AXIS2_PLACEMENT_3D('',#46194,#37079,#37080) ;
#30660 = AXIS2_PLACEMENT_3D('',#46197,#37082,#37083) ;
#30661 = AXIS2_PLACEMENT_3D('',#46198,#37084,#37085) ;
#30662 = AXIS2_PLACEMENT_3D('',#46199,#37086,#37087) ;
#30663 = AXIS2_PLACEMENT_3D('',#46200,#37088,#37089) ;
#30664 = AXIS2_PLACEMENT_3D('',#46201,#37090,#37091) ;
#30665 = AXIS2_PLACEMENT_3D('',#46202,#37092,#37093) ;
#30666 = AXIS2_PLACEMENT_3D('',#46203,#37094,#37095) ;
#30667 = AXIS2_PLACEMENT_3D('',#46204,#37096,#37097) ;
#30668 = AXIS2_PLACEMENT_3D('',#46205,#37098,#37099) ;
#30669 = AXIS2_PLACEMENT_3D('',#46206,#37100,#37101) ;
#30670 = AXIS2_PLACEMENT_3D('',#46207,#37102,#37103) ;
#30671 = AXIS2_PLACEMENT_3D('',#46208,#37104,#37105) ;
#30672 = AXIS2_PLACEMENT_3D('',#46209,#37106,#37107) ;
#30673 = AXIS2_PLACEMENT_3D('',#46210,#37108,#37109) ;
#30674 = AXIS2_PLACEMENT_3D('',#46211,#37110,#37111) ;
#30675 = AXIS2_PLACEMENT_3D('',#46212,#37112,#37113) ;
#30676 = AXIS2_PLACEMENT_3D('',#46214,#37114,#37115) ;
#30677 = AXIS2_PLACEMENT_3D('',#46217,#37117,#37118) ;
#30678 = AXIS2_PLACEMENT_3D('',#46218,#37119,#37120) ;
#30679 = AXIS2_PLACEMENT_3D('',#46227,#37125,#37126) ;
#30680 = AXIS2_PLACEMENT_3D('',#46233,#37130,#37131) ;
#30681 = AXIS2_PLACEMENT_3D('',#46241,#37136,#37137) ;
#30682 = AXIS2_PLACEMENT_3D('',#46247,#37141,#37142) ;
#30683 = AXIS2_PLACEMENT_3D('',#46249,#37144,#37145) ;
#30684 = AXIS2_PLACEMENT_3D('',#46253,#37148,#37149) ;
#30685 = AXIS2_PLACEMENT_3D('',#46255,#37151,#37152) ;
#30686 = AXIS2_PLACEMENT_3D('',#46257,#37153,#37154) ;
#30687 = AXIS2_PLACEMENT_3D('',#46260,#37156,#37157) ;
#30688 = AXIS2_PLACEMENT_3D('',#46261,#37158,#37159) ;
#30689 = AXIS2_PLACEMENT_3D('',#46270,#37164,#37165) ;
#30690 = AXIS2_PLACEMENT_3D('',#46276,#37169,#37170) ;
#30691 = AXIS2_PLACEMENT_3D('',#46280,#37173,#37174) ;
#30692 = AXIS2_PLACEMENT_3D('',#46284,#37177,#37178) ;
#30693 = AXIS2_PLACEMENT_3D('',#46286,#37180,#37181) ;
#30694 = AXIS2_PLACEMENT_3D('',#46288,#37182,#37183) ;
#30695 = AXIS2_PLACEMENT_3D('',#46291,#37185,#37186) ;
#30696 = AXIS2_PLACEMENT_3D('',#46292,#37187,#37188) ;
#30697 = AXIS2_PLACEMENT_3D('',#46294,#37189,#37190) ;
#30698 = AXIS2_PLACEMENT_3D('',#46297,#37192,#37193) ;
#30699 = AXIS2_PLACEMENT_3D('',#46298,#37194,#37195) ;
#30700 = AXIS2_PLACEMENT_3D('',#46300,#37196,#37197) ;
#30701 = AXIS2_PLACEMENT_3D('',#46303,#37199,#37200) ;
#30702 = AXIS2_PLACEMENT_3D('',#46304,#37201,#37202) ;
#30703 = AXIS2_PLACEMENT_3D('',#46306,#37203,#37204) ;
#30704 = AXIS2_PLACEMENT_3D('',#46309,#37206,#37207) ;
#30705 = AXIS2_PLACEMENT_3D('',#46310,#37208,#37209) ;
#30706 = AXIS2_PLACEMENT_3D('',#46312,#37210,#37211) ;
#30707 = AXIS2_PLACEMENT_3D('',#46316,#37213,#37214) ;
#30708 = AXIS2_PLACEMENT_3D('',#46320,#37216,#37217) ;
#30709 = AXIS2_PLACEMENT_3D('',#46323,#37219,#37220) ;
#30710 = AXIS2_PLACEMENT_3D('',#46324,#37221,#37222) ;
#30711 = AXIS2_PLACEMENT_3D('',#46340,#37230,#37231) ;
#30712 = AXIS2_PLACEMENT_3D('',#46342,#37232,#37233) ;
#30713 = AXIS2_PLACEMENT_3D('',#46344,#37234,#37235) ;
#30714 = AXIS2_PLACEMENT_3D('',#46358,#37243,#37244) ;
#30715 = AXIS2_PLACEMENT_3D('',#46362,#37247,#37248) ;
#30716 = AXIS2_PLACEMENT_3D('',#46365,#37249,#37250) ;
#30717 = AXIS2_PLACEMENT_3D('',#46375,#37256,#37257) ;
#30718 = AXIS2_PLACEMENT_3D('',#46378,#37260,#37261) ;
#30719 = AXIS2_PLACEMENT_3D('',#46380,#37263,#37264) ;
#30720 = AXIS2_PLACEMENT_3D('',#46383,#37267,#37268) ;
#30721 = AXIS2_PLACEMENT_3D('',#46385,#37270,#37271) ;
#30722 = AXIS2_PLACEMENT_3D('',#46393,#37276,#37277) ;
#30723 = AXIS2_PLACEMENT_3D('',#46395,#37279,#37280) ;
#30724 = AXIS2_PLACEMENT_3D('',#46397,#37282,#37283) ;
#30725 = AXIS2_PLACEMENT_3D('',#46399,#37285,#37286) ;
#30726 = AXIS2_PLACEMENT_3D('',#46403,#37288,#37289) ;
#30727 = AXIS2_PLACEMENT_3D('',#46405,#37291,#37292) ;
#30728 = AXIS2_PLACEMENT_3D('',#46414,#37297,#37298) ;
#30729 = AXIS2_PLACEMENT_3D('',#46415,#37299,#37300) ;
#30730 = AXIS2_PLACEMENT_3D('',#46416,#37301,#37302) ;
#30731 = AXIS2_PLACEMENT_3D('',#46419,#37305,#37306) ;
#30732 = AXIS2_PLACEMENT_3D('',#46421,#37308,#37309) ;
#30733 = AXIS2_PLACEMENT_3D('',#46423,#37311,#37312) ;
#30734 = AXIS2_PLACEMENT_3D('',#46424,#37313,#37314) ;
#30735 = AXIS2_PLACEMENT_3D('',#46425,#37315,#37316) ;
#30736 = AXIS2_PLACEMENT_3D('',#46434,#37321,#37322) ;
#30737 = AXIS2_PLACEMENT_3D('',#46440,#37326,#37327) ;
#30738 = AXIS2_PLACEMENT_3D('',#46448,#37332,#37333) ;
#30739 = AXIS2_PLACEMENT_3D('',#46456,#37338,#37339) ;
#30740 = AXIS2_PLACEMENT_3D('',#46461,#37343,#37344) ;
#30741 = AXIS2_PLACEMENT_3D('',#46465,#37347,#37348) ;
#30742 = AXIS2_PLACEMENT_3D('',#46466,#37349,#37350) ;
#30743 = AXIS2_PLACEMENT_3D('',#46468,#37351,#37352) ;
#30744 = AXIS2_PLACEMENT_3D('',#46471,#37354,#37355) ;
#30745 = AXIS2_PLACEMENT_3D('',#46472,#37356,#37357) ;
#30746 = AXIS2_PLACEMENT_3D('',#46481,#37362,#37363) ;
#30747 = AXIS2_PLACEMENT_3D('',#46490,#37368,#37369) ;
#30748 = AXIS2_PLACEMENT_3D('',#46493,#37372,#37373) ;
#30749 = AXIS2_PLACEMENT_3D('',#46499,#37377,#37378) ;
#30750 = AXIS2_PLACEMENT_3D('',#46504,#37382,#37383) ;
#30751 = AXIS2_PLACEMENT_3D('',#46506,#37384,#37385) ;
#30752 = AXIS2_PLACEMENT_3D('',#46509,#37387,#37388) ;
#30753 = AXIS2_PLACEMENT_3D('',#46510,#37389,#37390) ;
#30754 = AXIS2_PLACEMENT_3D('',#46519,#37395,#37396) ;
#30755 = AXIS2_PLACEMENT_3D('',#46525,#37400,#37401) ;
#30756 = AXIS2_PLACEMENT_3D('',#46531,#37405,#37406) ;
#30757 = AXIS2_PLACEMENT_3D('',#46537,#37410,#37411) ;
#30758 = AXIS2_PLACEMENT_3D('',#46543,#37415,#37416) ;
#30759 = AXIS2_PLACEMENT_3D('',#46545,#37417,#37418) ;
#30760 = AXIS2_PLACEMENT_3D('',#46548,#37420,#37421) ;
#30761 = AXIS2_PLACEMENT_3D('',#46549,#37422,#37423) ;
#30762 = AXIS2_PLACEMENT_3D('',#46552,#37426,#37427) ;
#30763 = AXIS2_PLACEMENT_3D('',#46555,#37430,#37431) ;
#30764 = AXIS2_PLACEMENT_3D('',#46556,#37432,#37433) ;
#30765 = AXIS2_PLACEMENT_3D('',#46557,#37434,#37435) ;
#30766 = AXIS2_PLACEMENT_3D('',#46558,#37436,#37437) ;
#30767 = AXIS2_PLACEMENT_3D('',#46567,#37442,#37443) ;
#30768 = AXIS2_PLACEMENT_3D('',#46573,#37447,#37448) ;
#30769 = AXIS2_PLACEMENT_3D('',#46577,#37451,#37452) ;
#30770 = AXIS2_PLACEMENT_3D('',#46581,#37455,#37456) ;
#30771 = AXIS2_PLACEMENT_3D('',#46655,#37494,#37495) ;
#30772 = AXIS2_PLACEMENT_3D('',#46664,#37500,#37501) ;
#30773 = AXIS2_PLACEMENT_3D('',#46667,#37504,#37505) ;
#30774 = AXIS2_PLACEMENT_3D('',#46669,#37507,#37508) ;
#30775 = AXIS2_PLACEMENT_3D('',#46671,#37510,#37511) ;
#30776 = AXIS2_PLACEMENT_3D('',#46712,#37536,#37537) ;
#30777 = AXIS2_PLACEMENT_3D('',#46718,#37541,#37542) ;
#30778 = AXIS2_PLACEMENT_3D('',#46720,#37544,#37545) ;
#30779 = AXIS2_PLACEMENT_3D('',#46722,#37547,#37548) ;
#30780 = AXIS2_PLACEMENT_3D('',#46723,#37549,#37550) ;
#30781 = AXIS2_PLACEMENT_3D('',#46729,#37554,#37555) ;
#30782 = AXIS2_PLACEMENT_3D('',#46731,#37557,#37558) ;
#30783 = AXIS2_PLACEMENT_3D('',#46733,#37560,#37561) ;
#30784 = AXIS2_PLACEMENT_3D('',#46734,#37562,#37563) ;
#30785 = AXIS2_PLACEMENT_3D('',#46740,#37567,#37568) ;
#30786 = AXIS2_PLACEMENT_3D('',#46742,#37570,#37571) ;
#30787 = AXIS2_PLACEMENT_3D('',#46744,#37573,#37574) ;
#30788 = AXIS2_PLACEMENT_3D('',#46745,#37575,#37576) ;
#30789 = AXIS2_PLACEMENT_3D('',#46751,#37580,#37581) ;
#30790 = AXIS2_PLACEMENT_3D('',#46753,#37583,#37584) ;
#30791 = AXIS2_PLACEMENT_3D('',#46755,#37586,#37587) ;
#30792 = AXIS2_PLACEMENT_3D('',#46756,#37588,#37589) ;
#30793 = AXIS2_PLACEMENT_3D('',#46762,#37593,#37594) ;
#30794 = AXIS2_PLACEMENT_3D('',#46764,#37596,#37597) ;
#30795 = AXIS2_PLACEMENT_3D('',#46766,#37599,#37600) ;
#30796 = AXIS2_PLACEMENT_3D('',#46767,#37601,#37602) ;
#30797 = AXIS2_PLACEMENT_3D('',#46773,#37606,#37607) ;
#30798 = AXIS2_PLACEMENT_3D('',#46775,#37609,#37610) ;
#30799 = AXIS2_PLACEMENT_3D('',#46777,#37612,#37613) ;
#30800 = AXIS2_PLACEMENT_3D('',#46778,#37614,#37615) ;
#30801 = AXIS2_PLACEMENT_3D('',#46784,#37619,#37620) ;
#30802 = AXIS2_PLACEMENT_3D('',#46786,#37622,#37623) ;
#30803 = AXIS2_PLACEMENT_3D('',#46788,#37625,#37626) ;
#30804 = AXIS2_PLACEMENT_3D('',#46789,#37627,#37628) ;
#30805 = AXIS2_PLACEMENT_3D('',#46795,#37632,#37633) ;
#30806 = AXIS2_PLACEMENT_3D('',#46797,#37635,#37636) ;
#30807 = AXIS2_PLACEMENT_3D('',#46799,#37638,#37639) ;
#30808 = AXIS2_PLACEMENT_3D('',#46800,#37640,#37641) ;
#30809 = AXIS2_PLACEMENT_3D('',#46801,#37642,#37643) ;
#30810 = AXIS2_PLACEMENT_3D('',#46803,#37644,#37645) ;
#30811 = AXIS2_PLACEMENT_3D('',#46806,#37647,#37648) ;
#30812 = AXIS2_PLACEMENT_3D('',#46807,#37649,#37650) ;
#30813 = AXIS2_PLACEMENT_3D('',#46809,#37651,#37652) ;
#30814 = AXIS2_PLACEMENT_3D('',#46812,#37654,#37655) ;
#30815 = AXIS2_PLACEMENT_3D('',#46813,#37656,#37657) ;
#30816 = AXIS2_PLACEMENT_3D('',#46815,#37658,#37659) ;
#30817 = AXIS2_PLACEMENT_3D('',#46818,#37661,#37662) ;
#30818 = AXIS2_PLACEMENT_3D('',#46819,#37663,#37664) ;
#30819 = AXIS2_PLACEMENT_3D('',#46821,#37665,#37666) ;
#30820 = AXIS2_PLACEMENT_3D('',#46824,#37668,#37669) ;
#30821 = AXIS2_PLACEMENT_3D('',#46825,#37670,#37671) ;
#30822 = AXIS2_PLACEMENT_3D('',#46830,#37673,#37674) ;
#30823 = AXIS2_PLACEMENT_3D('',#46882,#37676,#37677) ;
#30824 = AXIS2_PLACEMENT_3D('',#46926,#37678,#37679) ;
#30825 = AXIS2_PLACEMENT_3D('',#46935,#37684,#37685) ;
#30826 = AXIS2_PLACEMENT_3D('',#46936,#37686,#37687) ;
#30827 = AXIS2_PLACEMENT_3D('',#46938,#37688,#37689) ;
#30828 = AXIS2_PLACEMENT_3D('',#46939,#37690,#37691) ;
#30829 = AXIS2_PLACEMENT_3D('',#46940,#37692,#37693) ;
#30830 = AXIS2_PLACEMENT_3D('',#46942,#37694,#37695) ;
#30831 = AXIS2_PLACEMENT_3D('',#46945,#37697,#37698) ;
#30832 = AXIS2_PLACEMENT_3D('',#46946,#37699,#37700) ;
#30833 = AXIS2_PLACEMENT_3D('',#46947,#37701,#37702) ;
#30834 = AXIS2_PLACEMENT_3D('',#46956,#37707,#37708) ;
#30835 = AXIS2_PLACEMENT_3D('',#46959,#37711,#37712) ;
#30836 = AXIS2_PLACEMENT_3D('',#46961,#37714,#37715) ;
#30837 = AXIS2_PLACEMENT_3D('',#46963,#37717,#37718) ;
#30838 = AXIS2_PLACEMENT_3D('',#46964,#37719,#37720) ;
#30839 = AXIS2_PLACEMENT_3D('',#46967,#37722,#37723) ;
#30840 = AXIS2_PLACEMENT_3D('',#46968,#37724,#37725) ;
#30841 = AXIS2_PLACEMENT_3D('',#46969,#37726,#37727) ;
#30842 = AXIS2_PLACEMENT_3D('',#46970,#37728,#37729) ;
#30843 = AXIS2_PLACEMENT_3D('',#46972,#37730,#37731) ;
#30844 = AXIS2_PLACEMENT_3D('',#46975,#37733,#37734) ;
#30845 = AXIS2_PLACEMENT_3D('',#46976,#37735,#37736) ;
#30846 = AXIS2_PLACEMENT_3D('',#46979,#37738,#37739) ;
#30847 = AXIS2_PLACEMENT_3D('',#46980,#37740,#37741) ;
#30848 = AXIS2_PLACEMENT_3D('',#46982,#37742,#37743) ;
#30849 = AXIS2_PLACEMENT_3D('',#46985,#37745,#37746) ;
#30850 = AXIS2_PLACEMENT_3D('',#46986,#37747,#37748) ;
#30851 = AXIS2_PLACEMENT_3D('',#46987,#37749,#37750) ;
#30852 = AXIS2_PLACEMENT_3D('',#46988,#37751,#37752) ;
#30853 = AXIS2_PLACEMENT_3D('',#46990,#37753,#37754) ;
#30854 = AXIS2_PLACEMENT_3D('',#46992,#37755,#37756) ;
#30855 = AXIS2_PLACEMENT_3D('',#46993,#37757,#37758) ;
#30856 = AXIS2_PLACEMENT_3D('',#46995,#37759,#37760) ;
#30857 = AXIS2_PLACEMENT_3D('',#46997,#37761,#37762) ;
#30858 = AXIS2_PLACEMENT_3D('',#46998,#37763,#37764) ;
#30859 = AXIS2_PLACEMENT_3D('',#47000,#37766,#37767) ;
#30860 = AXIS2_PLACEMENT_3D('',#47002,#37769,#37770) ;
#30861 = AXIS2_PLACEMENT_3D('',#47003,#37771,#37772) ;
#30862 = AXIS2_PLACEMENT_3D('',#47005,#37773,#37774) ;
#30863 = AXIS2_PLACEMENT_3D('',#47008,#37776,#37777) ;
#30864 = AXIS2_PLACEMENT_3D('',#47009,#37778,#37779) ;
#30865 = AXIS2_PLACEMENT_3D('',#47011,#37780,#37781) ;
#30866 = AXIS2_PLACEMENT_3D('',#47014,#37783,#37784) ;
#30867 = AXIS2_PLACEMENT_3D('',#47015,#37785,#37786) ;
#30868 = AXIS2_PLACEMENT_3D('',#47017,#37787,#37788) ;
#30869 = AXIS2_PLACEMENT_3D('',#47020,#37790,#37791) ;
#30870 = AXIS2_PLACEMENT_3D('',#47021,#37792,#37793) ;
#30871 = AXIS2_PLACEMENT_3D('',#47023,#37794,#37795) ;
#30872 = AXIS2_PLACEMENT_3D('',#47026,#37797,#37798) ;
#30873 = AXIS2_PLACEMENT_3D('',#47027,#37799,#37800) ;
#30874 = AXIS2_PLACEMENT_3D('',#47029,#37801,#37802) ;
#30875 = AXIS2_PLACEMENT_3D('',#47032,#37804,#37805) ;
#30876 = AXIS2_PLACEMENT_3D('',#47033,#37806,#37807) ;
#30877 = AXIS2_PLACEMENT_3D('',#47035,#37808,#37809) ;
#30878 = AXIS2_PLACEMENT_3D('',#47038,#37811,#37812) ;
#30879 = AXIS2_PLACEMENT_3D('',#47039,#37813,#37814) ;
#30880 = AXIS2_PLACEMENT_3D('',#47041,#37815,#37816) ;
#30881 = AXIS2_PLACEMENT_3D('',#47044,#37818,#37819) ;
#30882 = AXIS2_PLACEMENT_3D('',#47045,#37820,#37821) ;
#30883 = AXIS2_PLACEMENT_3D('',#47047,#37822,#37823) ;
#30884 = AXIS2_PLACEMENT_3D('',#47050,#37825,#37826) ;
#30885 = AXIS2_PLACEMENT_3D('',#47051,#37827,#37828) ;
#30886 = AXIS2_PLACEMENT_3D('',#47060,#37833,#37834) ;
#30887 = AXIS2_PLACEMENT_3D('',#47061,#37835,#37836) ;
#30888 = AXIS2_PLACEMENT_3D('',#47062,#37837,#37838) ;
#30889 = AXIS2_PLACEMENT_3D('',#47063,#37839,#37840) ;
#30890 = AXIS2_PLACEMENT_3D('',#47064,#37841,#37842) ;
#30891 = AXIS2_PLACEMENT_3D('',#47065,#37843,#37844) ;
#30892 = AXIS2_PLACEMENT_3D('',#47066,#37845,#37846) ;
#30893 = AXIS2_PLACEMENT_3D('',#47069,#37847,#37848) ;
#30894 = AXIS2_PLACEMENT_3D('',#47070,#37849,#37850) ;
#30895 = AXIS2_PLACEMENT_3D('',#47073,#37852,#37853) ;
#30896 = AXIS2_PLACEMENT_3D('',#47074,#37854,#37855) ;
#30897 = AXIS2_PLACEMENT_3D('',#47075,#37856,#37857) ;
#30898 = AXIS2_PLACEMENT_3D('',#47081,#37861,#37862) ;
#30899 = AXIS2_PLACEMENT_3D('',#47087,#37866,#37867) ;
#30900 = AXIS2_PLACEMENT_3D('',#47089,#37868,#37869) ;
#30901 = AXIS2_PLACEMENT_3D('',#47092,#37871,#37872) ;
#30902 = AXIS2_PLACEMENT_3D('',#47093,#37873,#37874) ;
#30903 = AXIS2_PLACEMENT_3D('',#47095,#37875,#37876) ;
#30904 = AXIS2_PLACEMENT_3D('',#47096,#37877,#37878) ;
#30905 = AXIS2_PLACEMENT_3D('',#47097,#37879,#37880) ;
#30906 = AXIS2_PLACEMENT_3D('',#47099,#37881,#37882) ;
#30907 = AXIS2_PLACEMENT_3D('',#47101,#37884,#37885) ;
#30908 = AXIS2_PLACEMENT_3D('',#47103,#37886,#37887) ;
#30909 = AXIS2_PLACEMENT_3D('',#47106,#37889,#37890) ;
#30910 = AXIS2_PLACEMENT_3D('',#47107,#37891,#37892) ;
#30911 = AXIS2_PLACEMENT_3D('',#47124,#37901,#37902) ;
#30912 = AXIS2_PLACEMENT_3D('',#47138,#37910,#37911) ;
#30913 = AXIS2_PLACEMENT_3D('',#47141,#37914,#37915) ;
#30914 = AXIS2_PLACEMENT_3D('',#47143,#37917,#37918) ;
#30915 = AXIS2_PLACEMENT_3D('',#47145,#37920,#37921) ;
#30916 = AXIS2_PLACEMENT_3D('',#47146,#37922,#37923) ;
#30917 = AXIS2_PLACEMENT_3D('',#47150,#37926,#37927) ;
#30918 = AXIS2_PLACEMENT_3D('',#47154,#37930,#37931) ;
#30919 = AXIS2_PLACEMENT_3D('',#47156,#37933,#37934) ;
#30920 = AXIS2_PLACEMENT_3D('',#47157,#37935,#37936) ;
#30921 = AXIS2_PLACEMENT_3D('',#47163,#37940,#37941) ;
#30922 = AXIS2_PLACEMENT_3D('',#47167,#37944,#37945) ;
#30923 = AXIS2_PLACEMENT_3D('',#47171,#37948,#37949) ;
#30924 = AXIS2_PLACEMENT_3D('',#47173,#37951,#37952) ;
#30925 = AXIS2_PLACEMENT_3D('',#47174,#37953,#37954) ;
#30926 = AXIS2_PLACEMENT_3D('',#47175,#37955,#37956) ;
#30927 = AXIS2_PLACEMENT_3D('',#47177,#37957,#37958) ;
#30928 = AXIS2_PLACEMENT_3D('',#47180,#37960,#37961) ;
#30929 = AXIS2_PLACEMENT_3D('',#47181,#37962,#37963) ;
#30930 = AXIS2_PLACEMENT_3D('',#47182,#37964,#37965) ;
#30931 = AXIS2_PLACEMENT_3D('',#47184,#37966,#37967) ;
#30932 = AXIS2_PLACEMENT_3D('',#47185,#37968,#37969) ;
#30933 = AXIS2_PLACEMENT_3D('',#47186,#37970,#37971) ;
#30934 = AXIS2_PLACEMENT_3D('',#47188,#37972,#37973) ;
#30935 = AXIS2_PLACEMENT_3D('',#47190,#37974,#37975) ;
#30936 = AXIS2_PLACEMENT_3D('',#47191,#37976,#37977) ;
#30937 = AXIS2_PLACEMENT_3D('',#47194,#37979,#37980) ;
#30938 = AXIS2_PLACEMENT_3D('',#47195,#37981,#37982) ;
#30939 = AXIS2_PLACEMENT_3D('',#47196,#37983,#37984) ;
#30940 = AXIS2_PLACEMENT_3D('',#47198,#37985,#37986) ;
#30941 = AXIS2_PLACEMENT_3D('',#47200,#37988,#37989) ;
#30942 = AXIS2_PLACEMENT_3D('',#47201,#37990,#37991) ;
#30943 = AXIS2_PLACEMENT_3D('',#47202,#37992,#37993) ;
#30944 = AXIS2_PLACEMENT_3D('',#47205,#37994,#37995) ;
#30945 = AXIS2_PLACEMENT_3D('',#47206,#37996,#37997) ;
#30946 = AXIS2_PLACEMENT_3D('',#47209,#37998,#37999) ;
#30947 = AXIS2_PLACEMENT_3D('',#47210,#38000,#38001) ;
#30948 = AXIS2_PLACEMENT_3D('',#47213,#38002,#38003) ;
#30949 = AXIS2_PLACEMENT_3D('',#47214,#38004,#38005) ;
#30950 = AXIS2_PLACEMENT_3D('',#47216,#38006,#38007) ;
#30951 = AXIS2_PLACEMENT_3D('',#47217,#38008,#38009) ;
#30952 = AXIS2_PLACEMENT_3D('',#47219,#38010,#38011) ;
#30953 = AXIS2_PLACEMENT_3D('',#47221,#38013,#38014) ;
#30954 = AXIS2_PLACEMENT_3D('',#47222,#38015,#38016) ;
#30955 = AXIS2_PLACEMENT_3D('',#47225,#38017,#38018) ;
#30956 = AXIS2_PLACEMENT_3D('',#47226,#38019,#38020) ;
#30957 = AXIS2_PLACEMENT_3D('',#47227,#38021,#38022) ;
#30958 = AXIS2_PLACEMENT_3D('',#47230,#38023,#38024) ;
#30959 = AXIS2_PLACEMENT_3D('',#47232,#38025,#38026) ;
#30960 = AXIS2_PLACEMENT_3D('',#47234,#38027,#38028) ;
#30961 = AXIS2_PLACEMENT_3D('',#47235,#38029,#38030) ;
#30962 = AXIS2_PLACEMENT_3D('',#47236,#38031,#38032) ;
#30963 = AXIS2_PLACEMENT_3D('',#47239,#38033,#38034) ;
#30964 = AXIS2_PLACEMENT_3D('',#47240,#38035,#38036) ;
#30965 = AXIS2_PLACEMENT_3D('',#47241,#38037,#38038) ;
#30966 = AXIS2_PLACEMENT_3D('',#47244,#38039,#38040) ;
#30967 = AXIS2_PLACEMENT_3D('',#47246,#38041,#38042) ;
#30968 = AXIS2_PLACEMENT_3D('',#47247,#38043,#38044) ;
#30969 = AXIS2_PLACEMENT_3D('',#47248,#38045,#38046) ;
#30970 = AXIS2_PLACEMENT_3D('',#47250,#38047,#38048) ;
#30971 = AXIS2_PLACEMENT_3D('',#47273,#38050,#38051) ;
#30972 = AXIS2_PLACEMENT_3D('',#47275,#38052,#38053) ;
#30973 = AXIS2_PLACEMENT_3D('',#47278,#38055,#38056) ;
#30974 = AXIS2_PLACEMENT_3D('',#47279,#38057,#38058) ;
#30975 = AXIS2_PLACEMENT_3D('',#47281,#38059,#38060) ;
#30976 = AXIS2_PLACEMENT_3D('',#47285,#38062,#38063) ;
#30977 = AXIS2_PLACEMENT_3D('',#47287,#38064,#38065) ;
#30978 = AXIS2_PLACEMENT_3D('',#47288,#38066,#38067) ;
#30979 = AXIS2_PLACEMENT_3D('',#47289,#38068,#38069) ;
#30980 = AXIS2_PLACEMENT_3D('',#47290,#38070,#38071) ;
#30981 = AXIS2_PLACEMENT_3D('',#47292,#38072,#38073) ;
#30982 = AXIS2_PLACEMENT_3D('',#47295,#38075,#38076) ;
#30983 = AXIS2_PLACEMENT_3D('',#47296,#38077,#38078) ;
#30984 = AXIS2_PLACEMENT_3D('',#47297,#38079,#38080) ;
#30985 = AXIS2_PLACEMENT_3D('',#47298,#38081,#38082) ;
#30986 = AXIS2_PLACEMENT_3D('',#47300,#38084,#38085) ;
#30987 = AXIS2_PLACEMENT_3D('',#47301,#38086,#38087) ;
#30988 = AXIS2_PLACEMENT_3D('',#47305,#38089,#38090) ;
#30989 = AXIS2_PLACEMENT_3D('',#47306,#38091,#38092) ;
#30990 = AXIS2_PLACEMENT_3D('',#47307,#38093,#38094) ;
#30991 = AXIS2_PLACEMENT_3D('',#47308,#38095,#38096) ;
#30992 = AXIS2_PLACEMENT_3D('',#47311,#38098,#38099) ;
#30993 = AXIS2_PLACEMENT_3D('',#47312,#38100,#38101) ;
#30994 = AXIS2_PLACEMENT_3D('',#47313,#38102,#38103) ;
#30995 = AXIS2_PLACEMENT_3D('',#47314,#38104,#38105) ;
#30996 = AXIS2_PLACEMENT_3D('',#47317,#38107,#38108) ;
#30997 = AXIS2_PLACEMENT_3D('',#47318,#38109,#38110) ;
#30998 = AXIS2_PLACEMENT_3D('',#47319,#38111,#38112) ;
#30999 = AXIS2_PLACEMENT_3D('',#47320,#38113,#38114) ;
#31000 = AXIS2_PLACEMENT_3D('',#47321,#38115,#38116) ;
#31001 = AXIS2_PLACEMENT_3D('',#47322,#38117,#38118) ;
#31002 = AXIS2_PLACEMENT_3D('',#47324,#38119,#38120) ;
#31003 = AXIS2_PLACEMENT_3D('',#47325,#38121,#38122) ;
#31004 = AXIS2_PLACEMENT_3D('',#47328,#38123,#38124) ;
#31005 = AXIS2_PLACEMENT_3D('',#47330,#38125,#38126) ;
#31006 = AXIS2_PLACEMENT_3D('',#47331,#38127,#38128) ;
#31007 = AXIS2_PLACEMENT_3D('',#47332,#38129,#38130) ;
#31008 = AXIS2_PLACEMENT_3D('',#47352,#38132,#38133) ;
#31009 = AXIS2_PLACEMENT_3D('',#47353,#38134,#38135) ;
#31010 = AXIS2_PLACEMENT_3D('',#47356,#38136,#38137) ;
#31011 = AXIS2_PLACEMENT_3D('',#47357,#38138,#38139) ;
#31012 = AXIS2_PLACEMENT_3D('',#47360,#38140,#38141) ;
#31013 = AXIS2_PLACEMENT_3D('',#47362,#38142,#38143) ;
#31014 = AXIS2_PLACEMENT_3D('',#47363,#38144,#38145) ;
#31015 = AXIS2_PLACEMENT_3D('',#47364,#38146,#38147) ;
#31016 = AXIS2_PLACEMENT_3D('',#47379,#38148,#38149) ;
#31017 = AXIS2_PLACEMENT_3D('',#47400,#38150,#38151) ;
#31018 = AXIS2_PLACEMENT_3D('',#47401,#38152,#38153) ;
#31019 = AXIS2_PLACEMENT_3D('',#47404,#38155,#38156) ;
#31020 = AXIS2_PLACEMENT_3D('',#47405,#38157,#38158) ;
#31021 = AXIS2_PLACEMENT_3D('',#47406,#38159,#38160) ;
#31022 = AXIS2_PLACEMENT_3D('',#47407,#38161,#38162) ;
#31023 = AXIS2_PLACEMENT_3D('',#47410,#38163,#38164) ;
#31024 = AXIS2_PLACEMENT_3D('',#47412,#38165,#38166) ;
#31025 = AXIS2_PLACEMENT_3D('',#47413,#38167,#38168) ;
#31026 = AXIS2_PLACEMENT_3D('',#47415,#38169,#38170) ;
#31027 = AXIS2_PLACEMENT_3D('',#47416,#38171,#38172) ;
#31028 = AXIS2_PLACEMENT_3D('',#47437,#38173,#38174) ;
#31029 = AXIS2_PLACEMENT_3D('',#47438,#38175,#38176) ;
#31030 = AXIS2_PLACEMENT_3D('',#47440,#38177,#38178) ;
#31031 = AXIS2_PLACEMENT_3D('',#47456,#38180,#38181) ;
#31032 = AXIS2_PLACEMENT_3D('',#47457,#38182,#38183) ;
#31033 = AXIS2_PLACEMENT_3D('',#47458,#38184,#38185) ;
#31034 = AXIS2_PLACEMENT_3D('',#47459,#38186,#38187) ;
#31035 = AXIS2_PLACEMENT_3D('',#47462,#38188,#38189) ;
#31036 = AXIS2_PLACEMENT_3D('',#47463,#38190,#38191) ;
#31037 = AXIS2_PLACEMENT_3D('',#47464,#38192,#38193) ;
#31038 = AXIS2_PLACEMENT_3D('',#47467,#38194,#38195) ;
#31039 = AXIS2_PLACEMENT_3D('',#47469,#38196,#38197) ;
#31040 = AXIS2_PLACEMENT_3D('',#47472,#38199,#38200) ;
#31041 = AXIS2_PLACEMENT_3D('',#47474,#38201,#38202) ;
#31042 = AXIS2_PLACEMENT_3D('',#47476,#38203,#38204) ;
#31043 = AXIS2_PLACEMENT_3D('',#47477,#38205,#38206) ;
#31044 = AXIS2_PLACEMENT_3D('',#47478,#38207,#38208) ;
#31045 = AXIS2_PLACEMENT_3D('',#47479,#38209,#38210) ;
#31046 = AXIS2_PLACEMENT_3D('',#47485,#38214,#38215) ;
#31047 = AXIS2_PLACEMENT_3D('',#47487,#38216,#38217) ;
#31048 = AXIS2_PLACEMENT_3D('',#47488,#38218,#38219) ;
#31049 = AXIS2_PLACEMENT_3D('',#47489,#38220,#38221) ;
#31050 = AXIS2_PLACEMENT_3D('',#47492,#38223,#38224) ;
#31051 = AXIS2_PLACEMENT_3D('',#47493,#38225,#38226) ;
#31052 = AXIS2_PLACEMENT_3D('',#47494,#38227,#38228) ;
#31053 = AXIS2_PLACEMENT_3D('',#47496,#38229,#38230) ;
#31054 = AXIS2_PLACEMENT_3D('',#47499,#38232,#38233) ;
#31055 = AXIS2_PLACEMENT_3D('',#47500,#38234,#38235) ;
#31056 = AXIS2_PLACEMENT_3D('',#47501,#38236,#38237) ;
#31057 = AXIS2_PLACEMENT_3D('',#47502,#38238,#38239) ;
#31058 = AXIS2_PLACEMENT_3D('',#47503,#38240,#38241) ;
#31059 = AXIS2_PLACEMENT_3D('',#47505,#38242,#38243) ;
#31060 = AXIS2_PLACEMENT_3D('',#47508,#38245,#38246) ;
#31061 = AXIS2_PLACEMENT_3D('',#47509,#38247,#38248) ;
#31062 = AXIS2_PLACEMENT_3D('',#47510,#38249,#38250) ;
#31063 = AXIS2_PLACEMENT_3D('',#47511,#38251,#38252) ;
#31064 = AXIS2_PLACEMENT_3D('',#47512,#38253,#38254) ;
#31065 = AXIS2_PLACEMENT_3D('',#47514,#38255,#38256) ;
#31066 = AXIS2_PLACEMENT_3D('',#47517,#38258,#38259) ;
#31067 = AXIS2_PLACEMENT_3D('',#47518,#38260,#38261) ;
#31068 = AXIS2_PLACEMENT_3D('',#47519,#38262,#38263) ;
#31069 = AXIS2_PLACEMENT_3D('',#47520,#38264,#38265) ;
#31070 = AXIS2_PLACEMENT_3D('',#47521,#38266,#38267) ;
#31071 = AXIS2_PLACEMENT_3D('',#47523,#38268,#38269) ;
#31072 = AXIS2_PLACEMENT_3D('',#47526,#38271,#38272) ;
#31073 = AXIS2_PLACEMENT_3D('',#47565,#38273,#38274) ;
#31074 = AXIS2_PLACEMENT_3D('',#47567,#38275,#38276) ;
#31075 = AXIS2_PLACEMENT_3D('',#47570,#38278,#38279) ;
#31076 = AXIS2_PLACEMENT_3D('',#47571,#38280,#38281) ;
#31077 = AXIS2_PLACEMENT_3D('',#47572,#38282,#38283) ;
#31078 = AXIS2_PLACEMENT_3D('',#47573,#38284,#38285) ;
#31079 = AXIS2_PLACEMENT_3D('',#47575,#38286,#38287) ;
#31080 = AXIS2_PLACEMENT_3D('',#47577,#38289,#38290) ;
#31081 = AXIS2_PLACEMENT_3D('',#47578,#38291,#38292) ;
#31082 = AXIS2_PLACEMENT_3D('',#47580,#38293,#38294) ;
#31083 = AXIS2_PLACEMENT_3D('',#47583,#38296,#38297) ;
#31084 = AXIS2_PLACEMENT_3D('',#47584,#38298,#38299) ;
#31085 = AXIS2_PLACEMENT_3D('',#47586,#38300,#38301) ;
#31086 = AXIS2_PLACEMENT_3D('',#47589,#38303,#38304) ;
#31087 = AXIS2_PLACEMENT_3D('',#47590,#38305,#38306) ;
#31088 = AXIS2_PLACEMENT_3D('',#47591,#38307,#38308) ;
#31089 = AXIS2_PLACEMENT_3D('',#47592,#38309,#38310) ;
#31090 = AXIS2_PLACEMENT_3D('',#47595,#38311,#38312) ;
#31091 = AXIS2_PLACEMENT_3D('',#47625,#38313,#38314) ;
#31092 = AXIS2_PLACEMENT_3D('',#47628,#38316,#38317) ;
#31093 = AXIS2_PLACEMENT_3D('',#47629,#38318,#38319) ;
#31094 = AXIS2_PLACEMENT_3D('',#47631,#38320,#38321) ;
#31095 = AXIS2_PLACEMENT_3D('',#47634,#38323,#38324) ;
#31096 = AXIS2_PLACEMENT_3D('',#47635,#38325,#38326) ;
#31097 = AXIS2_PLACEMENT_3D('',#47639,#38328,#38329) ;
#31098 = AXIS2_PLACEMENT_3D('',#47641,#38330,#38331) ;
#31099 = AXIS2_PLACEMENT_3D('',#47643,#38332,#38333) ;
#31100 = AXIS2_PLACEMENT_3D('',#47645,#38334,#38335) ;
#31101 = AXIS2_PLACEMENT_3D('',#47646,#38336,#38337) ;
#31102 = AXIS2_PLACEMENT_3D('',#47647,#38338,#38339) ;
#31103 = AXIS2_PLACEMENT_3D('',#47648,#38340,#38341) ;
#31104 = AXIS2_PLACEMENT_3D('',#47649,#38342,#38343) ;
#31105 = AXIS2_PLACEMENT_3D('',#47650,#38344,#38345) ;
#31106 = AXIS2_PLACEMENT_3D('',#47652,#38346,#38347) ;
#31107 = AXIS2_PLACEMENT_3D('',#47653,#38348,#38349) ;
#31108 = AXIS2_PLACEMENT_3D('',#47654,#38350,#38351) ;
#31109 = AXIS2_PLACEMENT_3D('',#47656,#38352,#38353) ;
#31110 = AXIS2_PLACEMENT_3D('',#47658,#38354,#38355) ;
#31111 = AXIS2_PLACEMENT_3D('',#47659,#38356,#38357) ;
#31112 = AXIS2_PLACEMENT_3D('',#47660,#38358,#38359) ;
#31113 = AXIS2_PLACEMENT_3D('',#47663,#38360,#38361) ;
#31114 = AXIS2_PLACEMENT_3D('',#47665,#38362,#38363) ;
#31115 = AXIS2_PLACEMENT_3D('',#47666,#38364,#38365) ;
#31116 = AXIS2_PLACEMENT_3D('',#47667,#38366,#38367) ;
#31117 = AXIS2_PLACEMENT_3D('',#47670,#38368,#38369) ;
#31118 = AXIS2_PLACEMENT_3D('',#47672,#38370,#38371) ;
#31119 = AXIS2_PLACEMENT_3D('',#47674,#38372,#38373) ;
#31120 = AXIS2_PLACEMENT_3D('',#47676,#38374,#38375) ;
#31121 = AXIS2_PLACEMENT_3D('',#47677,#38376,#38377) ;
#31122 = AXIS2_PLACEMENT_3D('',#47678,#38378,#38379) ;
#31123 = AXIS2_PLACEMENT_3D('',#47681,#38380,#38381) ;
#31124 = AXIS2_PLACEMENT_3D('',#47683,#38382,#38383) ;
#31125 = AXIS2_PLACEMENT_3D('',#47684,#38384,#38385) ;
#31126 = AXIS2_PLACEMENT_3D('',#47685,#38386,#38387) ;
#31127 = AXIS2_PLACEMENT_3D('',#47688,#38388,#38389) ;
#31128 = AXIS2_PLACEMENT_3D('',#47690,#38390,#38391) ;
#31129 = AXIS2_PLACEMENT_3D('',#47691,#38392,#38393) ;
#31130 = AXIS2_PLACEMENT_3D('',#47692,#38394,#38395) ;
#31131 = AXIS2_PLACEMENT_3D('',#47695,#38396,#38397) ;
#31132 = AXIS2_PLACEMENT_3D('',#47697,#38398,#38399) ;
#31133 = AXIS2_PLACEMENT_3D('',#47698,#38400,#38401) ;
#31134 = AXIS2_PLACEMENT_3D('',#47699,#38402,#38403) ;
#31135 = AXIS2_PLACEMENT_3D('',#47702,#38404,#38405) ;
#31136 = AXIS2_PLACEMENT_3D('',#47704,#38406,#38407) ;
#31137 = AXIS2_PLACEMENT_3D('',#47706,#38408,#38409) ;
#31138 = AXIS2_PLACEMENT_3D('',#47708,#38410,#38411) ;
#31139 = AXIS2_PLACEMENT_3D('',#47709,#38412,#38413) ;
#31140 = AXIS2_PLACEMENT_3D('',#47710,#38414,#38415) ;
#31141 = AXIS2_PLACEMENT_3D('',#47713,#38416,#38417) ;
#31142 = AXIS2_PLACEMENT_3D('',#47715,#38418,#38419) ;
#31143 = AXIS2_PLACEMENT_3D('',#47716,#38420,#38421) ;
#31144 = AXIS2_PLACEMENT_3D('',#47717,#38422,#38423) ;
#31145 = AXIS2_PLACEMENT_3D('',#47720,#38424,#38425) ;
#31146 = AXIS2_PLACEMENT_3D('',#47722,#38426,#38427) ;
#31147 = AXIS2_PLACEMENT_3D('',#47723,#38428,#38429) ;
#31148 = AXIS2_PLACEMENT_3D('',#47724,#38430,#38431) ;
#31149 = AXIS2_PLACEMENT_3D('',#47727,#38432,#38433) ;
#31150 = AXIS2_PLACEMENT_3D('',#47729,#38434,#38435) ;
#31151 = AXIS2_PLACEMENT_3D('',#47730,#38436,#38437) ;
#31152 = AXIS2_PLACEMENT_3D('',#47731,#38438,#38439) ;
#31153 = AXIS2_PLACEMENT_3D('',#47734,#38440,#38441) ;
#31154 = AXIS2_PLACEMENT_3D('',#47736,#38442,#38443) ;
#31155 = AXIS2_PLACEMENT_3D('',#47738,#38444,#38445) ;
#31156 = AXIS2_PLACEMENT_3D('',#47740,#38446,#38447) ;
#31157 = AXIS2_PLACEMENT_3D('',#47741,#38448,#38449) ;
#31158 = AXIS2_PLACEMENT_3D('',#47742,#38450,#38451) ;
#31159 = AXIS2_PLACEMENT_3D('',#47745,#38452,#38453) ;
#31160 = AXIS2_PLACEMENT_3D('',#47747,#38454,#38455) ;
#31161 = AXIS2_PLACEMENT_3D('',#47748,#38456,#38457) ;
#31162 = AXIS2_PLACEMENT_3D('',#47749,#38458,#38459) ;
#31163 = AXIS2_PLACEMENT_3D('',#47752,#38460,#38461) ;
#31164 = AXIS2_PLACEMENT_3D('',#47754,#38462,#38463) ;
#31165 = AXIS2_PLACEMENT_3D('',#47755,#38464,#38465) ;
#31166 = AXIS2_PLACEMENT_3D('',#47756,#38466,#38467) ;
#31167 = AXIS2_PLACEMENT_3D('',#47759,#38468,#38469) ;
#31168 = AXIS2_PLACEMENT_3D('',#47761,#38470,#38471) ;
#31169 = AXIS2_PLACEMENT_3D('',#47762,#38472,#38473) ;
#31170 = AXIS2_PLACEMENT_3D('',#47763,#38474,#38475) ;
#31171 = AXIS2_PLACEMENT_3D('',#47766,#38476,#38477) ;
#31172 = AXIS2_PLACEMENT_3D('',#47768,#38478,#38479) ;
#31173 = AXIS2_PLACEMENT_3D('',#47770,#38480,#38481) ;
#31174 = AXIS2_PLACEMENT_3D('',#47772,#38482,#38483) ;
#31175 = AXIS2_PLACEMENT_3D('',#47773,#38484,#38485) ;
#31176 = AXIS2_PLACEMENT_3D('',#47774,#38486,#38487) ;
#31177 = AXIS2_PLACEMENT_3D('',#47777,#38488,#38489) ;
#31178 = AXIS2_PLACEMENT_3D('',#47779,#38490,#38491) ;
#31179 = AXIS2_PLACEMENT_3D('',#47780,#38492,#38493) ;
#31180 = AXIS2_PLACEMENT_3D('',#47781,#38494,#38495) ;
#31181 = AXIS2_PLACEMENT_3D('',#47784,#38496,#38497) ;
#31182 = AXIS2_PLACEMENT_3D('',#47786,#38498,#38499) ;
#31183 = AXIS2_PLACEMENT_3D('',#47787,#38500,#38501) ;
#31184 = AXIS2_PLACEMENT_3D('',#47788,#38502,#38503) ;
#31185 = AXIS2_PLACEMENT_3D('',#47791,#38504,#38505) ;
#31186 = AXIS2_PLACEMENT_3D('',#47793,#38506,#38507) ;
#31187 = AXIS2_PLACEMENT_3D('',#47794,#38508,#38509) ;
#31188 = AXIS2_PLACEMENT_3D('',#47795,#38510,#38511) ;
#31189 = AXIS2_PLACEMENT_3D('',#47798,#38512,#38513) ;
#31190 = AXIS2_PLACEMENT_3D('',#47800,#38514,#38515) ;
#31191 = AXIS2_PLACEMENT_3D('',#47802,#38516,#38517) ;
#31192 = AXIS2_PLACEMENT_3D('',#47804,#38518,#38519) ;
#31193 = AXIS2_PLACEMENT_3D('',#47805,#38520,#38521) ;
#31194 = AXIS2_PLACEMENT_3D('',#47806,#38522,#38523) ;
#31195 = AXIS2_PLACEMENT_3D('',#47809,#38524,#38525) ;
#31196 = AXIS2_PLACEMENT_3D('',#47811,#38526,#38527) ;
#31197 = AXIS2_PLACEMENT_3D('',#47812,#38528,#38529) ;
#31198 = AXIS2_PLACEMENT_3D('',#47813,#38530,#38531) ;
#31199 = AXIS2_PLACEMENT_3D('',#47816,#38532,#38533) ;
#31200 = AXIS2_PLACEMENT_3D('',#47818,#38534,#38535) ;
#31201 = AXIS2_PLACEMENT_3D('',#47819,#38536,#38537) ;
#31202 = AXIS2_PLACEMENT_3D('',#47820,#38538,#38539) ;
#31203 = AXIS2_PLACEMENT_3D('',#47823,#38540,#38541) ;
#31204 = AXIS2_PLACEMENT_3D('',#47825,#38542,#38543) ;
#31205 = AXIS2_PLACEMENT_3D('',#47826,#38544,#38545) ;
#31206 = AXIS2_PLACEMENT_3D('',#47827,#38546,#38547) ;
#31207 = AXIS2_PLACEMENT_3D('',#47830,#38548,#38549) ;
#31208 = AXIS2_PLACEMENT_3D('',#47832,#38550,#38551) ;
#31209 = AXIS2_PLACEMENT_3D('',#47834,#38552,#38553) ;
#31210 = AXIS2_PLACEMENT_3D('',#47836,#38554,#38555) ;
#31211 = AXIS2_PLACEMENT_3D('',#47837,#38556,#38557) ;
#31212 = AXIS2_PLACEMENT_3D('',#47838,#38558,#38559) ;
#31213 = AXIS2_PLACEMENT_3D('',#47841,#38560,#38561) ;
#31214 = AXIS2_PLACEMENT_3D('',#47843,#38562,#38563) ;
#31215 = AXIS2_PLACEMENT_3D('',#47844,#38564,#38565) ;
#31216 = AXIS2_PLACEMENT_3D('',#47845,#38566,#38567) ;
#31217 = AXIS2_PLACEMENT_3D('',#47848,#38568,#38569) ;
#31218 = AXIS2_PLACEMENT_3D('',#47850,#38570,#38571) ;
#31219 = AXIS2_PLACEMENT_3D('',#47851,#38572,#38573) ;
#31220 = AXIS2_PLACEMENT_3D('',#47852,#38574,#38575) ;
#31221 = AXIS2_PLACEMENT_3D('',#47855,#38576,#38577) ;
#31222 = AXIS2_PLACEMENT_3D('',#47857,#38578,#38579) ;
#31223 = AXIS2_PLACEMENT_3D('',#47858,#38580,#38581) ;
#31224 = AXIS2_PLACEMENT_3D('',#47859,#38582,#38583) ;
#31225 = AXIS2_PLACEMENT_3D('',#47862,#38584,#38585) ;
#31226 = AXIS2_PLACEMENT_3D('',#47864,#38586,#38587) ;
#31227 = AXIS2_PLACEMENT_3D('',#47866,#38588,#38589) ;
#31228 = AXIS2_PLACEMENT_3D('',#47868,#38590,#38591) ;
#31229 = AXIS2_PLACEMENT_3D('',#47869,#38592,#38593) ;
#31230 = AXIS2_PLACEMENT_3D('',#47870,#38594,#38595) ;
#31231 = AXIS2_PLACEMENT_3D('',#47873,#38596,#38597) ;
#31232 = AXIS2_PLACEMENT_3D('',#47875,#38598,#38599) ;
#31233 = AXIS2_PLACEMENT_3D('',#47876,#38600,#38601) ;
#31234 = AXIS2_PLACEMENT_3D('',#47877,#38602,#38603) ;
#31235 = AXIS2_PLACEMENT_3D('',#47880,#38604,#38605) ;
#31236 = AXIS2_PLACEMENT_3D('',#47882,#38606,#38607) ;
#31237 = AXIS2_PLACEMENT_3D('',#47883,#38608,#38609) ;
#31238 = AXIS2_PLACEMENT_3D('',#47884,#38610,#38611) ;
#31239 = AXIS2_PLACEMENT_3D('',#47887,#38612,#38613) ;
#31240 = AXIS2_PLACEMENT_3D('',#47889,#38614,#38615) ;
#31241 = AXIS2_PLACEMENT_3D('',#47890,#38616,#38617) ;
#31242 = AXIS2_PLACEMENT_3D('',#47891,#38618,#38619) ;
#31243 = AXIS2_PLACEMENT_3D('',#47894,#38620,#38621) ;
#31244 = AXIS2_PLACEMENT_3D('',#47896,#38622,#38623) ;
#31245 = AXIS2_PLACEMENT_3D('',#47898,#38624,#38625) ;
#31246 = AXIS2_PLACEMENT_3D('',#47900,#38626,#38627) ;
#31247 = AXIS2_PLACEMENT_3D('',#47901,#38628,#38629) ;
#31248 = AXIS2_PLACEMENT_3D('',#47902,#38630,#38631) ;
#31249 = AXIS2_PLACEMENT_3D('',#47905,#38632,#38633) ;
#31250 = AXIS2_PLACEMENT_3D('',#47907,#38634,#38635) ;
#31251 = AXIS2_PLACEMENT_3D('',#47908,#38636,#38637) ;
#31252 = AXIS2_PLACEMENT_3D('',#47909,#38638,#38639) ;
#31253 = AXIS2_PLACEMENT_3D('',#47912,#38640,#38641) ;
#31254 = AXIS2_PLACEMENT_3D('',#47914,#38642,#38643) ;
#31255 = AXIS2_PLACEMENT_3D('',#47915,#38644,#38645) ;
#31256 = AXIS2_PLACEMENT_3D('',#47916,#38646,#38647) ;
#31257 = AXIS2_PLACEMENT_3D('',#47919,#38648,#38649) ;
#31258 = AXIS2_PLACEMENT_3D('',#47921,#38650,#38651) ;
#31259 = AXIS2_PLACEMENT_3D('',#47922,#38652,#38653) ;
#31260 = AXIS2_PLACEMENT_3D('',#47923,#38654,#38655) ;
#31261 = AXIS2_PLACEMENT_3D('',#47926,#38656,#38657) ;
#31262 = AXIS2_PLACEMENT_3D('',#47928,#38658,#38659) ;
#31263 = AXIS2_PLACEMENT_3D('',#47930,#38660,#38661) ;
#31264 = AXIS2_PLACEMENT_3D('',#47932,#38662,#38663) ;
#31265 = AXIS2_PLACEMENT_3D('',#47933,#38664,#38665) ;
#31266 = AXIS2_PLACEMENT_3D('',#47934,#38666,#38667) ;
#31267 = AXIS2_PLACEMENT_3D('',#47937,#38668,#38669) ;
#31268 = AXIS2_PLACEMENT_3D('',#47939,#38670,#38671) ;
#31269 = AXIS2_PLACEMENT_3D('',#47940,#38672,#38673) ;
#31270 = AXIS2_PLACEMENT_3D('',#47941,#38674,#38675) ;
#31271 = AXIS2_PLACEMENT_3D('',#47944,#38676,#38677) ;
#31272 = AXIS2_PLACEMENT_3D('',#47946,#38678,#38679) ;
#31273 = AXIS2_PLACEMENT_3D('',#47947,#38680,#38681) ;
#31274 = AXIS2_PLACEMENT_3D('',#47948,#38682,#38683) ;
#31275 = AXIS2_PLACEMENT_3D('',#47951,#38684,#38685) ;
#31276 = AXIS2_PLACEMENT_3D('',#47953,#38686,#38687) ;
#31277 = AXIS2_PLACEMENT_3D('',#47954,#38688,#38689) ;
#31278 = AXIS2_PLACEMENT_3D('',#47955,#38690,#38691) ;
#31279 = AXIS2_PLACEMENT_3D('',#47958,#38692,#38693) ;
#31280 = AXIS2_PLACEMENT_3D('',#47960,#38694,#38695) ;
#31281 = AXIS2_PLACEMENT_3D('',#47962,#38696,#38697) ;
#31282 = AXIS2_PLACEMENT_3D('',#47964,#38698,#38699) ;
#31283 = AXIS2_PLACEMENT_3D('',#47965,#38700,#38701) ;
#31284 = AXIS2_PLACEMENT_3D('',#47966,#38702,#38703) ;
#31285 = AXIS2_PLACEMENT_3D('',#47969,#38704,#38705) ;
#31286 = AXIS2_PLACEMENT_3D('',#47971,#38706,#38707) ;
#31287 = AXIS2_PLACEMENT_3D('',#47972,#38708,#38709) ;
#31288 = AXIS2_PLACEMENT_3D('',#47973,#38710,#38711) ;
#31289 = AXIS2_PLACEMENT_3D('',#47976,#38712,#38713) ;
#31290 = AXIS2_PLACEMENT_3D('',#47978,#38714,#38715) ;
#31291 = AXIS2_PLACEMENT_3D('',#47979,#38716,#38717) ;
#31292 = AXIS2_PLACEMENT_3D('',#47980,#38718,#38719) ;
#31293 = AXIS2_PLACEMENT_3D('',#47983,#38720,#38721) ;
#31294 = AXIS2_PLACEMENT_3D('',#47985,#38722,#38723) ;
#31295 = AXIS2_PLACEMENT_3D('',#47986,#38724,#38725) ;
#31296 = AXIS2_PLACEMENT_3D('',#47987,#38726,#38727) ;
#31297 = AXIS2_PLACEMENT_3D('',#47990,#38728,#38729) ;
#31298 = AXIS2_PLACEMENT_3D('',#47992,#38730,#38731) ;
#31299 = AXIS2_PLACEMENT_3D('',#47994,#38732,#38733) ;
#31300 = AXIS2_PLACEMENT_3D('',#47996,#38734,#38735) ;
#31301 = AXIS2_PLACEMENT_3D('',#47997,#38736,#38737) ;
#31302 = AXIS2_PLACEMENT_3D('',#47998,#38738,#38739) ;
#31303 = AXIS2_PLACEMENT_3D('',#48001,#38740,#38741) ;
#31304 = AXIS2_PLACEMENT_3D('',#48003,#38742,#38743) ;
#31305 = AXIS2_PLACEMENT_3D('',#48004,#38744,#38745) ;
#31306 = AXIS2_PLACEMENT_3D('',#48005,#38746,#38747) ;
#31307 = AXIS2_PLACEMENT_3D('',#48008,#38748,#38749) ;
#31308 = AXIS2_PLACEMENT_3D('',#48010,#38750,#38751) ;
#31309 = AXIS2_PLACEMENT_3D('',#48011,#38752,#38753) ;
#31310 = AXIS2_PLACEMENT_3D('',#48012,#38754,#38755) ;
#31311 = AXIS2_PLACEMENT_3D('',#48015,#38756,#38757) ;
#31312 = AXIS2_PLACEMENT_3D('',#48017,#38758,#38759) ;
#31313 = AXIS2_PLACEMENT_3D('',#48018,#38760,#38761) ;
#31314 = AXIS2_PLACEMENT_3D('',#48019,#38762,#38763) ;
#31315 = AXIS2_PLACEMENT_3D('',#48022,#38764,#38765) ;
#31316 = AXIS2_PLACEMENT_3D('',#48024,#38766,#38767) ;
#31317 = AXIS2_PLACEMENT_3D('',#48026,#38768,#38769) ;
#31318 = AXIS2_PLACEMENT_3D('',#48028,#38770,#38771) ;
#31319 = AXIS2_PLACEMENT_3D('',#48029,#38772,#38773) ;
#31320 = AXIS2_PLACEMENT_3D('',#48030,#38774,#38775) ;
#31321 = AXIS2_PLACEMENT_3D('',#48033,#38776,#38777) ;
#31322 = AXIS2_PLACEMENT_3D('',#48035,#38778,#38779) ;
#31323 = AXIS2_PLACEMENT_3D('',#48036,#38780,#38781) ;
#31324 = AXIS2_PLACEMENT_3D('',#48037,#38782,#38783) ;
#31325 = AXIS2_PLACEMENT_3D('',#48040,#38784,#38785) ;
#31326 = AXIS2_PLACEMENT_3D('',#48042,#38786,#38787) ;
#31327 = AXIS2_PLACEMENT_3D('',#48043,#38788,#38789) ;
#31328 = AXIS2_PLACEMENT_3D('',#48044,#38790,#38791) ;
#31329 = AXIS2_PLACEMENT_3D('',#48047,#38792,#38793) ;
#31330 = AXIS2_PLACEMENT_3D('',#48049,#38794,#38795) ;
#31331 = AXIS2_PLACEMENT_3D('',#48050,#38796,#38797) ;
#31332 = AXIS2_PLACEMENT_3D('',#48051,#38798,#38799) ;
#31333 = AXIS2_PLACEMENT_3D('',#48054,#38800,#38801) ;
#31334 = AXIS2_PLACEMENT_3D('',#48056,#38802,#38803) ;
#31335 = AXIS2_PLACEMENT_3D('',#48058,#38804,#38805) ;
#31336 = AXIS2_PLACEMENT_3D('',#48060,#38806,#38807) ;
#31337 = AXIS2_PLACEMENT_3D('',#48061,#38808,#38809) ;
#31338 = AXIS2_PLACEMENT_3D('',#48062,#38810,#38811) ;
#31339 = AXIS2_PLACEMENT_3D('',#48065,#38812,#38813) ;
#31340 = AXIS2_PLACEMENT_3D('',#48067,#38814,#38815) ;
#31341 = AXIS2_PLACEMENT_3D('',#48068,#38816,#38817) ;
#31342 = AXIS2_PLACEMENT_3D('',#48069,#38818,#38819) ;
#31343 = AXIS2_PLACEMENT_3D('',#48072,#38820,#38821) ;
#31344 = AXIS2_PLACEMENT_3D('',#48074,#38822,#38823) ;
#31345 = AXIS2_PLACEMENT_3D('',#48075,#38824,#38825) ;
#31346 = AXIS2_PLACEMENT_3D('',#48076,#38826,#38827) ;
#31347 = AXIS2_PLACEMENT_3D('',#48079,#38828,#38829) ;
#31348 = AXIS2_PLACEMENT_3D('',#48081,#38830,#38831) ;
#31349 = AXIS2_PLACEMENT_3D('',#48082,#38832,#38833) ;
#31350 = AXIS2_PLACEMENT_3D('',#48083,#38834,#38835) ;
#31351 = AXIS2_PLACEMENT_3D('',#48086,#38836,#38837) ;
#31352 = AXIS2_PLACEMENT_3D('',#48088,#38838,#38839) ;
#31353 = AXIS2_PLACEMENT_3D('',#48090,#38840,#38841) ;
#31354 = AXIS2_PLACEMENT_3D('',#48092,#38842,#38843) ;
#31355 = AXIS2_PLACEMENT_3D('',#48093,#38844,#38845) ;
#31356 = AXIS2_PLACEMENT_3D('',#48094,#38846,#38847) ;
#31357 = AXIS2_PLACEMENT_3D('',#48097,#38848,#38849) ;
#31358 = AXIS2_PLACEMENT_3D('',#48099,#38850,#38851) ;
#31359 = AXIS2_PLACEMENT_3D('',#48100,#38852,#38853) ;
#31360 = AXIS2_PLACEMENT_3D('',#48101,#38854,#38855) ;
#31361 = AXIS2_PLACEMENT_3D('',#48104,#38856,#38857) ;
#31362 = AXIS2_PLACEMENT_3D('',#48106,#38858,#38859) ;
#31363 = AXIS2_PLACEMENT_3D('',#48107,#38860,#38861) ;
#31364 = AXIS2_PLACEMENT_3D('',#48108,#38862,#38863) ;
#31365 = AXIS2_PLACEMENT_3D('',#48111,#38864,#38865) ;
#31366 = AXIS2_PLACEMENT_3D('',#48113,#38866,#38867) ;
#31367 = AXIS2_PLACEMENT_3D('',#48114,#38868,#38869) ;
#31368 = AXIS2_PLACEMENT_3D('',#48115,#38870,#38871) ;
#31369 = AXIS2_PLACEMENT_3D('',#48118,#38872,#38873) ;
#31370 = AXIS2_PLACEMENT_3D('',#48120,#38874,#38875) ;
#31371 = AXIS2_PLACEMENT_3D('',#48122,#38876,#38877) ;
#31372 = AXIS2_PLACEMENT_3D('',#48124,#38878,#38879) ;
#31373 = AXIS2_PLACEMENT_3D('',#48125,#38880,#38881) ;
#31374 = AXIS2_PLACEMENT_3D('',#48126,#38882,#38883) ;
#31375 = AXIS2_PLACEMENT_3D('',#48129,#38884,#38885) ;
#31376 = AXIS2_PLACEMENT_3D('',#48131,#38886,#38887) ;
#31377 = AXIS2_PLACEMENT_3D('',#48132,#38888,#38889) ;
#31378 = AXIS2_PLACEMENT_3D('',#48133,#38890,#38891) ;
#31379 = AXIS2_PLACEMENT_3D('',#48136,#38892,#38893) ;
#31380 = AXIS2_PLACEMENT_3D('',#48138,#38894,#38895) ;
#31381 = AXIS2_PLACEMENT_3D('',#48139,#38896,#38897) ;
#31382 = AXIS2_PLACEMENT_3D('',#48140,#38898,#38899) ;
#31383 = AXIS2_PLACEMENT_3D('',#48143,#38900,#38901) ;
#31384 = AXIS2_PLACEMENT_3D('',#48145,#38902,#38903) ;
#31385 = AXIS2_PLACEMENT_3D('',#48146,#38904,#38905) ;
#31386 = AXIS2_PLACEMENT_3D('',#48147,#38906,#38907) ;
#31387 = AXIS2_PLACEMENT_3D('',#48150,#38908,#38909) ;
#31388 = AXIS2_PLACEMENT_3D('',#48152,#38910,#38911) ;
#31389 = AXIS2_PLACEMENT_3D('',#48154,#38912,#38913) ;
#31390 = AXIS2_PLACEMENT_3D('',#48156,#38914,#38915) ;
#31391 = AXIS2_PLACEMENT_3D('',#48157,#38916,#38917) ;
#31392 = AXIS2_PLACEMENT_3D('',#48158,#38918,#38919) ;
#31393 = AXIS2_PLACEMENT_3D('',#48161,#38920,#38921) ;
#31394 = AXIS2_PLACEMENT_3D('',#48163,#38922,#38923) ;
#31395 = AXIS2_PLACEMENT_3D('',#48164,#38924,#38925) ;
#31396 = AXIS2_PLACEMENT_3D('',#48165,#38926,#38927) ;
#31397 = AXIS2_PLACEMENT_3D('',#48168,#38928,#38929) ;
#31398 = AXIS2_PLACEMENT_3D('',#48170,#38930,#38931) ;
#31399 = AXIS2_PLACEMENT_3D('',#48171,#38932,#38933) ;
#31400 = AXIS2_PLACEMENT_3D('',#48172,#38934,#38935) ;
#31401 = AXIS2_PLACEMENT_3D('',#48175,#38936,#38937) ;
#31402 = AXIS2_PLACEMENT_3D('',#48177,#38938,#38939) ;
#31403 = AXIS2_PLACEMENT_3D('',#48178,#38940,#38941) ;
#31404 = AXIS2_PLACEMENT_3D('',#48179,#38942,#38943) ;
#31405 = AXIS2_PLACEMENT_3D('',#48182,#38944,#38945) ;
#31406 = AXIS2_PLACEMENT_3D('',#48184,#38946,#38947) ;
#31407 = AXIS2_PLACEMENT_3D('',#48186,#38948,#38949) ;
#31408 = AXIS2_PLACEMENT_3D('',#48188,#38950,#38951) ;
#31409 = AXIS2_PLACEMENT_3D('',#48189,#38952,#38953) ;
#31410 = AXIS2_PLACEMENT_3D('',#48190,#38954,#38955) ;
#31411 = AXIS2_PLACEMENT_3D('',#48193,#38956,#38957) ;
#31412 = AXIS2_PLACEMENT_3D('',#48195,#38958,#38959) ;
#31413 = AXIS2_PLACEMENT_3D('',#48196,#38960,#38961) ;
#31414 = AXIS2_PLACEMENT_3D('',#48197,#38962,#38963) ;
#31415 = AXIS2_PLACEMENT_3D('',#48200,#38964,#38965) ;
#31416 = AXIS2_PLACEMENT_3D('',#48202,#38966,#38967) ;
#31417 = AXIS2_PLACEMENT_3D('',#48203,#38968,#38969) ;
#31418 = AXIS2_PLACEMENT_3D('',#48204,#38970,#38971) ;
#31419 = AXIS2_PLACEMENT_3D('',#48207,#38972,#38973) ;
#31420 = AXIS2_PLACEMENT_3D('',#48209,#38974,#38975) ;
#31421 = AXIS2_PLACEMENT_3D('',#48210,#38976,#38977) ;
#31422 = AXIS2_PLACEMENT_3D('',#48211,#38978,#38979) ;
#31423 = AXIS2_PLACEMENT_3D('',#48214,#38980,#38981) ;
#31424 = AXIS2_PLACEMENT_3D('',#48216,#38982,#38983) ;
#31425 = AXIS2_PLACEMENT_3D('',#48218,#38984,#38985) ;
#31426 = AXIS2_PLACEMENT_3D('',#48220,#38986,#38987) ;
#31427 = AXIS2_PLACEMENT_3D('',#48221,#38988,#38989) ;
#31428 = AXIS2_PLACEMENT_3D('',#48222,#38990,#38991) ;
#31429 = AXIS2_PLACEMENT_3D('',#48225,#38992,#38993) ;
#31430 = AXIS2_PLACEMENT_3D('',#48227,#38994,#38995) ;
#31431 = AXIS2_PLACEMENT_3D('',#48228,#38996,#38997) ;
#31432 = AXIS2_PLACEMENT_3D('',#48229,#38998,#38999) ;
#31433 = AXIS2_PLACEMENT_3D('',#48232,#39000,#39001) ;
#31434 = AXIS2_PLACEMENT_3D('',#48234,#39002,#39003) ;
#31435 = AXIS2_PLACEMENT_3D('',#48235,#39004,#39005) ;
#31436 = AXIS2_PLACEMENT_3D('',#48236,#39006,#39007) ;
#31437 = AXIS2_PLACEMENT_3D('',#48239,#39008,#39009) ;
#31438 = AXIS2_PLACEMENT_3D('',#48241,#39010,#39011) ;
#31439 = AXIS2_PLACEMENT_3D('',#48242,#39012,#39013) ;
#31440 = AXIS2_PLACEMENT_3D('',#48243,#39014,#39015) ;
#31441 = AXIS2_PLACEMENT_3D('',#48246,#39016,#39017) ;
#31442 = AXIS2_PLACEMENT_3D('',#48248,#39018,#39019) ;
#31443 = AXIS2_PLACEMENT_3D('',#48250,#39020,#39021) ;
#31444 = AXIS2_PLACEMENT_3D('',#48252,#39022,#39023) ;
#31445 = AXIS2_PLACEMENT_3D('',#48253,#39024,#39025) ;
#31446 = AXIS2_PLACEMENT_3D('',#48254,#39026,#39027) ;
#31447 = AXIS2_PLACEMENT_3D('',#48257,#39028,#39029) ;
#31448 = AXIS2_PLACEMENT_3D('',#48259,#39030,#39031) ;
#31449 = AXIS2_PLACEMENT_3D('',#48260,#39032,#39033) ;
#31450 = AXIS2_PLACEMENT_3D('',#48261,#39034,#39035) ;
#31451 = AXIS2_PLACEMENT_3D('',#48264,#39036,#39037) ;
#31452 = AXIS2_PLACEMENT_3D('',#48266,#39038,#39039) ;
#31453 = AXIS2_PLACEMENT_3D('',#48267,#39040,#39041) ;
#31454 = AXIS2_PLACEMENT_3D('',#48268,#39042,#39043) ;
#31455 = AXIS2_PLACEMENT_3D('',#48271,#39044,#39045) ;
#31456 = AXIS2_PLACEMENT_3D('',#48273,#39046,#39047) ;
#31457 = AXIS2_PLACEMENT_3D('',#48274,#39048,#39049) ;
#31458 = AXIS2_PLACEMENT_3D('',#48275,#39050,#39051) ;
#31459 = AXIS2_PLACEMENT_3D('',#48278,#39052,#39053) ;
#31460 = AXIS2_PLACEMENT_3D('',#48280,#39054,#39055) ;
#31461 = AXIS2_PLACEMENT_3D('',#48282,#39056,#39057) ;
#31462 = AXIS2_PLACEMENT_3D('',#48284,#39058,#39059) ;
#31463 = AXIS2_PLACEMENT_3D('',#48285,#39060,#39061) ;
#31464 = AXIS2_PLACEMENT_3D('',#48286,#39062,#39063) ;
#31465 = AXIS2_PLACEMENT_3D('',#48289,#39064,#39065) ;
#31466 = AXIS2_PLACEMENT_3D('',#48291,#39066,#39067) ;
#31467 = AXIS2_PLACEMENT_3D('',#48292,#39068,#39069) ;
#31468 = AXIS2_PLACEMENT_3D('',#48293,#39070,#39071) ;
#31469 = AXIS2_PLACEMENT_3D('',#48296,#39072,#39073) ;
#31470 = AXIS2_PLACEMENT_3D('',#48298,#39074,#39075) ;
#31471 = AXIS2_PLACEMENT_3D('',#48299,#39076,#39077) ;
#31472 = AXIS2_PLACEMENT_3D('',#48300,#39078,#39079) ;
#31473 = AXIS2_PLACEMENT_3D('',#48303,#39080,#39081) ;
#31474 = AXIS2_PLACEMENT_3D('',#48305,#39082,#39083) ;
#31475 = AXIS2_PLACEMENT_3D('',#48306,#39084,#39085) ;
#31476 = AXIS2_PLACEMENT_3D('',#48307,#39086,#39087) ;
#31477 = AXIS2_PLACEMENT_3D('',#48310,#39088,#39089) ;
#31478 = AXIS2_PLACEMENT_3D('',#48312,#39090,#39091) ;
#31479 = AXIS2_PLACEMENT_3D('',#48314,#39092,#39093) ;
#31480 = AXIS2_PLACEMENT_3D('',#48316,#39094,#39095) ;
#31481 = AXIS2_PLACEMENT_3D('',#48317,#39096,#39097) ;
#31482 = AXIS2_PLACEMENT_3D('',#48318,#39098,#39099) ;
#31483 = AXIS2_PLACEMENT_3D('',#48321,#39100,#39101) ;
#31484 = AXIS2_PLACEMENT_3D('',#48323,#39102,#39103) ;
#31485 = AXIS2_PLACEMENT_3D('',#48324,#39104,#39105) ;
#31486 = AXIS2_PLACEMENT_3D('',#48325,#39106,#39107) ;
#31487 = AXIS2_PLACEMENT_3D('',#48328,#39108,#39109) ;
#31488 = AXIS2_PLACEMENT_3D('',#48330,#39110,#39111) ;
#31489 = AXIS2_PLACEMENT_3D('',#48331,#39112,#39113) ;
#31490 = AXIS2_PLACEMENT_3D('',#48332,#39114,#39115) ;
#31491 = AXIS2_PLACEMENT_3D('',#48335,#39116,#39117) ;
#31492 = AXIS2_PLACEMENT_3D('',#48337,#39118,#39119) ;
#31493 = AXIS2_PLACEMENT_3D('',#48338,#39120,#39121) ;
#31494 = AXIS2_PLACEMENT_3D('',#48339,#39122,#39123) ;
#31495 = AXIS2_PLACEMENT_3D('',#48342,#39124,#39125) ;
#31496 = AXIS2_PLACEMENT_3D('',#48344,#39126,#39127) ;
#31497 = AXIS2_PLACEMENT_3D('',#48346,#39128,#39129) ;
#31498 = AXIS2_PLACEMENT_3D('',#48348,#39130,#39131) ;
#31499 = AXIS2_PLACEMENT_3D('',#48349,#39132,#39133) ;
#31500 = AXIS2_PLACEMENT_3D('',#48350,#39134,#39135) ;
#31501 = AXIS2_PLACEMENT_3D('',#48353,#39136,#39137) ;
#31502 = AXIS2_PLACEMENT_3D('',#48355,#39138,#39139) ;
#31503 = AXIS2_PLACEMENT_3D('',#48356,#39140,#39141) ;
#31504 = AXIS2_PLACEMENT_3D('',#48357,#39142,#39143) ;
#31505 = AXIS2_PLACEMENT_3D('',#48360,#39144,#39145) ;
#31506 = AXIS2_PLACEMENT_3D('',#48362,#39146,#39147) ;
#31507 = AXIS2_PLACEMENT_3D('',#48363,#39148,#39149) ;
#31508 = AXIS2_PLACEMENT_3D('',#48364,#39150,#39151) ;
#31509 = AXIS2_PLACEMENT_3D('',#48367,#39152,#39153) ;
#31510 = AXIS2_PLACEMENT_3D('',#48369,#39154,#39155) ;
#31511 = AXIS2_PLACEMENT_3D('',#48370,#39156,#39157) ;
#31512 = AXIS2_PLACEMENT_3D('',#48371,#39158,#39159) ;
#31513 = AXIS2_PLACEMENT_3D('',#48374,#39160,#39161) ;
#31514 = AXIS2_PLACEMENT_3D('',#48376,#39162,#39163) ;
#31515 = AXIS2_PLACEMENT_3D('',#48378,#39164,#39165) ;
#31516 = AXIS2_PLACEMENT_3D('',#48380,#39166,#39167) ;
#31517 = AXIS2_PLACEMENT_3D('',#48381,#39168,#39169) ;
#31518 = AXIS2_PLACEMENT_3D('',#48382,#39170,#39171) ;
#31519 = AXIS2_PLACEMENT_3D('',#48385,#39172,#39173) ;
#31520 = AXIS2_PLACEMENT_3D('',#48387,#39174,#39175) ;
#31521 = AXIS2_PLACEMENT_3D('',#48388,#39176,#39177) ;
#31522 = AXIS2_PLACEMENT_3D('',#48389,#39178,#39179) ;
#31523 = AXIS2_PLACEMENT_3D('',#48392,#39180,#39181) ;
#31524 = AXIS2_PLACEMENT_3D('',#48394,#39182,#39183) ;
#31525 = AXIS2_PLACEMENT_3D('',#48395,#39184,#39185) ;
#31526 = AXIS2_PLACEMENT_3D('',#48396,#39186,#39187) ;
#31527 = AXIS2_PLACEMENT_3D('',#48399,#39188,#39189) ;
#31528 = AXIS2_PLACEMENT_3D('',#48401,#39190,#39191) ;
#31529 = AXIS2_PLACEMENT_3D('',#48402,#39192,#39193) ;
#31530 = AXIS2_PLACEMENT_3D('',#48403,#39194,#39195) ;
#31531 = AXIS2_PLACEMENT_3D('',#48406,#39196,#39197) ;
#31532 = AXIS2_PLACEMENT_3D('',#48408,#39198,#39199) ;
#31533 = AXIS2_PLACEMENT_3D('',#48410,#39200,#39201) ;
#31534 = AXIS2_PLACEMENT_3D('',#48412,#39202,#39203) ;
#31535 = AXIS2_PLACEMENT_3D('',#48413,#39204,#39205) ;
#31536 = AXIS2_PLACEMENT_3D('',#48414,#39206,#39207) ;
#31537 = AXIS2_PLACEMENT_3D('',#48417,#39208,#39209) ;
#31538 = AXIS2_PLACEMENT_3D('',#48419,#39210,#39211) ;
#31539 = AXIS2_PLACEMENT_3D('',#48420,#39212,#39213) ;
#31540 = AXIS2_PLACEMENT_3D('',#48421,#39214,#39215) ;
#31541 = AXIS2_PLACEMENT_3D('',#48424,#39216,#39217) ;
#31542 = AXIS2_PLACEMENT_3D('',#48426,#39218,#39219) ;
#31543 = AXIS2_PLACEMENT_3D('',#48427,#39220,#39221) ;
#31544 = AXIS2_PLACEMENT_3D('',#48428,#39222,#39223) ;
#31545 = AXIS2_PLACEMENT_3D('',#48431,#39224,#39225) ;
#31546 = AXIS2_PLACEMENT_3D('',#48433,#39226,#39227) ;
#31547 = AXIS2_PLACEMENT_3D('',#48434,#39228,#39229) ;
#31548 = AXIS2_PLACEMENT_3D('',#48435,#39230,#39231) ;
#31549 = AXIS2_PLACEMENT_3D('',#48438,#39232,#39233) ;
#31550 = AXIS2_PLACEMENT_3D('',#48440,#39234,#39235) ;
#31551 = AXIS2_PLACEMENT_3D('',#48442,#39236,#39237) ;
#31552 = AXIS2_PLACEMENT_3D('',#48444,#39238,#39239) ;
#31553 = AXIS2_PLACEMENT_3D('',#48445,#39240,#39241) ;
#31554 = AXIS2_PLACEMENT_3D('',#48446,#39242,#39243) ;
#31555 = AXIS2_PLACEMENT_3D('',#48449,#39244,#39245) ;
#31556 = AXIS2_PLACEMENT_3D('',#48451,#39246,#39247) ;
#31557 = AXIS2_PLACEMENT_3D('',#48452,#39248,#39249) ;
#31558 = AXIS2_PLACEMENT_3D('',#48453,#39250,#39251) ;
#31559 = AXIS2_PLACEMENT_3D('',#48456,#39252,#39253) ;
#31560 = AXIS2_PLACEMENT_3D('',#48458,#39254,#39255) ;
#31561 = AXIS2_PLACEMENT_3D('',#48459,#39256,#39257) ;
#31562 = AXIS2_PLACEMENT_3D('',#48460,#39258,#39259) ;
#31563 = AXIS2_PLACEMENT_3D('',#48463,#39260,#39261) ;
#31564 = AXIS2_PLACEMENT_3D('',#48465,#39262,#39263) ;
#31565 = AXIS2_PLACEMENT_3D('',#48466,#39264,#39265) ;
#31566 = AXIS2_PLACEMENT_3D('',#48467,#39266,#39267) ;
#31567 = AXIS2_PLACEMENT_3D('',#48470,#39268,#39269) ;
#31568 = AXIS2_PLACEMENT_3D('',#48472,#39270,#39271) ;
#31569 = AXIS2_PLACEMENT_3D('',#48474,#39272,#39273) ;
#31570 = AXIS2_PLACEMENT_3D('',#48476,#39274,#39275) ;
#31571 = AXIS2_PLACEMENT_3D('',#48477,#39276,#39277) ;
#31572 = AXIS2_PLACEMENT_3D('',#48478,#39278,#39279) ;
#31573 = AXIS2_PLACEMENT_3D('',#48481,#39280,#39281) ;
#31574 = AXIS2_PLACEMENT_3D('',#48483,#39282,#39283) ;
#31575 = AXIS2_PLACEMENT_3D('',#48484,#39284,#39285) ;
#31576 = AXIS2_PLACEMENT_3D('',#48485,#39286,#39287) ;
#31577 = AXIS2_PLACEMENT_3D('',#48488,#39288,#39289) ;
#31578 = AXIS2_PLACEMENT_3D('',#48490,#39290,#39291) ;
#31579 = AXIS2_PLACEMENT_3D('',#48491,#39292,#39293) ;
#31580 = AXIS2_PLACEMENT_3D('',#48492,#39294,#39295) ;
#31581 = AXIS2_PLACEMENT_3D('',#48495,#39296,#39297) ;
#31582 = AXIS2_PLACEMENT_3D('',#48497,#39298,#39299) ;
#31583 = AXIS2_PLACEMENT_3D('',#48498,#39300,#39301) ;
#31584 = AXIS2_PLACEMENT_3D('',#48499,#39302,#39303) ;
#31585 = AXIS2_PLACEMENT_3D('',#48502,#39304,#39305) ;
#31586 = AXIS2_PLACEMENT_3D('',#48504,#39306,#39307) ;
#31587 = AXIS2_PLACEMENT_3D('',#48506,#39308,#39309) ;
#31588 = AXIS2_PLACEMENT_3D('',#48508,#39310,#39311) ;
#31589 = AXIS2_PLACEMENT_3D('',#48509,#39312,#39313) ;
#31590 = AXIS2_PLACEMENT_3D('',#48510,#39314,#39315) ;
#31591 = AXIS2_PLACEMENT_3D('',#48513,#39316,#39317) ;
#31592 = AXIS2_PLACEMENT_3D('',#48515,#39318,#39319) ;
#31593 = AXIS2_PLACEMENT_3D('',#48516,#39320,#39321) ;
#31594 = AXIS2_PLACEMENT_3D('',#48517,#39322,#39323) ;
#31595 = AXIS2_PLACEMENT_3D('',#48520,#39324,#39325) ;
#31596 = AXIS2_PLACEMENT_3D('',#48522,#39326,#39327) ;
#31597 = AXIS2_PLACEMENT_3D('',#48523,#39328,#39329) ;
#31598 = AXIS2_PLACEMENT_3D('',#48524,#39330,#39331) ;
#31599 = AXIS2_PLACEMENT_3D('',#48527,#39332,#39333) ;
#31600 = AXIS2_PLACEMENT_3D('',#48529,#39334,#39335) ;
#31601 = AXIS2_PLACEMENT_3D('',#48530,#39336,#39337) ;
#31602 = AXIS2_PLACEMENT_3D('',#48531,#39338,#39339) ;
#31603 = AXIS2_PLACEMENT_3D('',#48534,#39340,#39341) ;
#31604 = AXIS2_PLACEMENT_3D('',#48536,#39342,#39343) ;
#31605 = AXIS2_PLACEMENT_3D('',#48538,#39344,#39345) ;
#31606 = AXIS2_PLACEMENT_3D('',#48540,#39346,#39347) ;
#31607 = AXIS2_PLACEMENT_3D('',#48541,#39348,#39349) ;
#31608 = AXIS2_PLACEMENT_3D('',#48542,#39350,#39351) ;
#31609 = AXIS2_PLACEMENT_3D('',#48545,#39352,#39353) ;
#31610 = AXIS2_PLACEMENT_3D('',#48547,#39354,#39355) ;
#31611 = AXIS2_PLACEMENT_3D('',#48548,#39356,#39357) ;
#31612 = AXIS2_PLACEMENT_3D('',#48549,#39358,#39359) ;
#31613 = AXIS2_PLACEMENT_3D('',#48552,#39360,#39361) ;
#31614 = AXIS2_PLACEMENT_3D('',#48554,#39362,#39363) ;
#31615 = AXIS2_PLACEMENT_3D('',#48555,#39364,#39365) ;
#31616 = AXIS2_PLACEMENT_3D('',#48556,#39366,#39367) ;
#31617 = AXIS2_PLACEMENT_3D('',#48559,#39368,#39369) ;
#31618 = AXIS2_PLACEMENT_3D('',#48561,#39370,#39371) ;
#31619 = AXIS2_PLACEMENT_3D('',#48562,#39372,#39373) ;
#31620 = AXIS2_PLACEMENT_3D('',#48563,#39374,#39375) ;
#31621 = AXIS2_PLACEMENT_3D('',#48566,#39376,#39377) ;
#31622 = AXIS2_PLACEMENT_3D('',#48568,#39378,#39379) ;
#31623 = AXIS2_PLACEMENT_3D('',#48570,#39380,#39381) ;
#31624 = AXIS2_PLACEMENT_3D('',#48572,#39382,#39383) ;
#31625 = AXIS2_PLACEMENT_3D('',#48573,#39384,#39385) ;
#31626 = AXIS2_PLACEMENT_3D('',#48574,#39386,#39387) ;
#31627 = AXIS2_PLACEMENT_3D('',#48577,#39388,#39389) ;
#31628 = AXIS2_PLACEMENT_3D('',#48579,#39390,#39391) ;
#31629 = AXIS2_PLACEMENT_3D('',#48580,#39392,#39393) ;
#31630 = AXIS2_PLACEMENT_3D('',#48581,#39394,#39395) ;
#31631 = AXIS2_PLACEMENT_3D('',#48584,#39396,#39397) ;
#31632 = AXIS2_PLACEMENT_3D('',#48586,#39398,#39399) ;
#31633 = AXIS2_PLACEMENT_3D('',#48587,#39400,#39401) ;
#31634 = AXIS2_PLACEMENT_3D('',#48588,#39402,#39403) ;
#31635 = AXIS2_PLACEMENT_3D('',#48591,#39404,#39405) ;
#31636 = AXIS2_PLACEMENT_3D('',#48593,#39406,#39407) ;
#31637 = AXIS2_PLACEMENT_3D('',#48594,#39408,#39409) ;
#31638 = AXIS2_PLACEMENT_3D('',#48595,#39410,#39411) ;
#31639 = AXIS2_PLACEMENT_3D('',#48598,#39412,#39413) ;
#31640 = AXIS2_PLACEMENT_3D('',#48600,#39414,#39415) ;
#31641 = AXIS2_PLACEMENT_3D('',#48602,#39416,#39417) ;
#31642 = AXIS2_PLACEMENT_3D('',#48604,#39418,#39419) ;
#31643 = AXIS2_PLACEMENT_3D('',#48605,#39420,#39421) ;
#31644 = AXIS2_PLACEMENT_3D('',#48606,#39422,#39423) ;
#31645 = AXIS2_PLACEMENT_3D('',#48609,#39424,#39425) ;
#31646 = AXIS2_PLACEMENT_3D('',#48611,#39426,#39427) ;
#31647 = AXIS2_PLACEMENT_3D('',#48612,#39428,#39429) ;
#31648 = AXIS2_PLACEMENT_3D('',#48613,#39430,#39431) ;
#31649 = AXIS2_PLACEMENT_3D('',#48616,#39432,#39433) ;
#31650 = AXIS2_PLACEMENT_3D('',#48618,#39434,#39435) ;
#31651 = AXIS2_PLACEMENT_3D('',#48619,#39436,#39437) ;
#31652 = AXIS2_PLACEMENT_3D('',#48620,#39438,#39439) ;
#31653 = AXIS2_PLACEMENT_3D('',#48623,#39440,#39441) ;
#31654 = AXIS2_PLACEMENT_3D('',#48625,#39442,#39443) ;
#31655 = AXIS2_PLACEMENT_3D('',#48626,#39444,#39445) ;
#31656 = AXIS2_PLACEMENT_3D('',#48627,#39446,#39447) ;
#31657 = AXIS2_PLACEMENT_3D('',#48630,#39448,#39449) ;
#31658 = AXIS2_PLACEMENT_3D('',#48632,#39450,#39451) ;
#31659 = AXIS2_PLACEMENT_3D('',#48634,#39452,#39453) ;
#31660 = AXIS2_PLACEMENT_3D('',#48636,#39454,#39455) ;
#31661 = AXIS2_PLACEMENT_3D('',#48637,#39456,#39457) ;
#31662 = AXIS2_PLACEMENT_3D('',#48638,#39458,#39459) ;
#31663 = AXIS2_PLACEMENT_3D('',#48641,#39460,#39461) ;
#31664 = AXIS2_PLACEMENT_3D('',#48643,#39462,#39463) ;
#31665 = AXIS2_PLACEMENT_3D('',#48644,#39464,#39465) ;
#31666 = AXIS2_PLACEMENT_3D('',#48645,#39466,#39467) ;
#31667 = AXIS2_PLACEMENT_3D('',#48648,#39468,#39469) ;
#31668 = AXIS2_PLACEMENT_3D('',#48650,#39470,#39471) ;
#31669 = AXIS2_PLACEMENT_3D('',#48651,#39472,#39473) ;
#31670 = AXIS2_PLACEMENT_3D('',#48652,#39474,#39475) ;
#31671 = AXIS2_PLACEMENT_3D('',#48655,#39476,#39477) ;
#31672 = AXIS2_PLACEMENT_3D('',#48657,#39478,#39479) ;
#31673 = AXIS2_PLACEMENT_3D('',#48658,#39480,#39481) ;
#31674 = AXIS2_PLACEMENT_3D('',#48659,#39482,#39483) ;
#31675 = AXIS2_PLACEMENT_3D('',#48660,#39484,#39485) ;
#31676 = AXIS2_PLACEMENT_3D('',#48661,#39486,#39487) ;
#31677 = AXIS2_PLACEMENT_3D('',#48662,#39488,#39489) ;
#31678 = AXIS2_PLACEMENT_3D('',#48663,#39490,#39491) ;
#31679 = AXIS2_PLACEMENT_3D('',#48666,#39493,#39494) ;
#31680 = AXIS2_PLACEMENT_3D('',#48667,#39495,#39496) ;
#31681 = AXIS2_PLACEMENT_3D('',#48668,#39497,#39498) ;
#31682 = AXIS2_PLACEMENT_3D('',#48671,#39500,#39501) ;
#31683 = AXIS2_PLACEMENT_3D('',#48672,#39502,#39503) ;
#31684 = AXIS2_PLACEMENT_3D('',#48673,#39504,#39505) ;
#31685 = AXIS2_PLACEMENT_3D('',#48676,#39507,#39508) ;
#31686 = AXIS2_PLACEMENT_3D('',#48677,#39509,#39510) ;
#31687 = AXIS2_PLACEMENT_3D('',#48678,#39511,#39512) ;
#31688 = AXIS2_PLACEMENT_3D('',#48681,#39514,#39515) ;
#31689 = AXIS2_PLACEMENT_3D('',#48682,#39516,#39517) ;
#31690 = AXIS2_PLACEMENT_3D('',#48683,#39518,#39519) ;
#31691 = AXIS2_PLACEMENT_3D('',#48686,#39521,#39522) ;
#31692 = AXIS2_PLACEMENT_3D('',#48687,#39523,#39524) ;
#31693 = AXIS2_PLACEMENT_3D('',#48688,#39525,#39526) ;
#31694 = AXIS2_PLACEMENT_3D('',#48691,#39528,#39529) ;
#31695 = AXIS2_PLACEMENT_3D('',#48692,#39530,#39531) ;
#31696 = AXIS2_PLACEMENT_3D('',#48693,#39532,#39533) ;
#31697 = AXIS2_PLACEMENT_3D('',#48696,#39535,#39536) ;
#31698 = AXIS2_PLACEMENT_3D('',#48697,#39537,#39538) ;
#31699 = AXIS2_PLACEMENT_3D('',#48698,#39539,#39540) ;
#31700 = AXIS2_PLACEMENT_3D('',#48701,#39542,#39543) ;
#31701 = AXIS2_PLACEMENT_3D('',#48702,#39544,#39545) ;
#31702 = AXIS2_PLACEMENT_3D('',#48703,#39546,#39547) ;
#31703 = AXIS2_PLACEMENT_3D('',#48706,#39549,#39550) ;
#31704 = AXIS2_PLACEMENT_3D('',#48707,#39551,#39552) ;
#31705 = AXIS2_PLACEMENT_3D('',#48708,#39553,#39554) ;
#31706 = AXIS2_PLACEMENT_3D('',#48711,#39556,#39557) ;
#31707 = AXIS2_PLACEMENT_3D('',#48712,#39558,#39559) ;
#31708 = AXIS2_PLACEMENT_3D('',#48713,#39560,#39561) ;
#31709 = AXIS2_PLACEMENT_3D('',#48716,#39563,#39564) ;
#31710 = AXIS2_PLACEMENT_3D('',#48717,#39565,#39566) ;
#31711 = AXIS2_PLACEMENT_3D('',#48718,#39567,#39568) ;
#31712 = AXIS2_PLACEMENT_3D('',#48721,#39570,#39571) ;
#31713 = AXIS2_PLACEMENT_3D('',#48722,#39572,#39573) ;
#31714 = AXIS2_PLACEMENT_3D('',#48723,#39574,#39575) ;
#31715 = AXIS2_PLACEMENT_3D('',#48726,#39577,#39578) ;
#31716 = AXIS2_PLACEMENT_3D('',#48727,#39579,#39580) ;
#31717 = AXIS2_PLACEMENT_3D('',#48728,#39581,#39582) ;
#31718 = AXIS2_PLACEMENT_3D('',#48731,#39584,#39585) ;
#31719 = AXIS2_PLACEMENT_3D('',#48732,#39586,#39587) ;
#31720 = AXIS2_PLACEMENT_3D('',#48733,#39588,#39589) ;
#31721 = AXIS2_PLACEMENT_3D('',#48736,#39591,#39592) ;
#31722 = AXIS2_PLACEMENT_3D('',#48737,#39593,#39594) ;
#31723 = AXIS2_PLACEMENT_3D('',#48738,#39595,#39596) ;
#31724 = AXIS2_PLACEMENT_3D('',#48741,#39598,#39599) ;
#31725 = AXIS2_PLACEMENT_3D('',#48742,#39600,#39601) ;
#31726 = AXIS2_PLACEMENT_3D('',#48743,#39602,#39603) ;
#31727 = AXIS2_PLACEMENT_3D('',#48746,#39605,#39606) ;
#31728 = AXIS2_PLACEMENT_3D('',#48747,#39607,#39608) ;
#31729 = AXIS2_PLACEMENT_3D('',#48748,#39609,#39610) ;
#31730 = AXIS2_PLACEMENT_3D('',#48751,#39612,#39613) ;
#31731 = AXIS2_PLACEMENT_3D('',#48752,#39614,#39615) ;
#31732 = AXIS2_PLACEMENT_3D('',#48753,#39616,#39617) ;
#31733 = AXIS2_PLACEMENT_3D('',#48756,#39619,#39620) ;
#31734 = AXIS2_PLACEMENT_3D('',#48757,#39621,#39622) ;
#31735 = AXIS2_PLACEMENT_3D('',#48758,#39623,#39624) ;
#31736 = AXIS2_PLACEMENT_3D('',#48761,#39626,#39627) ;
#31737 = AXIS2_PLACEMENT_3D('',#48762,#39628,#39629) ;
#31738 = AXIS2_PLACEMENT_3D('',#48763,#39630,#39631) ;
#31739 = AXIS2_PLACEMENT_3D('',#48766,#39633,#39634) ;
#31740 = AXIS2_PLACEMENT_3D('',#48767,#39635,#39636) ;
#31741 = AXIS2_PLACEMENT_3D('',#48768,#39637,#39638) ;
#31742 = AXIS2_PLACEMENT_3D('',#48771,#39640,#39641) ;
#31743 = AXIS2_PLACEMENT_3D('',#48772,#39642,#39643) ;
#31744 = AXIS2_PLACEMENT_3D('',#48773,#39644,#39645) ;
#31745 = AXIS2_PLACEMENT_3D('',#48776,#39647,#39648) ;
#31746 = AXIS2_PLACEMENT_3D('',#48777,#39649,#39650) ;
#31747 = AXIS2_PLACEMENT_3D('',#48778,#39651,#39652) ;
#31748 = AXIS2_PLACEMENT_3D('',#48781,#39654,#39655) ;
#31749 = AXIS2_PLACEMENT_3D('',#48782,#39656,#39657) ;
#31750 = AXIS2_PLACEMENT_3D('',#48783,#39658,#39659) ;
#31751 = AXIS2_PLACEMENT_3D('',#48786,#39661,#39662) ;
#31752 = AXIS2_PLACEMENT_3D('',#48787,#39663,#39664) ;
#31753 = AXIS2_PLACEMENT_3D('',#48788,#39665,#39666) ;
#31754 = AXIS2_PLACEMENT_3D('',#48791,#39668,#39669) ;
#31755 = AXIS2_PLACEMENT_3D('',#48792,#39670,#39671) ;
#31756 = AXIS2_PLACEMENT_3D('',#48793,#39672,#39673) ;
#31757 = AXIS2_PLACEMENT_3D('',#48796,#39675,#39676) ;
#31758 = AXIS2_PLACEMENT_3D('',#48797,#39677,#39678) ;
#31759 = AXIS2_PLACEMENT_3D('',#48798,#39679,#39680) ;
#31760 = AXIS2_PLACEMENT_3D('',#48801,#39682,#39683) ;
#31761 = AXIS2_PLACEMENT_3D('',#48802,#39684,#39685) ;
#31762 = AXIS2_PLACEMENT_3D('',#48803,#39686,#39687) ;
#31763 = AXIS2_PLACEMENT_3D('',#48806,#39689,#39690) ;
#31764 = AXIS2_PLACEMENT_3D('',#48807,#39691,#39692) ;
#31765 = AXIS2_PLACEMENT_3D('',#48808,#39693,#39694) ;
#31766 = AXIS2_PLACEMENT_3D('',#48811,#39696,#39697) ;
#31767 = AXIS2_PLACEMENT_3D('',#48812,#39698,#39699) ;
#31768 = AXIS2_PLACEMENT_3D('',#48813,#39700,#39701) ;
#31769 = AXIS2_PLACEMENT_3D('',#48816,#39703,#39704) ;
#31770 = AXIS2_PLACEMENT_3D('',#48817,#39705,#39706) ;
#31771 = AXIS2_PLACEMENT_3D('',#48818,#39707,#39708) ;
#31772 = AXIS2_PLACEMENT_3D('',#48821,#39710,#39711) ;
#31773 = AXIS2_PLACEMENT_3D('',#48822,#39712,#39713) ;
#31774 = AXIS2_PLACEMENT_3D('',#48823,#39714,#39715) ;
#31775 = AXIS2_PLACEMENT_3D('',#48826,#39717,#39718) ;
#31776 = AXIS2_PLACEMENT_3D('',#48827,#39719,#39720) ;
#31777 = AXIS2_PLACEMENT_3D('',#48828,#39721,#39722) ;
#31778 = AXIS2_PLACEMENT_3D('',#48831,#39724,#39725) ;
#31779 = AXIS2_PLACEMENT_3D('',#48832,#39726,#39727) ;
#31780 = AXIS2_PLACEMENT_3D('',#48833,#39728,#39729) ;
#31781 = AXIS2_PLACEMENT_3D('',#48836,#39731,#39732) ;
#31782 = AXIS2_PLACEMENT_3D('',#48837,#39733,#39734) ;
#31783 = AXIS2_PLACEMENT_3D('',#48838,#39735,#39736) ;
#31784 = AXIS2_PLACEMENT_3D('',#48841,#39738,#39739) ;
#31785 = AXIS2_PLACEMENT_3D('',#48842,#39740,#39741) ;
#31786 = AXIS2_PLACEMENT_3D('',#48843,#39742,#39743) ;
#31787 = AXIS2_PLACEMENT_3D('',#48846,#39745,#39746) ;
#31788 = AXIS2_PLACEMENT_3D('',#48847,#39747,#39748) ;
#31789 = AXIS2_PLACEMENT_3D('',#48848,#39749,#39750) ;
#31790 = AXIS2_PLACEMENT_3D('',#48851,#39752,#39753) ;
#31791 = AXIS2_PLACEMENT_3D('',#48852,#39754,#39755) ;
#31792 = AXIS2_PLACEMENT_3D('',#48853,#39756,#39757) ;
#31793 = AXIS2_PLACEMENT_3D('',#48856,#39759,#39760) ;
#31794 = AXIS2_PLACEMENT_3D('',#48857,#39761,#39762) ;
#31795 = AXIS2_PLACEMENT_3D('',#48858,#39763,#39764) ;
#31796 = AXIS2_PLACEMENT_3D('',#48861,#39766,#39767) ;
#31797 = AXIS2_PLACEMENT_3D('',#48862,#39768,#39769) ;
#31798 = AXIS2_PLACEMENT_3D('',#48863,#39770,#39771) ;
#31799 = AXIS2_PLACEMENT_3D('',#48866,#39773,#39774) ;
#31800 = AXIS2_PLACEMENT_3D('',#48867,#39775,#39776) ;
#31801 = AXIS2_PLACEMENT_3D('',#48868,#39777,#39778) ;
#31802 = AXIS2_PLACEMENT_3D('',#48871,#39780,#39781) ;
#31803 = AXIS2_PLACEMENT_3D('',#48872,#39782,#39783) ;
#31804 = AXIS2_PLACEMENT_3D('',#48873,#39784,#39785) ;
#31805 = AXIS2_PLACEMENT_3D('',#48876,#39787,#39788) ;
#31806 = AXIS2_PLACEMENT_3D('',#48877,#39789,#39790) ;
#31807 = AXIS2_PLACEMENT_3D('',#48878,#39791,#39792) ;
#31808 = AXIS2_PLACEMENT_3D('',#48881,#39794,#39795) ;
#31809 = AXIS2_PLACEMENT_3D('',#48882,#39796,#39797) ;
#31810 = AXIS2_PLACEMENT_3D('',#48883,#39798,#39799) ;
#31811 = AXIS2_PLACEMENT_3D('',#48886,#39801,#39802) ;
#31812 = AXIS2_PLACEMENT_3D('',#48887,#39803,#39804) ;
#31813 = AXIS2_PLACEMENT_3D('',#48888,#39805,#39806) ;
#31814 = AXIS2_PLACEMENT_3D('',#48891,#39808,#39809) ;
#31815 = AXIS2_PLACEMENT_3D('',#48892,#39810,#39811) ;
#31816 = AXIS2_PLACEMENT_3D('',#48893,#39812,#39813) ;
#31817 = AXIS2_PLACEMENT_3D('',#48896,#39815,#39816) ;
#31818 = AXIS2_PLACEMENT_3D('',#48897,#39817,#39818) ;
#31819 = AXIS2_PLACEMENT_3D('',#48898,#39819,#39820) ;
#31820 = AXIS2_PLACEMENT_3D('',#48901,#39822,#39823) ;
#31821 = AXIS2_PLACEMENT_3D('',#48902,#39824,#39825) ;
#31822 = AXIS2_PLACEMENT_3D('',#48903,#39826,#39827) ;
#31823 = AXIS2_PLACEMENT_3D('',#48906,#39829,#39830) ;
#31824 = AXIS2_PLACEMENT_3D('',#48907,#39831,#39832) ;
#31825 = AXIS2_PLACEMENT_3D('',#48908,#39833,#39834) ;
#31826 = AXIS2_PLACEMENT_3D('',#48911,#39836,#39837) ;
#31827 = AXIS2_PLACEMENT_3D('',#48912,#39838,#39839) ;
#31828 = AXIS2_PLACEMENT_3D('',#48913,#39840,#39841) ;
#31829 = AXIS2_PLACEMENT_3D('',#48916,#39843,#39844) ;
#31830 = AXIS2_PLACEMENT_3D('',#48917,#39845,#39846) ;
#31831 = AXIS2_PLACEMENT_3D('',#48918,#39847,#39848) ;
#31832 = AXIS2_PLACEMENT_3D('',#48921,#39850,#39851) ;
#31833 = AXIS2_PLACEMENT_3D('',#48922,#39852,#39853) ;
#31834 = AXIS2_PLACEMENT_3D('',#48923,#39854,#39855) ;
#31835 = AXIS2_PLACEMENT_3D('',#48926,#39857,#39858) ;
#31836 = AXIS2_PLACEMENT_3D('',#48927,#39859,#39860) ;
#31837 = AXIS2_PLACEMENT_3D('',#48928,#39861,#39862) ;
#31838 = AXIS2_PLACEMENT_3D('',#48931,#39864,#39865) ;
#31839 = AXIS2_PLACEMENT_3D('',#48932,#39866,#39867) ;
#31840 = AXIS2_PLACEMENT_3D('',#48933,#39868,#39869) ;
#31841 = AXIS2_PLACEMENT_3D('',#48936,#39871,#39872) ;
#31842 = AXIS2_PLACEMENT_3D('',#48937,#39873,#39874) ;
#31843 = AXIS2_PLACEMENT_3D('',#48938,#39875,#39876) ;
#31844 = AXIS2_PLACEMENT_3D('',#48941,#39878,#39879) ;
#31845 = AXIS2_PLACEMENT_3D('',#48942,#39880,#39881) ;
#31846 = AXIS2_PLACEMENT_3D('',#48943,#39882,#39883) ;
#31847 = AXIS2_PLACEMENT_3D('',#48946,#39885,#39886) ;
#31848 = AXIS2_PLACEMENT_3D('',#48947,#39887,#39888) ;
#31849 = AXIS2_PLACEMENT_3D('',#48948,#39889,#39890) ;
#31850 = AXIS2_PLACEMENT_3D('',#48951,#39892,#39893) ;
#31851 = AXIS2_PLACEMENT_3D('',#48952,#39894,#39895) ;
#31852 = AXIS2_PLACEMENT_3D('',#48953,#39896,#39897) ;
#31853 = AXIS2_PLACEMENT_3D('',#48956,#39899,#39900) ;
#31854 = AXIS2_PLACEMENT_3D('',#48957,#39901,#39902) ;
#31855 = AXIS2_PLACEMENT_3D('',#48958,#39903,#39904) ;
#31856 = AXIS2_PLACEMENT_3D('',#48961,#39906,#39907) ;
#31857 = AXIS2_PLACEMENT_3D('',#48962,#39908,#39909) ;
#31858 = AXIS2_PLACEMENT_3D('',#48963,#39910,#39911) ;
#31859 = AXIS2_PLACEMENT_3D('',#48966,#39913,#39914) ;
#31860 = AXIS2_PLACEMENT_3D('',#48967,#39915,#39916) ;
#31861 = AXIS2_PLACEMENT_3D('',#48968,#39917,#39918) ;
#31862 = AXIS2_PLACEMENT_3D('',#48971,#39920,#39921) ;
#31863 = AXIS2_PLACEMENT_3D('',#48972,#39922,#39923) ;
#31864 = AXIS2_PLACEMENT_3D('',#48973,#39924,#39925) ;
#31865 = AXIS2_PLACEMENT_3D('',#48976,#39927,#39928) ;
#31866 = AXIS2_PLACEMENT_3D('',#48977,#39929,#39930) ;
#31867 = AXIS2_PLACEMENT_3D('',#48978,#39931,#39932) ;
#31868 = AXIS2_PLACEMENT_3D('',#48981,#39934,#39935) ;
#31869 = AXIS2_PLACEMENT_3D('',#48982,#39936,#39937) ;
#31870 = AXIS2_PLACEMENT_3D('',#48983,#39938,#39939) ;
#31871 = AXIS2_PLACEMENT_3D('',#48986,#39941,#39942) ;
#31872 = AXIS2_PLACEMENT_3D('',#48987,#39943,#39944) ;
#31873 = AXIS2_PLACEMENT_3D('',#48988,#39945,#39946) ;
#31874 = AXIS2_PLACEMENT_3D('',#48991,#39948,#39949) ;
#31875 = AXIS2_PLACEMENT_3D('',#48992,#39950,#39951) ;
#31876 = AXIS2_PLACEMENT_3D('',#48993,#39952,#39953) ;
#31877 = AXIS2_PLACEMENT_3D('',#48996,#39955,#39956) ;
#31878 = AXIS2_PLACEMENT_3D('',#48997,#39957,#39958) ;
#31879 = AXIS2_PLACEMENT_3D('',#48998,#39959,#39960) ;
#31880 = AXIS2_PLACEMENT_3D('',#49001,#39962,#39963) ;
#31881 = AXIS2_PLACEMENT_3D('',#49002,#39964,#39965) ;
#31882 = AXIS2_PLACEMENT_3D('',#49003,#39966,#39967) ;
#31883 = AXIS2_PLACEMENT_3D('',#49006,#39969,#39970) ;
#31884 = AXIS2_PLACEMENT_3D('',#49007,#39971,#39972) ;
#31885 = AXIS2_PLACEMENT_3D('',#49008,#39973,#39974) ;
#31886 = AXIS2_PLACEMENT_3D('',#49011,#39976,#39977) ;
#31887 = AXIS2_PLACEMENT_3D('',#49012,#39978,#39979) ;
#31888 = AXIS2_PLACEMENT_3D('',#49013,#39980,#39981) ;
#31889 = AXIS2_PLACEMENT_3D('',#49016,#39983,#39984) ;
#31890 = AXIS2_PLACEMENT_3D('',#49017,#39985,#39986) ;
#31891 = AXIS2_PLACEMENT_3D('',#49018,#39987,#39988) ;
#31892 = AXIS2_PLACEMENT_3D('',#49021,#39990,#39991) ;
#31893 = AXIS2_PLACEMENT_3D('',#49022,#39992,#39993) ;
#31894 = AXIS2_PLACEMENT_3D('',#49023,#39994,#39995) ;
#31895 = AXIS2_PLACEMENT_3D('',#49026,#39997,#39998) ;
#31896 = AXIS2_PLACEMENT_3D('',#49027,#39999,#40000) ;
#31897 = AXIS2_PLACEMENT_3D('',#49028,#40001,#40002) ;
#31898 = AXIS2_PLACEMENT_3D('',#49031,#40004,#40005) ;
#31899 = AXIS2_PLACEMENT_3D('',#49032,#40006,#40007) ;
#31900 = AXIS2_PLACEMENT_3D('',#49033,#40008,#40009) ;
#31901 = AXIS2_PLACEMENT_3D('',#49036,#40011,#40012) ;
#31902 = AXIS2_PLACEMENT_3D('',#49037,#40013,#40014) ;
#31903 = AXIS2_PLACEMENT_3D('',#49038,#40015,#40016) ;
#31904 = AXIS2_PLACEMENT_3D('',#49041,#40018,#40019) ;
#31905 = AXIS2_PLACEMENT_3D('',#49042,#40020,#40021) ;
#31906 = AXIS2_PLACEMENT_3D('',#49043,#40022,#40023) ;
#31907 = AXIS2_PLACEMENT_3D('',#49046,#40025,#40026) ;
#31908 = AXIS2_PLACEMENT_3D('',#49047,#40027,#40028) ;
#31909 = AXIS2_PLACEMENT_3D('',#49048,#40029,#40030) ;
#31910 = AXIS2_PLACEMENT_3D('',#49051,#40032,#40033) ;
#31911 = AXIS2_PLACEMENT_3D('',#49052,#40034,#40035) ;
#31912 = AXIS2_PLACEMENT_3D('',#49053,#40036,#40037) ;
#31913 = AXIS2_PLACEMENT_3D('',#49056,#40039,#40040) ;
#31914 = AXIS2_PLACEMENT_3D('',#49057,#40041,#40042) ;
#31915 = AXIS2_PLACEMENT_3D('',#49058,#40043,#40044) ;
#31916 = AXIS2_PLACEMENT_3D('',#49061,#40046,#40047) ;
#31917 = AXIS2_PLACEMENT_3D('',#49062,#40048,#40049) ;
#31918 = AXIS2_PLACEMENT_3D('',#49063,#40050,#40051) ;
#31919 = AXIS2_PLACEMENT_3D('',#49066,#40053,#40054) ;
#31920 = AXIS2_PLACEMENT_3D('',#49067,#40055,#40056) ;
#31921 = AXIS2_PLACEMENT_3D('',#49068,#40057,#40058) ;
#31922 = AXIS2_PLACEMENT_3D('',#49071,#40060,#40061) ;
#31923 = AXIS2_PLACEMENT_3D('',#49072,#40062,#40063) ;
#31924 = AXIS2_PLACEMENT_3D('',#49073,#40064,#40065) ;
#31925 = AXIS2_PLACEMENT_3D('',#49076,#40067,#40068) ;
#31926 = AXIS2_PLACEMENT_3D('',#49077,#40069,#40070) ;
#31927 = AXIS2_PLACEMENT_3D('',#49078,#40071,#40072) ;
#31928 = AXIS2_PLACEMENT_3D('',#49081,#40074,#40075) ;
#31929 = AXIS2_PLACEMENT_3D('',#49082,#40076,#40077) ;
#31930 = AXIS2_PLACEMENT_3D('',#49083,#40078,#40079) ;
#31931 = AXIS2_PLACEMENT_3D('',#49086,#40081,#40082) ;
#31932 = AXIS2_PLACEMENT_3D('',#49087,#40083,#40084) ;
#31933 = AXIS2_PLACEMENT_3D('',#49088,#40085,#40086) ;
#31934 = AXIS2_PLACEMENT_3D('',#49091,#40088,#40089) ;
#31935 = AXIS2_PLACEMENT_3D('',#49092,#40090,#40091) ;
#31936 = AXIS2_PLACEMENT_3D('',#49093,#40092,#40093) ;
#31937 = AXIS2_PLACEMENT_3D('',#49096,#40095,#40096) ;
#31938 = AXIS2_PLACEMENT_3D('',#49097,#40097,#40098) ;
#31939 = AXIS2_PLACEMENT_3D('',#49098,#40099,#40100) ;
#31940 = AXIS2_PLACEMENT_3D('',#49101,#40102,#40103) ;
#31941 = AXIS2_PLACEMENT_3D('',#49102,#40104,#40105) ;
#31942 = AXIS2_PLACEMENT_3D('',#49103,#40106,#40107) ;
#31943 = AXIS2_PLACEMENT_3D('',#49106,#40109,#40110) ;
#31944 = AXIS2_PLACEMENT_3D('',#49107,#40111,#40112) ;
#31945 = AXIS2_PLACEMENT_3D('',#49108,#40113,#40114) ;
#31946 = AXIS2_PLACEMENT_3D('',#49111,#40116,#40117) ;
#31947 = AXIS2_PLACEMENT_3D('',#49112,#40118,#40119) ;
#31948 = AXIS2_PLACEMENT_3D('',#49113,#40120,#40121) ;
#31949 = AXIS2_PLACEMENT_3D('',#49116,#40123,#40124) ;
#31950 = AXIS2_PLACEMENT_3D('',#49117,#40125,#40126) ;
#31951 = AXIS2_PLACEMENT_3D('',#49118,#40127,#40128) ;
#31952 = AXIS2_PLACEMENT_3D('',#49121,#40130,#40131) ;
#31953 = AXIS2_PLACEMENT_3D('',#49122,#40132,#40133) ;
#31954 = AXIS2_PLACEMENT_3D('',#49123,#40134,#40135) ;
#31955 = AXIS2_PLACEMENT_3D('',#49126,#40137,#40138) ;
#31956 = AXIS2_PLACEMENT_3D('',#49127,#40139,#40140) ;
#31957 = AXIS2_PLACEMENT_3D('',#49128,#40141,#40142) ;
#31958 = AXIS2_PLACEMENT_3D('',#49131,#40144,#40145) ;
#31959 = AXIS2_PLACEMENT_3D('',#49132,#40146,#40147) ;
#31960 = AXIS2_PLACEMENT_3D('',#49133,#40148,#40149) ;
#31961 = AXIS2_PLACEMENT_3D('',#49136,#40151,#40152) ;
#31962 = AXIS2_PLACEMENT_3D('',#49137,#40153,#40154) ;
#31963 = AXIS2_PLACEMENT_3D('',#49138,#40155,#40156) ;
#31964 = AXIS2_PLACEMENT_3D('',#49141,#40158,#40159) ;
#31965 = AXIS2_PLACEMENT_3D('',#49142,#40160,#40161) ;
#31966 = AXIS2_PLACEMENT_3D('',#49143,#40162,#40163) ;
#31967 = AXIS2_PLACEMENT_3D('',#49146,#40165,#40166) ;
#31968 = AXIS2_PLACEMENT_3D('',#49147,#40167,#40168) ;
#31969 = AXIS2_PLACEMENT_3D('',#49148,#40169,#40170) ;
#31970 = AXIS2_PLACEMENT_3D('',#49151,#40172,#40173) ;
#31971 = AXIS2_PLACEMENT_3D('',#49152,#40174,#40175) ;
#31972 = AXIS2_PLACEMENT_3D('',#49153,#40176,#40177) ;
#31973 = AXIS2_PLACEMENT_3D('',#49156,#40179,#40180) ;
#31974 = AXIS2_PLACEMENT_3D('',#49157,#40181,#40182) ;
#31975 = AXIS2_PLACEMENT_3D('',#49158,#40183,#40184) ;
#31976 = AXIS2_PLACEMENT_3D('',#49161,#40186,#40187) ;
#31977 = AXIS2_PLACEMENT_3D('',#49162,#40188,#40189) ;
#31978 = AXIS2_PLACEMENT_3D('',#49163,#40190,#40191) ;
#31979 = AXIS2_PLACEMENT_3D('',#49166,#40193,#40194) ;
#31980 = AXIS2_PLACEMENT_3D('',#49167,#40195,#40196) ;
#31981 = AXIS2_PLACEMENT_3D('',#49168,#40197,#40198) ;
#31982 = AXIS2_PLACEMENT_3D('',#49171,#40200,#40201) ;
#31983 = AXIS2_PLACEMENT_3D('',#49172,#40202,#40203) ;
#31984 = AXIS2_PLACEMENT_3D('',#49173,#40204,#40205) ;
#31985 = AXIS2_PLACEMENT_3D('',#49176,#40207,#40208) ;
#31986 = AXIS2_PLACEMENT_3D('',#49177,#40209,#40210) ;
#31987 = AXIS2_PLACEMENT_3D('',#49178,#40211,#40212) ;
#31988 = AXIS2_PLACEMENT_3D('',#49181,#40214,#40215) ;
#31989 = AXIS2_PLACEMENT_3D('',#49182,#40216,#40217) ;
#31990 = AXIS2_PLACEMENT_3D('',#49183,#40218,#40219) ;
#31991 = AXIS2_PLACEMENT_3D('',#49186,#40221,#40222) ;
#31992 = AXIS2_PLACEMENT_3D('',#49187,#40223,#40224) ;
#31993 = AXIS2_PLACEMENT_3D('',#49188,#40225,#40226) ;
#31994 = AXIS2_PLACEMENT_3D('',#49191,#40228,#40229) ;
#31995 = AXIS2_PLACEMENT_3D('',#49192,#40230,#40231) ;
#31996 = AXIS2_PLACEMENT_3D('',#49193,#40232,#40233) ;
#31997 = AXIS2_PLACEMENT_3D('',#49196,#40235,#40236) ;
#31998 = AXIS2_PLACEMENT_3D('',#49197,#40237,#40238) ;
#31999 = AXIS2_PLACEMENT_3D('',#49198,#40239,#40240) ;
#32000 = AXIS2_PLACEMENT_3D('',#49201,#40242,#40243) ;
#32001 = AXIS2_PLACEMENT_3D('',#49202,#40244,#40245) ;
#32002 = AXIS2_PLACEMENT_3D('',#49203,#40246,#40247) ;
#32003 = AXIS2_PLACEMENT_3D('',#49206,#40249,#40250) ;
#32004 = AXIS2_PLACEMENT_3D('',#49207,#40251,#40252) ;
#32005 = AXIS2_PLACEMENT_3D('',#49208,#40253,#40254) ;
#32006 = AXIS2_PLACEMENT_3D('',#49211,#40256,#40257) ;
#32007 = AXIS2_PLACEMENT_3D('',#49212,#40258,#40259) ;
#32008 = AXIS2_PLACEMENT_3D('',#49213,#40260,#40261) ;
#32009 = AXIS2_PLACEMENT_3D('',#49216,#40263,#40264) ;
#32010 = AXIS2_PLACEMENT_3D('',#49217,#40265,#40266) ;
#32011 = AXIS2_PLACEMENT_3D('',#49218,#40267,#40268) ;
#32012 = AXIS2_PLACEMENT_3D('',#49221,#40270,#40271) ;
#32013 = AXIS2_PLACEMENT_3D('',#49222,#40272,#40273) ;
#32014 = AXIS2_PLACEMENT_3D('',#49223,#40274,#40275) ;
#32015 = AXIS2_PLACEMENT_3D('',#49226,#40277,#40278) ;
#32016 = AXIS2_PLACEMENT_3D('',#49227,#40279,#40280) ;
#32017 = AXIS2_PLACEMENT_3D('',#49228,#40281,#40282) ;
#32018 = AXIS2_PLACEMENT_3D('',#49231,#40284,#40285) ;
#32019 = AXIS2_PLACEMENT_3D('',#49232,#40286,#40287) ;
#32020 = AXIS2_PLACEMENT_3D('',#49233,#40288,#40289) ;
#32021 = AXIS2_PLACEMENT_3D('',#49236,#40291,#40292) ;
#32022 = AXIS2_PLACEMENT_3D('',#49237,#40293,#40294) ;
#32023 = AXIS2_PLACEMENT_3D('',#49238,#40295,#40296) ;
#32024 = AXIS2_PLACEMENT_3D('',#49241,#40298,#40299) ;
#32025 = AXIS2_PLACEMENT_3D('',#49242,#40300,#40301) ;
#32026 = AXIS2_PLACEMENT_3D('',#49243,#40302,#40303) ;
#32027 = AXIS2_PLACEMENT_3D('',#49246,#40305,#40306) ;
#32028 = AXIS2_PLACEMENT_3D('',#49247,#40307,#40308) ;
#32029 = AXIS2_PLACEMENT_3D('',#49248,#40309,#40310) ;
#32030 = AXIS2_PLACEMENT_3D('',#49251,#40312,#40313) ;
#32031 = AXIS2_PLACEMENT_3D('',#49252,#40314,#40315) ;
#32032 = AXIS2_PLACEMENT_3D('',#49253,#40316,#40317) ;
#32033 = AXIS2_PLACEMENT_3D('',#49256,#40319,#40320) ;
#32034 = AXIS2_PLACEMENT_3D('',#49257,#40321,#40322) ;
#32035 = AXIS2_PLACEMENT_3D('',#49258,#40323,#40324) ;
#32036 = AXIS2_PLACEMENT_3D('',#49261,#40326,#40327) ;
#32037 = AXIS2_PLACEMENT_3D('',#49262,#40328,#40329) ;
#32038 = AXIS2_PLACEMENT_3D('',#49263,#40330,#40331) ;
#32039 = AXIS2_PLACEMENT_3D('',#49266,#40333,#40334) ;
#32040 = AXIS2_PLACEMENT_3D('',#49267,#40335,#40336) ;
#32041 = AXIS2_PLACEMENT_3D('',#49268,#40337,#40338) ;
#32042 = AXIS2_PLACEMENT_3D('',#49271,#40340,#40341) ;
#32043 = AXIS2_PLACEMENT_3D('',#49272,#40342,#40343) ;
#32044 = AXIS2_PLACEMENT_3D('',#49273,#40344,#40345) ;
#32045 = AXIS2_PLACEMENT_3D('',#49276,#40347,#40348) ;
#32046 = AXIS2_PLACEMENT_3D('',#49277,#40349,#40350) ;
#32047 = AXIS2_PLACEMENT_3D('',#49278,#40351,#40352) ;
#32048 = AXIS2_PLACEMENT_3D('',#49281,#40354,#40355) ;
#32049 = AXIS2_PLACEMENT_3D('',#49282,#40356,#40357) ;
#32050 = AXIS2_PLACEMENT_3D('',#49283,#40358,#40359) ;
#32051 = AXIS2_PLACEMENT_3D('',#49286,#40361,#40362) ;
#32052 = AXIS2_PLACEMENT_3D('',#49287,#40363,#40364) ;
#32053 = AXIS2_PLACEMENT_3D('',#49288,#40365,#40366) ;
#32054 = AXIS2_PLACEMENT_3D('',#49291,#40368,#40369) ;
#32055 = AXIS2_PLACEMENT_3D('',#49292,#40370,#40371) ;
#32056 = AXIS2_PLACEMENT_3D('',#49293,#40372,#40373) ;
#32057 = AXIS2_PLACEMENT_3D('',#49295,#40374,#40375) ;
#32058 = AXIS2_PLACEMENT_3D('',#49319,#40378,#40379) ;
#32059 = AXIS2_PLACEMENT_3D('',#49341,#40380,#40381) ;
#32060 = AXIS2_PLACEMENT_3D('',#49343,#40382,#40383) ;
#32061 = AXIS2_PLACEMENT_3D('',#49346,#40385,#40386) ;
#32062 = AXIS2_PLACEMENT_3D('',#49347,#40387,#40388) ;
#32063 = AXIS2_PLACEMENT_3D('',#49348,#40389,#40390) ;
#32064 = AXIS2_PLACEMENT_3D('',#49349,#40391,#40392) ;
#32065 = AXIS2_PLACEMENT_3D('',#49352,#40394,#40395) ;
#32066 = AXIS2_PLACEMENT_3D('',#49353,#40396,#40397) ;
#32067 = AXIS2_PLACEMENT_3D('',#49354,#40398,#40399) ;
#32068 = AXIS2_PLACEMENT_3D('',#49355,#40400,#40401) ;
#32069 = AXIS2_PLACEMENT_3D('',#49356,#40402,#40403) ;
#32070 = AXIS2_PLACEMENT_3D('',#49357,#40404,#40405) ;
#32071 = AXIS2_PLACEMENT_3D('',#49358,#40406,#40407) ;
#32072 = AXIS2_PLACEMENT_3D('',#49359,#40408,#40409) ;
#32073 = AXIS2_PLACEMENT_3D('',#49360,#40410,#40411) ;
#32074 = AXIS2_PLACEMENT_3D('',#49361,#40412,#40413) ;
#32075 = AXIS2_PLACEMENT_3D('',#49362,#40414,#40415) ;
#32076 = AXIS2_PLACEMENT_3D('',#49363,#40416,#40417) ;
#32077 = AXIS2_PLACEMENT_3D('',#49364,#40418,#40419) ;
#32078 = AXIS2_PLACEMENT_3D('',#49365,#40420,#40421) ;
#32079 = AXIS2_PLACEMENT_3D('',#49366,#40422,#40423) ;
#32080 = AXIS2_PLACEMENT_3D('',#49367,#40424,#40425) ;
#32081 = AXIS2_PLACEMENT_3D('',#49368,#40426,#40427) ;
#32082 = AXIS2_PLACEMENT_3D('',#49369,#40428,#40429) ;
#32083 = AXIS2_PLACEMENT_3D('',#49370,#40430,#40431) ;
#32084 = AXIS2_PLACEMENT_3D('',#49373,#40432,#40433) ;
#32085 = AXIS2_PLACEMENT_3D('',#49374,#40434,#40435) ;
#32086 = AXIS2_PLACEMENT_3D('',#49377,#40436,#40437) ;
#32087 = AXIS2_PLACEMENT_3D('',#49378,#40438,#40439) ;
#32088 = AXIS2_PLACEMENT_3D('',#49379,#40440,#40441) ;
#32089 = AXIS2_PLACEMENT_3D('',#49380,#40442,#40443) ;
#32090 = AXIS2_PLACEMENT_3D('',#49381,#40444,#40445) ;
#32091 = AXIS2_PLACEMENT_3D('',#49382,#40446,#40447) ;
#32092 = AXIS2_PLACEMENT_3D('',#49384,#40448,#40449) ;
#32093 = AXIS2_PLACEMENT_3D('',#49386,#40450,#40451) ;
#32094 = AXIS2_PLACEMENT_3D('',#49387,#40452,#40453) ;
#32095 = AXIS2_PLACEMENT_3D('',#49428,#40454,#40455) ;
#32096 = AXIS2_PLACEMENT_3D('',#49429,#40456,#40457) ;
#32097 = AXIS2_PLACEMENT_3D('',#49432,#40458,#40459) ;
#32098 = AXIS2_PLACEMENT_3D('',#49434,#40460,#40461) ;
#32099 = AXIS2_PLACEMENT_3D('',#49436,#40463,#40464) ;
#32100 = AXIS2_PLACEMENT_3D('',#49437,#40465,#40466) ;
#32101 = AXIS2_PLACEMENT_3D('',#49439,#40467,#40468) ;
#32102 = AXIS2_PLACEMENT_3D('',#49441,#40469,#40470) ;
#32103 = AXIS2_PLACEMENT_3D('',#49442,#40471,#40472) ;
#32104 = AXIS2_PLACEMENT_3D('',#49483,#40473,#40474) ;
#32105 = AXIS2_PLACEMENT_3D('',#49484,#40475,#40476) ;
#32106 = AXIS2_PLACEMENT_3D('',#49487,#40478,#40479) ;
#32107 = AXIS2_PLACEMENT_3D('',#49488,#40480,#40481) ;
#32108 = AXIS2_PLACEMENT_3D('',#49489,#40482,#40483) ;
#32109 = AXIS2_PLACEMENT_3D('',#49491,#40484,#40485) ;
#32110 = AXIS2_PLACEMENT_3D('',#49493,#40487,#40488) ;
#32111 = AXIS2_PLACEMENT_3D('',#49494,#40489,#40490) ;
#32112 = AXIS2_PLACEMENT_3D('',#49497,#40492,#40493) ;
#32113 = AXIS2_PLACEMENT_3D('',#49498,#40494,#40495) ;
#32114 = AXIS2_PLACEMENT_3D('',#49499,#40496,#40497) ;
#32115 = AXIS2_PLACEMENT_3D('',#49500,#40498,#40499) ;
#32116 = AXIS2_PLACEMENT_3D('',#49501,#40500,#40501) ;
#32117 = AXIS2_PLACEMENT_3D('',#49503,#40502,#40503) ;
#32118 = AXIS2_PLACEMENT_3D('',#49504,#40504,#40505) ;
#32119 = AXIS2_PLACEMENT_3D('',#49505,#40506,#40507) ;
#32120 = AXIS2_PLACEMENT_3D('',#49507,#40508,#40509) ;
#32121 = AXIS2_PLACEMENT_3D('',#49510,#40511,#40512) ;
#32122 = AXIS2_PLACEMENT_3D('',#49511,#40513,#40514) ;
#32123 = AXIS2_PLACEMENT_3D('',#49512,#40515,#40516) ;
#32124 = AXIS2_PLACEMENT_3D('',#49521,#40521,#40522) ;
#32125 = AXIS2_PLACEMENT_3D('',#49529,#40527,#40528) ;
#32126 = AXIS2_PLACEMENT_3D('',#49537,#40533,#40534) ;
#32127 = AXIS2_PLACEMENT_3D('',#49540,#40537,#40538) ;
#32128 = AXIS2_PLACEMENT_3D('',#49541,#40539,#40540) ;
#32129 = AXIS2_PLACEMENT_3D('',#49543,#40542,#40543) ;
#32130 = AXIS2_PLACEMENT_3D('',#49544,#40544,#40545) ;
#32131 = AXIS2_PLACEMENT_3D('',#49546,#40546,#40547) ;
#32132 = AXIS2_PLACEMENT_3D('',#49547,#40548,#40549) ;
#32133 = AXIS2_PLACEMENT_3D('',#49551,#40551,#40552) ;
#32134 = AXIS2_PLACEMENT_3D('',#49552,#40553,#40554) ;
#32135 = AXIS2_PLACEMENT_3D('',#49576,#40557,#40558) ;
#32136 = AXIS2_PLACEMENT_3D('',#49634,#40559,#40560) ;
#32137 = AXIS2_PLACEMENT_3D('',#49635,#40561,#40562) ;
#32138 = AXIS2_PLACEMENT_3D('',#49637,#40564,#40565) ;
#32139 = AXIS2_PLACEMENT_3D('',#49717,#40567,#40568) ;
#32140 = AXIS2_PLACEMENT_3D('',#49721,#40570,#40571) ;
#32141 = AXIS2_PLACEMENT_3D('',#49722,#40572,#40573) ;
#32142 = AXIS2_PLACEMENT_3D('',#49723,#40574,#40575) ;
#32143 = AXIS2_PLACEMENT_3D('',#49727,#40578,#40579) ;
#32144 = AXIS2_PLACEMENT_3D('',#49728,#40580,#40581) ;
#32145 = AXIS2_PLACEMENT_3D('',#49729,#40582,#40583) ;
#32146 = AXIS2_PLACEMENT_3D('',#49730,#40584,#40585) ;
#32147 = AXIS2_PLACEMENT_3D('',#49739,#40589,#40590) ;
#32148 = AXIS2_PLACEMENT_3D('',#49746,#40594,#40595) ;
#32149 = AXIS2_PLACEMENT_3D('',#49750,#40597,#40598) ;
#32150 = AXIS2_PLACEMENT_3D('',#49751,#40599,#40600) ;
#32151 = AXIS2_PLACEMENT_3D('',#49753,#40601,#40602) ;
#32152 = AXIS2_PLACEMENT_3D('',#49754,#40603,#40604) ;
#32153 = AXIS2_PLACEMENT_3D('',#49755,#40605,#40606) ;
#32154 = AXIS2_PLACEMENT_3D('',#49757,#40607,#40608) ;
#32155 = AXIS2_PLACEMENT_3D('',#49758,#40609,#40610) ;
#32156 = AXIS2_PLACEMENT_3D('',#49759,#40611,#40612) ;
#32157 = AXIS2_PLACEMENT_3D('',#49761,#40614,#40615) ;
#32158 = AXIS2_PLACEMENT_3D('',#49762,#40616,#40617) ;
#32159 = AXIS2_PLACEMENT_3D('',#49764,#40618,#40619) ;
#32160 = AXIS2_PLACEMENT_3D('',#49767,#40621,#40622) ;
#32161 = AXIS2_PLACEMENT_3D('',#49768,#40623,#40624) ;
#32162 = AXIS2_PLACEMENT_3D('',#49770,#40625,#40626) ;
#32163 = AXIS2_PLACEMENT_3D('',#49773,#40628,#40629) ;
#32164 = AXIS2_PLACEMENT_3D('',#49774,#40630,#40631) ;
#32165 = AXIS2_PLACEMENT_3D('',#49775,#40632,#40633) ;
#32166 = AXIS2_PLACEMENT_3D('',#49776,#40634,#40635) ;
#32167 = AXIS2_PLACEMENT_3D('',#49777,#40636,#40637) ;
#32168 = AXIS2_PLACEMENT_3D('',#49782,#40639,#40640) ;
#32169 = AXIS2_PLACEMENT_3D('',#49785,#40642,#40643) ;
#32170 = AXIS2_PLACEMENT_3D('',#49786,#40644,#40645) ;
#32171 = AXIS2_PLACEMENT_3D('',#49796,#40651,#40652) ;
#32172 = AXIS2_PLACEMENT_3D('',#49800,#40655,#40656) ;
#32173 = AXIS2_PLACEMENT_3D('',#49804,#40659,#40660) ;
#32174 = AXIS2_PLACEMENT_3D('',#49810,#40664,#40665) ;
#32175 = AXIS2_PLACEMENT_3D('',#49812,#40667,#40668) ;
#32176 = AXIS2_PLACEMENT_3D('',#49814,#40670,#40671) ;
#32177 = AXIS2_PLACEMENT_3D('',#49815,#40672,#40673) ;
#32178 = AXIS2_PLACEMENT_3D('',#49824,#40678,#40679) ;
#32179 = AXIS2_PLACEMENT_3D('',#49833,#40684,#40685) ;
#32180 = AXIS2_PLACEMENT_3D('',#49836,#40688,#40689) ;
#32181 = AXIS2_PLACEMENT_3D('',#49838,#40691,#40692) ;
#32182 = AXIS2_PLACEMENT_3D('',#49840,#40694,#40695) ;
#32183 = AXIS2_PLACEMENT_3D('',#49841,#40696,#40697) ;
#32184 = AXIS2_PLACEMENT_3D('',#49842,#40698,#40699) ;
#32185 = AXIS2_PLACEMENT_3D('',#49855,#40706,#40707) ;
#32186 = AXIS2_PLACEMENT_3D('',#49857,#40708,#40709) ;
#32187 = AXIS2_PLACEMENT_3D('',#49861,#40712,#40713) ;
#32188 = AXIS2_PLACEMENT_3D('',#49865,#40716,#40717) ;
#32189 = AXIS2_PLACEMENT_3D('',#49871,#40721,#40722) ;
#32190 = AXIS2_PLACEMENT_3D('',#49873,#40724,#40725) ;
#32191 = AXIS2_PLACEMENT_3D('',#49877,#40728,#40729) ;
#32192 = AXIS2_PLACEMENT_3D('',#49879,#40730,#40731) ;
#32193 = AXIS2_PLACEMENT_3D('',#49880,#40732,#40733) ;
#32194 = AXIS2_PLACEMENT_3D('',#49882,#40734,#40735) ;
#32195 = AXIS2_PLACEMENT_3D('',#49883,#40736,#40737) ;
#32196 = AXIS2_PLACEMENT_3D('',#49886,#40739,#40740) ;
#32197 = AXIS2_PLACEMENT_3D('',#49887,#40741,#40742) ;
#32198 = AXIS2_PLACEMENT_3D('',#49889,#40743,#40744) ;
#32199 = AXIS2_PLACEMENT_3D('',#49891,#40746,#40747) ;
#32200 = AXIS2_PLACEMENT_3D('',#49892,#40748,#40749) ;
#32201 = AXIS2_PLACEMENT_3D('',#49893,#40750,#40751) ;
#32202 = AXIS2_PLACEMENT_3D('',#49894,#40752,#40753) ;
#32203 = AXIS2_PLACEMENT_3D('',#49895,#40754,#40755) ;
#32204 = AXIS2_PLACEMENT_3D('',#49896,#40756,#40757) ;
#32205 = AXIS2_PLACEMENT_3D('',#49897,#40758,#40759) ;
#32206 = AXIS2_PLACEMENT_3D('',#49898,#40760,#40761) ;
#32207 = AXIS2_PLACEMENT_3D('',#49899,#40762,#40763) ;
#32208 = AXIS2_PLACEMENT_3D('',#49900,#40764,#40765) ;
#32209 = AXIS2_PLACEMENT_3D('',#49902,#40766,#40767) ;
#32210 = AXIS2_PLACEMENT_3D('',#49905,#40769,#40770) ;
#32211 = AXIS2_PLACEMENT_3D('',#49906,#40771,#40772) ;
#32212 = AXIS2_PLACEMENT_3D('',#49907,#40773,#40774) ;
#32213 = AXIS2_PLACEMENT_3D('',#49916,#40779,#40780) ;
#32214 = AXIS2_PLACEMENT_3D('',#49925,#40785,#40786) ;
#32215 = AXIS2_PLACEMENT_3D('',#49932,#40791,#40792) ;
#32216 = AXIS2_PLACEMENT_3D('',#49936,#40795,#40796) ;
#32217 = AXIS2_PLACEMENT_3D('',#49940,#40799,#40800) ;
#32218 = AXIS2_PLACEMENT_3D('',#49942,#40802,#40803) ;
#32219 = AXIS2_PLACEMENT_3D('',#49944,#40805,#40806) ;
#32220 = AXIS2_PLACEMENT_3D('',#49945,#40807,#40808) ;
#32221 = AXIS2_PLACEMENT_3D('',#49946,#40809,#40810) ;
#32222 = AXIS2_PLACEMENT_3D('',#49948,#40811,#40812) ;
#32223 = AXIS2_PLACEMENT_3D('',#49951,#40814,#40815) ;
#32224 = AXIS2_PLACEMENT_3D('',#49952,#40816,#40817) ;
#32225 = AXIS2_PLACEMENT_3D('',#49961,#40822,#40823) ;
#32226 = AXIS2_PLACEMENT_3D('',#49970,#40828,#40829) ;
#32227 = AXIS2_PLACEMENT_3D('',#49977,#40834,#40835) ;
#32228 = AXIS2_PLACEMENT_3D('',#49981,#40838,#40839) ;
#32229 = AXIS2_PLACEMENT_3D('',#49985,#40842,#40843) ;
#32230 = AXIS2_PLACEMENT_3D('',#49987,#40845,#40846) ;
#32231 = AXIS2_PLACEMENT_3D('',#49989,#40848,#40849) ;
#32232 = AXIS2_PLACEMENT_3D('',#49990,#40850,#40851) ;
#32233 = AXIS2_PLACEMENT_3D('',#49991,#40852,#40853) ;
#32234 = AXIS2_PLACEMENT_3D('',#49993,#40854,#40855) ;
#32235 = AXIS2_PLACEMENT_3D('',#49996,#40857,#40858) ;
#32236 = AXIS2_PLACEMENT_3D('',#49997,#40859,#40860) ;
#32237 = AXIS2_PLACEMENT_3D('',#49998,#40861,#40862) ;
#32238 = AXIS2_PLACEMENT_3D('',#50007,#40867,#40868) ;
#32239 = AXIS2_PLACEMENT_3D('',#50016,#40873,#40874) ;
#32240 = AXIS2_PLACEMENT_3D('',#50023,#40879,#40880) ;
#32241 = AXIS2_PLACEMENT_3D('',#50027,#40883,#40884) ;
#32242 = AXIS2_PLACEMENT_3D('',#50031,#40887,#40888) ;
#32243 = AXIS2_PLACEMENT_3D('',#50033,#40890,#40891) ;
#32244 = AXIS2_PLACEMENT_3D('',#50035,#40893,#40894) ;
#32245 = AXIS2_PLACEMENT_3D('',#50036,#40895,#40896) ;
#32246 = AXIS2_PLACEMENT_3D('',#50037,#40897,#40898) ;
#32247 = AXIS2_PLACEMENT_3D('',#50039,#40899,#40900) ;
#32248 = AXIS2_PLACEMENT_3D('',#50042,#40902,#40903) ;
#32249 = AXIS2_PLACEMENT_3D('',#50043,#40904,#40905) ;
#32250 = AXIS2_PLACEMENT_3D('',#50052,#40910,#40911) ;
#32251 = AXIS2_PLACEMENT_3D('',#50061,#40916,#40917) ;
#32252 = AXIS2_PLACEMENT_3D('',#50068,#40922,#40923) ;
#32253 = AXIS2_PLACEMENT_3D('',#50072,#40926,#40927) ;
#32254 = AXIS2_PLACEMENT_3D('',#50076,#40930,#40931) ;
#32255 = AXIS2_PLACEMENT_3D('',#50078,#40933,#40934) ;
#32256 = AXIS2_PLACEMENT_3D('',#50080,#40936,#40937) ;
#32257 = AXIS2_PLACEMENT_3D('',#50081,#40938,#40939) ;
#32258 = AXIS2_PLACEMENT_3D('',#50082,#40940,#40941) ;
#32259 = AXIS2_PLACEMENT_3D('',#50084,#40942,#40943) ;
#32260 = AXIS2_PLACEMENT_3D('',#50086,#40944,#40945) ;
#32261 = AXIS2_PLACEMENT_3D('',#50087,#40946,#40947) ;
#32262 = AXIS2_PLACEMENT_3D('',#50089,#40948,#40949) ;
#32263 = AXIS2_PLACEMENT_3D('',#50091,#40951,#40952) ;
#32264 = AXIS2_PLACEMENT_3D('',#50092,#40953,#40954) ;
#32265 = AXIS2_PLACEMENT_3D('',#50095,#40956,#40957) ;
#32266 = AXIS2_PLACEMENT_3D('',#50096,#40958,#40959) ;
#32267 = AXIS2_PLACEMENT_3D('',#50097,#40960,#40961) ;
#32268 = AXIS2_PLACEMENT_3D('',#50098,#40962,#40963) ;
#32269 = AXIS2_PLACEMENT_3D('',#50100,#40964,#40965) ;
#32270 = AXIS2_PLACEMENT_3D('',#50102,#40966,#40967) ;
#32271 = AXIS2_PLACEMENT_3D('',#50103,#40968,#40969) ;
#32272 = AXIS2_PLACEMENT_3D('',#50105,#40970,#40971) ;
#32273 = AXIS2_PLACEMENT_3D('',#50107,#40973,#40974) ;
#32274 = AXIS2_PLACEMENT_3D('',#50108,#40975,#40976) ;
#32275 = AXIS2_PLACEMENT_3D('',#50111,#40978,#40979) ;
#32276 = AXIS2_PLACEMENT_3D('',#50112,#40980,#40981) ;
#32277 = AXIS2_PLACEMENT_3D('',#50113,#40982,#40983) ;
#32278 = AXIS2_PLACEMENT_3D('',#50114,#40984,#40985) ;
#32279 = AXIS2_PLACEMENT_3D('',#50117,#40986,#40987) ;
#32280 = AXIS2_PLACEMENT_3D('',#50142,#40988,#40989) ;
#32281 = AXIS2_PLACEMENT_3D('',#50144,#40990,#40991) ;
#32282 = AXIS2_PLACEMENT_3D('',#50148,#40993,#40994) ;
#32283 = AXIS2_PLACEMENT_3D('',#50150,#40995,#40996) ;
#32284 = AXIS2_PLACEMENT_3D('',#50151,#40997,#40998) ;
#32285 = AXIS2_PLACEMENT_3D('',#50152,#40999,#41000) ;
#32286 = AXIS2_PLACEMENT_3D('',#50153,#41001,#41002) ;
#32287 = AXIS2_PLACEMENT_3D('',#50156,#41003,#41004) ;
#32288 = AXIS2_PLACEMENT_3D('',#50157,#41005,#41006) ;
#32289 = AXIS2_PLACEMENT_3D('',#50158,#41007,#41008) ;
#32290 = AXIS2_PLACEMENT_3D('',#50161,#41009,#41010) ;
#32291 = AXIS2_PLACEMENT_3D('',#50162,#41011,#41012) ;
#32292 = AXIS2_PLACEMENT_3D('',#50163,#41013,#41014) ;
#32293 = AXIS2_PLACEMENT_3D('',#50166,#41015,#41016) ;
#32294 = AXIS2_PLACEMENT_3D('',#50167,#41017,#41018) ;
#32295 = AXIS2_PLACEMENT_3D('',#50168,#41019,#41020) ;
#32296 = AXIS2_PLACEMENT_3D('',#50171,#41021,#41022) ;
#32297 = AXIS2_PLACEMENT_3D('',#50173,#41023,#41024) ;
#32298 = AXIS2_PLACEMENT_3D('',#50175,#41025,#41026) ;
#32299 = AXIS2_PLACEMENT_3D('',#50176,#41027,#41028) ;
#32300 = AXIS2_PLACEMENT_3D('',#50177,#41029,#41030) ;
#32301 = AXIS2_PLACEMENT_3D('',#50180,#41031,#41032) ;
#32302 = AXIS2_PLACEMENT_3D('',#50182,#41033,#41034) ;
#32303 = AXIS2_PLACEMENT_3D('',#50184,#41035,#41036) ;
#32304 = AXIS2_PLACEMENT_3D('',#50185,#41037,#41038) ;
#32305 = AXIS2_PLACEMENT_3D('',#50186,#41039,#41040) ;
#32306 = AXIS2_PLACEMENT_3D('',#50189,#41041,#41042) ;
#32307 = AXIS2_PLACEMENT_3D('',#50191,#41043,#41044) ;
#32308 = AXIS2_PLACEMENT_3D('',#50193,#41045,#41046) ;
#32309 = AXIS2_PLACEMENT_3D('',#50194,#41047,#41048) ;
#32310 = AXIS2_PLACEMENT_3D('',#50195,#41049,#41050) ;
#32311 = AXIS2_PLACEMENT_3D('',#50198,#41051,#41052) ;
#32312 = AXIS2_PLACEMENT_3D('',#50200,#41053,#41054) ;
#32313 = AXIS2_PLACEMENT_3D('',#50202,#41055,#41056) ;
#32314 = AXIS2_PLACEMENT_3D('',#50203,#41057,#41058) ;
#32315 = AXIS2_PLACEMENT_3D('',#50204,#41059,#41060) ;
#32316 = AXIS2_PLACEMENT_3D('',#50207,#41061,#41062) ;
#32317 = AXIS2_PLACEMENT_3D('',#50209,#41063,#41064) ;
#32318 = AXIS2_PLACEMENT_3D('',#50211,#41065,#41066) ;
#32319 = AXIS2_PLACEMENT_3D('',#50212,#41067,#41068) ;
#32320 = AXIS2_PLACEMENT_3D('',#50213,#41069,#41070) ;
#32321 = AXIS2_PLACEMENT_3D('',#50216,#41071,#41072) ;
#32322 = AXIS2_PLACEMENT_3D('',#50218,#41073,#41074) ;
#32323 = AXIS2_PLACEMENT_3D('',#50220,#41075,#41076) ;
#32324 = AXIS2_PLACEMENT_3D('',#50221,#41077,#41078) ;
#32325 = AXIS2_PLACEMENT_3D('',#50222,#41079,#41080) ;
#32326 = AXIS2_PLACEMENT_3D('',#50223,#41081,#41082) ;
#32327 = AXIS2_PLACEMENT_3D('',#50224,#41083,#41084) ;
#32328 = AXIS2_PLACEMENT_3D('',#50227,#41085,#41086) ;
#32329 = AXIS2_PLACEMENT_3D('',#50228,#41087,#41088) ;
#32330 = AXIS2_PLACEMENT_3D('',#50229,#41089,#41090) ;
#32331 = AXIS2_PLACEMENT_3D('',#50231,#41091,#41092) ;
#32332 = AXIS2_PLACEMENT_3D('',#50232,#41093,#41094) ;
#32333 = AXIS2_PLACEMENT_3D('',#50235,#41096,#41097) ;
#32334 = AXIS2_PLACEMENT_3D('',#50236,#41098,#41099) ;
#32335 = AXIS2_PLACEMENT_3D('',#50237,#41100,#41101) ;
#32336 = AXIS2_PLACEMENT_3D('',#50240,#41103,#41104) ;
#32337 = AXIS2_PLACEMENT_3D('',#50241,#41105,#41106) ;
#32338 = AXIS2_PLACEMENT_3D('',#50242,#41107,#41108) ;
#32339 = AXIS2_PLACEMENT_3D('',#50245,#41110,#41111) ;
#32340 = AXIS2_PLACEMENT_3D('',#50246,#41112,#41113) ;
#32341 = AXIS2_PLACEMENT_3D('',#50247,#41114,#41115) ;
#32342 = AXIS2_PLACEMENT_3D('',#50249,#41117,#41118) ;
#32343 = AXIS2_PLACEMENT_3D('',#50250,#41119,#41120) ;
#32344 = AXIS2_PLACEMENT_3D('',#50252,#41122,#41123) ;
#32345 = AXIS2_PLACEMENT_3D('',#50253,#41124,#41125) ;
#32346 = AXIS2_PLACEMENT_3D('',#50255,#41127,#41128) ;
#32347 = AXIS2_PLACEMENT_3D('',#50256,#41129,#41130) ;
#32348 = AXIS2_PLACEMENT_3D('',#50258,#41132,#41133) ;
#32349 = AXIS2_PLACEMENT_3D('',#50259,#41134,#41135) ;
#32350 = AXIS2_PLACEMENT_3D('',#50261,#41137,#41138) ;
#32351 = AXIS2_PLACEMENT_3D('',#50262,#41139,#41140) ;
#32352 = AXIS2_PLACEMENT_3D('',#50278,#41142,#41143) ;
#32353 = AXIS2_PLACEMENT_3D('',#50280,#41144,#41145) ;
#32354 = AXIS2_PLACEMENT_3D('',#50293,#41146,#41147) ;
#32355 = AXIS2_PLACEMENT_3D('',#50296,#41149,#41150) ;
#32356 = AXIS2_PLACEMENT_3D('',#50297,#41151,#41152) ;
#32357 = AXIS2_PLACEMENT_3D('',#50298,#41153,#41154) ;
#32358 = AXIS2_PLACEMENT_3D('',#50300,#41156,#41157) ;
#32359 = AXIS2_PLACEMENT_3D('',#50301,#41158,#41159) ;
#32360 = AXIS2_PLACEMENT_3D('',#50302,#41160,#41161) ;
#32361 = AXIS2_PLACEMENT_3D('',#50305,#41163,#41164) ;
#32362 = AXIS2_PLACEMENT_3D('',#50306,#41165,#41166) ;
#32363 = AXIS2_PLACEMENT_3D('',#50307,#41167,#41168) ;
#32364 = AXIS2_PLACEMENT_3D('',#50308,#41169,#41170) ;
#32365 = AXIS2_PLACEMENT_3D('',#50309,#41171,#41172) ;
#32366 = AXIS2_PLACEMENT_3D('',#50310,#41173,#41174) ;
#32367 = AXIS2_PLACEMENT_3D('',#50311,#41175,#41176) ;
#32368 = AXIS2_PLACEMENT_3D('',#50312,#41177,#41178) ;
#32369 = AXIS2_PLACEMENT_3D('',#50313,#41179,#41180) ;
#32370 = AXIS2_PLACEMENT_3D('',#50314,#41181,#41182) ;
#32371 = AXIS2_PLACEMENT_3D('',#50315,#41183,#41184) ;
#32372 = AXIS2_PLACEMENT_3D('',#50316,#41185,#41186) ;
#32373 = AXIS2_PLACEMENT_3D('',#50317,#41187,#41188) ;
#32374 = AXIS2_PLACEMENT_3D('',#50318,#41189,#41190) ;
#32375 = AXIS2_PLACEMENT_3D('',#50319,#41191,#41192) ;
#32376 = AXIS2_PLACEMENT_3D('',#50320,#41193,#41194) ;
#32377 = AXIS2_PLACEMENT_3D('',#50321,#41195,#41196) ;
#32378 = AXIS2_PLACEMENT_3D('',#50322,#41197,#41198) ;
#32379 = AXIS2_PLACEMENT_3D('',#50323,#41199,#41200) ;
#32380 = AXIS2_PLACEMENT_3D('',#50324,#41201,#41202) ;
#32381 = AXIS2_PLACEMENT_3D('',#50325,#41203,#41204) ;
#32382 = AXIS2_PLACEMENT_3D('',#50326,#41205,#41206) ;
#32383 = AXIS2_PLACEMENT_3D('',#50327,#41207,#41208) ;
#32384 = AXIS2_PLACEMENT_3D('',#50328,#41209,#41210) ;
#32385 = AXIS2_PLACEMENT_3D('',#50329,#41211,#41212) ;
#32386 = AXIS2_PLACEMENT_3D('',#50330,#41213,#41214) ;
#32387 = AXIS2_PLACEMENT_3D('',#50331,#41215,#41216) ;
#32388 = AXIS2_PLACEMENT_3D('',#50332,#41217,#41218) ;
#32389 = AXIS2_PLACEMENT_3D('',#50333,#41219,#41220) ;
#32390 = AXIS2_PLACEMENT_3D('',#50334,#41221,#41222) ;
#32391 = DIRECTION('axis',(0.,0.,1.)) ;
#32392 = DIRECTION('refdir',(1.,0.,0.)) ;
#32393 = DIRECTION('axis',(0.,0.,1.)) ;
#32394 = DIRECTION('refdir',(1.,0.,0.)) ;
#32395 = DIRECTION('axis',(0.,0.,1.)) ;
#32396 = DIRECTION('refdir',(1.,0.,0.)) ;
#32397 = DIRECTION('center_axis',(-1.,0.,0.)) ;
#32398 = DIRECTION('ref_axis',(0.,0.,1.)) ;
#32399 = DIRECTION('center_axis',(-1.,0.,0.)) ;
#32400 = DIRECTION('ref_axis',(0.,0.,1.)) ;
#32401 = DIRECTION('',(-1.,0.,0.)) ;
#32402 = DIRECTION('center_axis',(1.,0.,0.)) ;
#32403 = DIRECTION('ref_axis',(0.,0.,1.)) ;
#32404 = DIRECTION('center_axis',(-1.,0.,0.)) ;
#32405 = DIRECTION('ref_axis',(0.,0.,1.)) ;
#32406 = DIRECTION('',(0.,0.,1.)) ;
#32407 = DIRECTION('',(0.,1.,0.)) ;
#32408 = DIRECTION('',(0.,0.,-1.)) ;
#32409 = DIRECTION('',(0.,-1.,0.)) ;
#32410 = DIRECTION('',(0.,0.,-1.)) ;
#32411 = DIRECTION('',(0.,1.,0.)) ;
#32412 = DIRECTION('',(0.,0.,-1.)) ;
#32413 = DIRECTION('',(0.,1.,0.)) ;
#32414 = DIRECTION('center_axis',(0.,1.,0.)) ;
#32415 = DIRECTION('ref_axis',(0.,0.,1.)) ;
#32416 = DIRECTION('',(1.,0.,0.)) ;
#32417 = DIRECTION('',(0.,0.,-1.)) ;
#32418 = DIRECTION('',(-1.,0.,0.)) ;
#32419 = DIRECTION('center_axis',(0.,0.,1.)) ;
#32420 = DIRECTION('ref_axis',(1.,0.,0.)) ;
#32421 = DIRECTION('',(-1.,0.,0.)) ;
#32422 = DIRECTION('',(0.,-1.,0.)) ;
#32423 = DIRECTION('',(1.,0.,0.)) ;
#32424 = DIRECTION('center_axis',(0.,1.,0.)) ;
#32425 = DIRECTION('ref_axis',(0.,0.,1.)) ;
#32426 = DIRECTION('',(0.,0.,-1.)) ;
#32427 = DIRECTION('',(-1.,0.,0.)) ;
#32428 = DIRECTION('center_axis',(0.,0.,1.)) ;
#32429 = DIRECTION('ref_axis',(1.,0.,0.)) ;
#32430 = DIRECTION('center_axis',(0.,0.,1.)) ;
#32431 = DIRECTION('ref_axis',(1.,0.,0.)) ;
#32432 = DIRECTION('',(0.,-1.,0.)) ;
#32433 = DIRECTION('center_axis',(0.,0.,1.)) ;
#32434 = DIRECTION('ref_axis',(1.,0.,0.)) ;
#32435 = DIRECTION('',(0.,1.,0.)) ;
#32436 = DIRECTION('',(1.,0.,0.)) ;
#32437 = DIRECTION('center_axis',(1.,0.,0.)) ;
#32438 = DIRECTION('ref_axis',(0.,0.,-1.)) ;
#32439 = DIRECTION('',(0.,0.,-1.)) ;
#32440 = DIRECTION('',(0.,0.,-1.)) ;
#32441 = DIRECTION('',(0.,-1.,0.)) ;
#32442 = DIRECTION('center_axis',(0.,-1.,0.)) ;
#32443 = DIRECTION('ref_axis',(0.,0.,-1.)) ;
#32444 = DIRECTION('center_axis',(0.,0.,1.)) ;
#32445 = DIRECTION('ref_axis',(1.,0.,0.)) ;
#32446 = DIRECTION('center_axis',(0.,0.,1.)) ;
#32447 = DIRECTION('ref_axis',(1.,0.,0.)) ;
#32448 = DIRECTION('',(0.,0.,-1.)) ;
#32449 = DIRECTION('center_axis',(0.,0.,-1.)) ;
#32450 = DIRECTION('ref_axis',(1.,0.,0.)) ;
#32451 = DIRECTION('',(0.,0.,1.)) ;
#32452 = DIRECTION('center_axis',(0.,0.,1.)) ;
#32453 = DIRECTION('ref_axis',(1.,0.,0.)) ;
#32454 = DIRECTION('',(0.,0.,-1.)) ;
#32455 = DIRECTION('center_axis',(0.,0.,-1.)) ;
#32456 = DIRECTION('ref_axis',(1.,0.,0.)) ;
#32457 = DIRECTION('center_axis',(0.,0.,-1.)) ;
#32458 = DIRECTION('ref_axis',(1.,0.,0.)) ;
#32459 = DIRECTION('center_axis',(1.,0.,0.)) ;
#32460 = DIRECTION('ref_axis',(0.,0.,-1.)) ;
#32461 = DIRECTION('center_axis',(1.,0.,0.)) ;
#32462 = DIRECTION('ref_axis',(0.,0.,-1.)) ;
#32463 = DIRECTION('',(1.,0.,0.)) ;
#32464 = DIRECTION('center_axis',(-1.,0.,0.)) ;
#32465 = DIRECTION('ref_axis',(0.,0.,-1.)) ;
#32466 = DIRECTION('center_axis',(-1.,0.,0.)) ;
#32467 = DIRECTION('ref_axis',(0.,0.,1.)) ;
#32468 = DIRECTION('',(0.,1.,0.)) ;
#32469 = DIRECTION('',(0.,0.,-1.)) ;
#32470 = DIRECTION('',(0.,-1.,0.)) ;
#32471 = DIRECTION('',(0.,0.,-1.)) ;
#32472 = DIRECTION('',(0.,1.,0.)) ;
#32473 = DIRECTION('',(0.,0.,-1.)) ;
#32474 = DIRECTION('',(0.,1.,0.)) ;
#32475 = DIRECTION('center_axis',(0.,1.,0.)) ;
#32476 = DIRECTION('ref_axis',(0.,0.,1.)) ;
#32477 = DIRECTION('',(1.,0.,0.)) ;
#32478 = DIRECTION('',(0.,0.,-1.)) ;
#32479 = DIRECTION('',(-1.,0.,0.)) ;
#32480 = DIRECTION('center_axis',(0.,0.,1.)) ;
#32481 = DIRECTION('ref_axis',(1.,0.,0.)) ;
#32482 = DIRECTION('',(-1.,0.,0.)) ;
#32483 = DIRECTION('',(0.,-1.,0.)) ;
#32484 = DIRECTION('',(1.,0.,0.)) ;
#32485 = DIRECTION('center_axis',(0.,1.,0.)) ;
#32486 = DIRECTION('ref_axis',(0.,0.,1.)) ;
#32487 = DIRECTION('',(0.,0.,-1.)) ;
#32488 = DIRECTION('',(-1.,0.,0.)) ;
#32489 = DIRECTION('center_axis',(0.,0.,1.)) ;
#32490 = DIRECTION('ref_axis',(1.,0.,0.)) ;
#32491 = DIRECTION('',(0.,-1.,0.)) ;
#32492 = DIRECTION('center_axis',(0.,0.,1.)) ;
#32493 = DIRECTION('ref_axis',(1.,0.,0.)) ;
#32494 = DIRECTION('',(0.,1.,0.)) ;
#32495 = DIRECTION('',(1.,0.,0.)) ;
#32496 = DIRECTION('center_axis',(1.,0.,0.)) ;
#32497 = DIRECTION('ref_axis',(0.,0.,-1.)) ;
#32498 = DIRECTION('',(0.,0.,-1.)) ;
#32499 = DIRECTION('',(0.,-1.,0.)) ;
#32500 = DIRECTION('center_axis',(0.,-1.,0.)) ;
#32501 = DIRECTION('ref_axis',(0.,0.,-1.)) ;
#32502 = DIRECTION('center_axis',(0.,0.,1.)) ;
#32503 = DIRECTION('ref_axis',(0.707106781186547,-0.707106781186548,0.)) ;
#32504 = DIRECTION('center_axis',(0.,0.,1.)) ;
#32505 = DIRECTION('ref_axis',(1.,0.,0.)) ;
#32506 = DIRECTION('',(0.707106781186547,-0.707106781186548,0.)) ;
#32507 = DIRECTION('',(0.707106781186548,0.707106781186547,0.)) ;
#32508 = DIRECTION('',(-0.707106781186547,0.707106781186548,0.)) ;
#32509 = DIRECTION('center_axis',(0.707106781186548,0.707106781186547,0.)) ;
#32510 = DIRECTION('ref_axis',(0.,0.,1.)) ;
#32511 = DIRECTION('',(-0.707106781186547,0.707106781186548,0.)) ;
#32512 = DIRECTION('',(0.,0.,-1.)) ;
#32513 = DIRECTION('center_axis',(-0.707106781186548,-0.707106781186547,0.)) ;
#32514 = DIRECTION('ref_axis',(0.,0.,-1.)) ;
#32515 = DIRECTION('',(0.,0.,-1.)) ;
#32516 = DIRECTION('',(0.707106781186547,-0.707106781186548,0.)) ;
#32517 = DIRECTION('center_axis',(-0.707106781186548,-0.707106781186547,0.)) ;
#32518 = DIRECTION('ref_axis',(0.,0.,-1.)) ;
#32519 = DIRECTION('',(0.707106781186547,-0.707106781186548,0.)) ;
#32520 = DIRECTION('',(0.,0.,-1.)) ;
#32521 = DIRECTION('',(-0.707106781186547,0.707106781186548,0.)) ;
#32522 = DIRECTION('center_axis',(0.,0.,1.)) ;
#32523 = DIRECTION('ref_axis',(0.707106781186547,-0.707106781186548,0.)) ;
#32524 = DIRECTION('center_axis',(0.,0.,-1.)) ;
#32525 = DIRECTION('ref_axis',(1.,0.,0.)) ;
#32526 = DIRECTION('',(-0.707106781186548,-0.707106781186547,0.)) ;
#32527 = DIRECTION('center_axis',(0.,0.,1.)) ;
#32528 = DIRECTION('ref_axis',(0.707106781186547,-0.707106781186548,0.)) ;
#32529 = DIRECTION('center_axis',(0.,0.,1.)) ;
#32530 = DIRECTION('ref_axis',(1.,0.,0.)) ;
#32531 = DIRECTION('',(-0.707106781186547,0.707106781186548,0.)) ;
#32532 = DIRECTION('',(0.707106781186548,0.707106781186547,0.)) ;
#32533 = DIRECTION('center_axis',(0.,0.,1.)) ;
#32534 = DIRECTION('ref_axis',(0.707106781186547,-0.707106781186548,0.)) ;
#32535 = DIRECTION('center_axis',(0.,0.,-1.)) ;
#32536 = DIRECTION('ref_axis',(1.,0.,0.)) ;
#32537 = DIRECTION('',(-0.707106781186548,-0.707106781186547,0.)) ;
#32538 = DIRECTION('',(0.707106781186547,-0.707106781186548,0.)) ;
#32539 = DIRECTION('center_axis',(0.707106781186548,0.707106781186547,0.)) ;
#32540 = DIRECTION('ref_axis',(0.,0.,1.)) ;
#32541 = DIRECTION('',(0.,0.,-1.)) ;
#32542 = DIRECTION('center_axis',(0.707106781186547,-0.707106781186548,0.)) ;
#32543 = DIRECTION('ref_axis',(0.,0.,-1.)) ;
#32544 = DIRECTION('center_axis',(-0.707106781186547,0.707106781186548,0.)) ;
#32545 = DIRECTION('ref_axis',(0.,0.,1.)) ;
#32546 = DIRECTION('center_axis',(0.,0.,1.)) ;
#32547 = DIRECTION('ref_axis',(-0.707106781186548,-0.707106781186547,0.)) ;
#32548 = DIRECTION('center_axis',(0.,0.,1.)) ;
#32549 = DIRECTION('ref_axis',(1.,0.,0.)) ;
#32550 = DIRECTION('',(-0.707106781186548,-0.707106781186547,0.)) ;
#32551 = DIRECTION('',(0.707106781186547,-0.707106781186548,0.)) ;
#32552 = DIRECTION('',(0.707106781186548,0.707106781186547,0.)) ;
#32553 = DIRECTION('center_axis',(0.707106781186547,-0.707106781186548,0.)) ;
#32554 = DIRECTION('ref_axis',(0.,0.,1.)) ;
#32555 = DIRECTION('',(0.707106781186548,0.707106781186547,0.)) ;
#32556 = DIRECTION('',(0.,0.,-1.)) ;
#32557 = DIRECTION('center_axis',(-0.707106781186547,0.707106781186548,0.)) ;
#32558 = DIRECTION('ref_axis',(0.,0.,-1.)) ;
#32559 = DIRECTION('',(0.,0.,-1.)) ;
#32560 = DIRECTION('',(-0.707106781186548,-0.707106781186547,0.)) ;
#32561 = DIRECTION('center_axis',(-0.707106781186547,0.707106781186548,0.)) ;
#32562 = DIRECTION('ref_axis',(0.,0.,-1.)) ;
#32563 = DIRECTION('',(-0.707106781186548,-0.707106781186547,0.)) ;
#32564 = DIRECTION('',(0.,0.,-1.)) ;
#32565 = DIRECTION('',(0.707106781186548,0.707106781186547,0.)) ;
#32566 = DIRECTION('center_axis',(0.,0.,1.)) ;
#32567 = DIRECTION('ref_axis',(-0.707106781186548,-0.707106781186547,0.)) ;
#32568 = DIRECTION('center_axis',(0.,0.,-1.)) ;
#32569 = DIRECTION('ref_axis',(1.,0.,0.)) ;
#32570 = DIRECTION('',(-0.707106781186547,0.707106781186548,0.)) ;
#32571 = DIRECTION('center_axis',(0.,0.,1.)) ;
#32572 = DIRECTION('ref_axis',(-0.707106781186548,-0.707106781186547,0.)) ;
#32573 = DIRECTION('center_axis',(0.,0.,1.)) ;
#32574 = DIRECTION('ref_axis',(1.,0.,0.)) ;
#32575 = DIRECTION('',(0.707106781186548,0.707106781186547,0.)) ;
#32576 = DIRECTION('',(0.707106781186547,-0.707106781186548,0.)) ;
#32577 = DIRECTION('center_axis',(0.,0.,1.)) ;
#32578 = DIRECTION('ref_axis',(-0.707106781186548,-0.707106781186547,0.)) ;
#32579 = DIRECTION('center_axis',(0.,0.,-1.)) ;
#32580 = DIRECTION('ref_axis',(1.,0.,0.)) ;
#32581 = DIRECTION('',(-0.707106781186547,0.707106781186548,0.)) ;
#32582 = DIRECTION('',(-0.707106781186548,-0.707106781186547,0.)) ;
#32583 = DIRECTION('center_axis',(0.707106781186547,-0.707106781186548,0.)) ;
#32584 = DIRECTION('ref_axis',(0.,0.,1.)) ;
#32585 = DIRECTION('',(0.,0.,-1.)) ;
#32586 = DIRECTION('center_axis',(-0.707106781186548,-0.707106781186547,0.)) ;
#32587 = DIRECTION('ref_axis',(0.,0.,-1.)) ;
#32588 = DIRECTION('center_axis',(0.707106781186548,0.707106781186547,0.)) ;
#32589 = DIRECTION('ref_axis',(0.,0.,1.)) ;
#32590 = DIRECTION('center_axis',(0.,0.,1.)) ;
#32591 = DIRECTION('ref_axis',(-0.707106781186547,0.707106781186548,0.)) ;
#32592 = DIRECTION('center_axis',(0.,0.,1.)) ;
#32593 = DIRECTION('ref_axis',(1.,0.,0.)) ;
#32594 = DIRECTION('',(-0.707106781186547,0.707106781186548,0.)) ;
#32595 = DIRECTION('',(-0.707106781186548,-0.707106781186547,0.)) ;
#32596 = DIRECTION('',(0.707106781186547,-0.707106781186548,0.)) ;
#32597 = DIRECTION('center_axis',(-0.707106781186548,-0.707106781186547,0.)) ;
#32598 = DIRECTION('ref_axis',(0.,0.,1.)) ;
#32599 = DIRECTION('',(0.707106781186547,-0.707106781186548,0.)) ;
#32600 = DIRECTION('',(0.,0.,-1.)) ;
#32601 = DIRECTION('center_axis',(0.707106781186548,0.707106781186547,0.)) ;
#32602 = DIRECTION('ref_axis',(0.,0.,-1.)) ;
#32603 = DIRECTION('',(0.,0.,-1.)) ;
#32604 = DIRECTION('',(-0.707106781186547,0.707106781186548,0.)) ;
#32605 = DIRECTION('center_axis',(0.707106781186548,0.707106781186547,0.)) ;
#32606 = DIRECTION('ref_axis',(0.,0.,-1.)) ;
#32607 = DIRECTION('',(-0.707106781186547,0.707106781186548,0.)) ;
#32608 = DIRECTION('',(0.,0.,-1.)) ;
#32609 = DIRECTION('',(0.707106781186547,-0.707106781186548,0.)) ;
#32610 = DIRECTION('center_axis',(0.,0.,1.)) ;
#32611 = DIRECTION('ref_axis',(-0.707106781186547,0.707106781186548,0.)) ;
#32612 = DIRECTION('center_axis',(0.,0.,-1.)) ;
#32613 = DIRECTION('ref_axis',(1.,0.,0.)) ;
#32614 = DIRECTION('',(0.707106781186548,0.707106781186547,0.)) ;
#32615 = DIRECTION('center_axis',(0.,0.,1.)) ;
#32616 = DIRECTION('ref_axis',(-0.707106781186547,0.707106781186548,0.)) ;
#32617 = DIRECTION('center_axis',(0.,0.,1.)) ;
#32618 = DIRECTION('ref_axis',(1.,0.,0.)) ;
#32619 = DIRECTION('',(0.707106781186547,-0.707106781186548,0.)) ;
#32620 = DIRECTION('',(-0.707106781186548,-0.707106781186547,0.)) ;
#32621 = DIRECTION('center_axis',(0.,0.,1.)) ;
#32622 = DIRECTION('ref_axis',(-0.707106781186547,0.707106781186548,0.)) ;
#32623 = DIRECTION('center_axis',(0.,0.,-1.)) ;
#32624 = DIRECTION('ref_axis',(1.,0.,0.)) ;
#32625 = DIRECTION('',(0.707106781186548,0.707106781186547,0.)) ;
#32626 = DIRECTION('',(-0.707106781186547,0.707106781186548,0.)) ;
#32627 = DIRECTION('center_axis',(-0.707106781186548,-0.707106781186547,0.)) ;
#32628 = DIRECTION('ref_axis',(0.,0.,1.)) ;
#32629 = DIRECTION('',(0.,0.,-1.)) ;
#32630 = DIRECTION('center_axis',(-0.707106781186547,0.707106781186548,0.)) ;
#32631 = DIRECTION('ref_axis',(0.,0.,-1.)) ;
#32632 = DIRECTION('center_axis',(0.707106781186547,-0.707106781186548,0.)) ;
#32633 = DIRECTION('ref_axis',(0.,0.,1.)) ;
#32634 = DIRECTION('center_axis',(0.,0.,1.)) ;
#32635 = DIRECTION('ref_axis',(0.707106781186548,0.707106781186547,0.)) ;
#32636 = DIRECTION('center_axis',(0.,0.,1.)) ;
#32637 = DIRECTION('ref_axis',(1.,0.,0.)) ;
#32638 = DIRECTION('',(0.707106781186548,0.707106781186547,0.)) ;
#32639 = DIRECTION('',(-0.707106781186547,0.707106781186548,0.)) ;
#32640 = DIRECTION('',(-0.707106781186548,-0.707106781186547,0.)) ;
#32641 = DIRECTION('center_axis',(-0.707106781186547,0.707106781186548,0.)) ;
#32642 = DIRECTION('ref_axis',(0.,0.,1.)) ;
#32643 = DIRECTION('',(-0.707106781186548,-0.707106781186547,0.)) ;
#32644 = DIRECTION('',(0.,0.,-1.)) ;
#32645 = DIRECTION('center_axis',(0.707106781186547,-0.707106781186548,0.)) ;
#32646 = DIRECTION('ref_axis',(0.,0.,-1.)) ;
#32647 = DIRECTION('',(0.,0.,-1.)) ;
#32648 = DIRECTION('',(0.707106781186548,0.707106781186547,0.)) ;
#32649 = DIRECTION('center_axis',(0.707106781186547,-0.707106781186548,0.)) ;
#32650 = DIRECTION('ref_axis',(0.,0.,-1.)) ;
#32651 = DIRECTION('',(0.707106781186548,0.707106781186547,0.)) ;
#32652 = DIRECTION('',(0.,0.,-1.)) ;
#32653 = DIRECTION('',(-0.707106781186548,-0.707106781186547,0.)) ;
#32654 = DIRECTION('center_axis',(0.,0.,1.)) ;
#32655 = DIRECTION('ref_axis',(0.707106781186548,0.707106781186547,0.)) ;
#32656 = DIRECTION('center_axis',(0.,0.,-1.)) ;
#32657 = DIRECTION('ref_axis',(1.,0.,0.)) ;
#32658 = DIRECTION('',(0.707106781186547,-0.707106781186548,0.)) ;
#32659 = DIRECTION('center_axis',(0.,0.,1.)) ;
#32660 = DIRECTION('ref_axis',(0.707106781186548,0.707106781186547,0.)) ;
#32661 = DIRECTION('center_axis',(0.,0.,1.)) ;
#32662 = DIRECTION('ref_axis',(1.,0.,0.)) ;
#32663 = DIRECTION('',(-0.707106781186548,-0.707106781186547,0.)) ;
#32664 = DIRECTION('',(-0.707106781186547,0.707106781186548,0.)) ;
#32665 = DIRECTION('center_axis',(0.,0.,1.)) ;
#32666 = DIRECTION('ref_axis',(0.707106781186548,0.707106781186547,0.)) ;
#32667 = DIRECTION('center_axis',(0.,0.,-1.)) ;
#32668 = DIRECTION('ref_axis',(1.,0.,0.)) ;
#32669 = DIRECTION('',(0.707106781186547,-0.707106781186548,0.)) ;
#32670 = DIRECTION('',(0.707106781186548,0.707106781186547,0.)) ;
#32671 = DIRECTION('center_axis',(-0.707106781186547,0.707106781186548,0.)) ;
#32672 = DIRECTION('ref_axis',(0.,0.,1.)) ;
#32673 = DIRECTION('',(0.,0.,-1.)) ;
#32674 = DIRECTION('center_axis',(0.707106781186548,0.707106781186547,0.)) ;
#32675 = DIRECTION('ref_axis',(0.,0.,-1.)) ;
#32676 = DIRECTION('center_axis',(-0.707106781186548,-0.707106781186547,0.)) ;
#32677 = DIRECTION('ref_axis',(0.,0.,1.)) ;
#32678 = DIRECTION('center_axis',(0.,0.,1.)) ;
#32679 = DIRECTION('ref_axis',(1.,0.,0.)) ;
#32680 = DIRECTION('center_axis',(0.,0.,1.)) ;
#32681 = DIRECTION('ref_axis',(1.,0.,0.)) ;
#32682 = DIRECTION('',(0.,0.,1.)) ;
#32683 = DIRECTION('center_axis',(0.,0.,-1.)) ;
#32684 = DIRECTION('ref_axis',(1.,0.,0.)) ;
#32685 = DIRECTION('center_axis',(0.,0.,1.)) ;
#32686 = DIRECTION('ref_axis',(1.,0.,0.)) ;
#32687 = DIRECTION('center_axis',(0.,0.,-1.)) ;
#32688 = DIRECTION('ref_axis',(1.,0.,0.)) ;
#32689 = DIRECTION('',(0.,0.,1.)) ;
#32690 = DIRECTION('center_axis',(0.,0.,-1.)) ;
#32691 = DIRECTION('ref_axis',(1.,0.,0.)) ;
#32692 = DIRECTION('center_axis',(0.,0.,-1.)) ;
#32693 = DIRECTION('ref_axis',(-1.,0.,0.)) ;
#32694 = DIRECTION('center_axis',(0.,0.,1.)) ;
#32695 = DIRECTION('ref_axis',(1.,0.,0.)) ;
#32696 = DIRECTION('center_axis',(0.,0.,1.)) ;
#32697 = DIRECTION('ref_axis',(1.,0.,0.)) ;
#32698 = DIRECTION('center_axis',(0.,0.,1.)) ;
#32699 = DIRECTION('ref_axis',(1.,0.,0.)) ;
#32700 = DIRECTION('',(-0.565399080761227,-6.92414174495092E-17,0.824817482522261)) ;
#32701 = DIRECTION('center_axis',(0.,0.,1.)) ;
#32702 = DIRECTION('ref_axis',(1.,0.,0.)) ;
#32703 = DIRECTION('',(0.565399080761227,6.92414174495092E-17,-0.824817482522261)) ;
#32704 = DIRECTION('center_axis',(0.,0.,-1.)) ;
#32705 = DIRECTION('ref_axis',(1.,0.,0.)) ;
#32706 = DIRECTION('center_axis',(0.,0.,-1.)) ;
#32707 = DIRECTION('ref_axis',(-1.,0.,0.)) ;
#32708 = DIRECTION('axis',(0.,0.,1.)) ;
#32709 = DIRECTION('refdir',(1.,0.,0.)) ;
#32710 = DIRECTION('center_axis',(0.,0.,1.)) ;
#32711 = DIRECTION('ref_axis',(1.,0.,0.)) ;
#32712 = DIRECTION('',(-1.,0.,0.)) ;
#32713 = DIRECTION('',(0.,1.,0.)) ;
#32714 = DIRECTION('',(1.,0.,0.)) ;
#32715 = DIRECTION('',(0.,-1.,0.)) ;
#32716 = DIRECTION('center_axis',(1.,0.,0.)) ;
#32717 = DIRECTION('ref_axis',(0.,0.,-1.)) ;
#32718 = DIRECTION('',(0.,0.,-1.)) ;
#32719 = DIRECTION('',(0.,0.,1.)) ;
#32720 = DIRECTION('',(0.,1.,0.)) ;
#32721 = DIRECTION('center_axis',(-1.,0.,0.)) ;
#32722 = DIRECTION('ref_axis',(0.,0.,1.)) ;
#32723 = DIRECTION('',(0.,0.,1.)) ;
#32724 = DIRECTION('',(0.,-1.,0.)) ;
#32725 = DIRECTION('',(0.,0.,-1.)) ;
#32726 = DIRECTION('center_axis',(0.,-1.,0.)) ;
#32727 = DIRECTION('ref_axis',(0.,0.,-1.)) ;
#32728 = DIRECTION('',(1.,0.,0.)) ;
#32729 = DIRECTION('',(0.,0.,-1.)) ;
#32730 = DIRECTION('',(-1.,0.,0.)) ;
#32731 = DIRECTION('',(0.,0.,-1.)) ;
#32732 = DIRECTION('',(1.,0.,0.)) ;
#32733 = DIRECTION('center_axis',(0.,1.,0.)) ;
#32734 = DIRECTION('ref_axis',(0.,0.,1.)) ;
#32735 = DIRECTION('',(-1.,0.,0.)) ;
#32736 = DIRECTION('',(0.,0.,-1.)) ;
#32737 = DIRECTION('',(1.,0.,0.)) ;
#32738 = DIRECTION('',(0.,0.,-1.)) ;
#32739 = DIRECTION('',(-1.,0.,0.)) ;
#32740 = DIRECTION('center_axis',(0.,0.,1.)) ;
#32741 = DIRECTION('ref_axis',(1.,0.,0.)) ;
#32742 = DIRECTION('',(0.,1.,0.)) ;
#32743 = DIRECTION('',(0.,-1.,0.)) ;
#32744 = DIRECTION('center_axis',(1.,0.,0.)) ;
#32745 = DIRECTION('ref_axis',(0.,0.,-1.)) ;
#32746 = DIRECTION('',(0.,1.,0.)) ;
#32747 = DIRECTION('center_axis',(-1.,0.,0.)) ;
#32748 = DIRECTION('ref_axis',(0.,0.,1.)) ;
#32749 = DIRECTION('',(0.,-1.,0.)) ;
#32750 = DIRECTION('center_axis',(0.,0.,1.)) ;
#32751 = DIRECTION('ref_axis',(1.,0.,0.)) ;
#32752 = DIRECTION('center_axis',(0.,0.,1.)) ;
#32753 = DIRECTION('ref_axis',(1.,0.,0.)) ;
#32754 = DIRECTION('',(0.,0.,1.)) ;
#32755 = DIRECTION('center_axis',(0.,0.,-1.)) ;
#32756 = DIRECTION('ref_axis',(1.,0.,0.)) ;
#32757 = DIRECTION('center_axis',(0.,0.,-1.)) ;
#32758 = DIRECTION('ref_axis',(-1.,0.,0.)) ;
#32759 = DIRECTION('center_axis',(0.,0.,-1.)) ;
#32760 = DIRECTION('ref_axis',(1.,0.,0.)) ;
#32761 = DIRECTION('center_axis',(0.,0.,1.)) ;
#32762 = DIRECTION('ref_axis',(1.,0.,0.)) ;
#32763 = DIRECTION('center_axis',(0.,0.,1.)) ;
#32764 = DIRECTION('ref_axis',(1.,0.,0.)) ;
#32765 = DIRECTION('',(0.,0.,-1.)) ;
#32766 = DIRECTION('center_axis',(0.,0.,-1.)) ;
#32767 = DIRECTION('ref_axis',(-1.,0.,0.)) ;
#32768 = DIRECTION('center_axis',(0.,0.,1.)) ;
#32769 = DIRECTION('ref_axis',(1.,0.,0.)) ;
#32770 = DIRECTION('axis',(0.,0.,1.)) ;
#32771 = DIRECTION('refdir',(1.,0.,0.)) ;
#32772 = DIRECTION('center_axis',(0.,0.,1.)) ;
#32773 = DIRECTION('ref_axis',(1.,0.,0.)) ;
#32774 = DIRECTION('',(1.,0.,0.)) ;
#32775 = DIRECTION('',(0.,-1.,0.)) ;
#32776 = DIRECTION('',(1.,0.,0.)) ;
#32777 = DIRECTION('',(0.,1.,0.)) ;
#32778 = DIRECTION('center_axis',(0.,0.,1.)) ;
#32779 = DIRECTION('ref_axis',(1.,0.,0.)) ;
#32780 = DIRECTION('',(-1.,0.,0.)) ;
#32781 = DIRECTION('',(0.,-1.,0.)) ;
#32782 = DIRECTION('',(-1.,0.,0.)) ;
#32783 = DIRECTION('',(0.,1.,0.)) ;
#32784 = DIRECTION('center_axis',(0.,1.,0.)) ;
#32785 = DIRECTION('ref_axis',(0.,0.,1.)) ;
#32786 = DIRECTION('',(0.,0.,-1.)) ;
#32787 = DIRECTION('',(0.,0.,-1.)) ;
#32788 = DIRECTION('center_axis',(1.,0.,0.)) ;
#32789 = DIRECTION('ref_axis',(0.,0.,-1.)) ;
#32790 = DIRECTION('center_axis',(1.,0.,0.)) ;
#32791 = DIRECTION('ref_axis',(0.,0.,-1.)) ;
#32792 = DIRECTION('center_axis',(1.,0.,0.)) ;
#32793 = DIRECTION('ref_axis',(0.,1.,1.83697019872103E-16)) ;
#32794 = DIRECTION('center_axis',(-1.,0.,0.)) ;
#32795 = DIRECTION('ref_axis',(0.,0.,-1.)) ;
#32796 = DIRECTION('center_axis',(-1.,0.,0.)) ;
#32797 = DIRECTION('ref_axis',(0.,0.,1.)) ;
#32798 = DIRECTION('axis',(0.,0.,1.)) ;
#32799 = DIRECTION('refdir',(1.,0.,0.)) ;
#32800 = DIRECTION('center_axis',(1.,0.,0.)) ;
#32801 = DIRECTION('ref_axis',(0.,0.,-1.)) ;
#32802 = DIRECTION('',(0.,0.,1.)) ;
#32803 = DIRECTION('',(0.,1.,0.)) ;
#32804 = DIRECTION('',(0.,0.,-1.)) ;
#32805 = DIRECTION('',(0.,-1.,0.)) ;
#32806 = DIRECTION('center_axis',(1.,0.,0.)) ;
#32807 = DIRECTION('ref_axis',(0.,0.,-1.)) ;
#32808 = DIRECTION('',(0.,0.,1.)) ;
#32809 = DIRECTION('',(0.,1.,0.)) ;
#32810 = DIRECTION('',(0.,0.,-1.)) ;
#32811 = DIRECTION('',(0.,-1.,0.)) ;
#32812 = DIRECTION('center_axis',(1.,0.,0.)) ;
#32813 = DIRECTION('ref_axis',(0.,0.,-1.)) ;
#32814 = DIRECTION('',(0.,0.,1.)) ;
#32815 = DIRECTION('',(0.,1.,0.)) ;
#32816 = DIRECTION('',(0.,0.,-1.)) ;
#32817 = DIRECTION('',(0.,-1.,0.)) ;
#32818 = DIRECTION('center_axis',(1.,0.,0.)) ;
#32819 = DIRECTION('ref_axis',(0.,0.,-1.)) ;
#32820 = DIRECTION('',(0.,0.,1.)) ;
#32821 = DIRECTION('',(0.,1.,0.)) ;
#32822 = DIRECTION('',(0.,0.,-1.)) ;
#32823 = DIRECTION('',(0.,-1.,0.)) ;
#32824 = DIRECTION('center_axis',(1.,0.,0.)) ;
#32825 = DIRECTION('ref_axis',(0.,0.,-1.)) ;
#32826 = DIRECTION('',(0.,0.,1.)) ;
#32827 = DIRECTION('',(0.,1.,0.)) ;
#32828 = DIRECTION('',(0.,0.,-1.)) ;
#32829 = DIRECTION('',(0.,-1.,0.)) ;
#32830 = DIRECTION('center_axis',(1.,0.,0.)) ;
#32831 = DIRECTION('ref_axis',(0.,0.,-1.)) ;
#32832 = DIRECTION('',(0.,0.,1.)) ;
#32833 = DIRECTION('',(0.,1.,0.)) ;
#32834 = DIRECTION('',(0.,0.,-1.)) ;
#32835 = DIRECTION('',(0.,-1.,0.)) ;
#32836 = DIRECTION('center_axis',(-1.,0.,0.)) ;
#32837 = DIRECTION('ref_axis',(0.,0.,1.)) ;
#32838 = DIRECTION('',(0.,0.,1.)) ;
#32839 = DIRECTION('',(0.,-1.,0.)) ;
#32840 = DIRECTION('',(0.,0.,-1.)) ;
#32841 = DIRECTION('',(0.,1.,0.)) ;
#32842 = DIRECTION('center_axis',(-1.,0.,0.)) ;
#32843 = DIRECTION('ref_axis',(0.,0.,1.)) ;
#32844 = DIRECTION('',(0.,0.,-1.)) ;
#32845 = DIRECTION('',(0.,1.,0.)) ;
#32846 = DIRECTION('',(0.,0.,-1.)) ;
#32847 = DIRECTION('',(0.,-1.,0.)) ;
#32848 = DIRECTION('center_axis',(-1.,0.,0.)) ;
#32849 = DIRECTION('ref_axis',(0.,0.,1.)) ;
#32850 = DIRECTION('',(0.,0.,-1.)) ;
#32851 = DIRECTION('',(0.,1.,0.)) ;
#32852 = DIRECTION('',(0.,0.,1.)) ;
#32853 = DIRECTION('',(0.,-1.,0.)) ;
#32854 = DIRECTION('center_axis',(-1.,0.,0.)) ;
#32855 = DIRECTION('ref_axis',(0.,0.,1.)) ;
#32856 = DIRECTION('',(0.,0.,-1.)) ;
#32857 = DIRECTION('',(0.,1.,0.)) ;
#32858 = DIRECTION('',(0.,0.,1.)) ;
#32859 = DIRECTION('',(0.,-1.,0.)) ;
#32860 = DIRECTION('center_axis',(-1.,0.,0.)) ;
#32861 = DIRECTION('ref_axis',(0.,0.,1.)) ;
#32862 = DIRECTION('',(0.,0.,-1.)) ;
#32863 = DIRECTION('',(0.,1.,0.)) ;
#32864 = DIRECTION('',(0.,0.,1.)) ;
#32865 = DIRECTION('',(0.,-1.,0.)) ;
#32866 = DIRECTION('center_axis',(-1.,0.,0.)) ;
#32867 = DIRECTION('ref_axis',(0.,0.,1.)) ;
#32868 = DIRECTION('',(0.,0.,-1.)) ;
#32869 = DIRECTION('',(0.,1.,0.)) ;
#32870 = DIRECTION('',(0.,0.,1.)) ;
#32871 = DIRECTION('',(0.,-1.,0.)) ;
#32872 = DIRECTION('center_axis',(0.,1.,0.)) ;
#32873 = DIRECTION('ref_axis',(0.,0.,1.)) ;
#32874 = DIRECTION('',(0.,0.,1.)) ;
#32875 = DIRECTION('',(-1.,0.,0.)) ;
#32876 = DIRECTION('',(1.,0.,0.)) ;
#32877 = DIRECTION('center_axis',(0.,-1.,0.)) ;
#32878 = DIRECTION('ref_axis',(0.,0.,-1.)) ;
#32879 = DIRECTION('',(0.,0.,-1.)) ;
#32880 = DIRECTION('',(-1.,0.,0.)) ;
#32881 = DIRECTION('',(1.,0.,0.)) ;
#32882 = DIRECTION('center_axis',(0.,0.,1.)) ;
#32883 = DIRECTION('ref_axis',(1.,0.,0.)) ;
#32884 = DIRECTION('center_axis',(0.,0.,1.)) ;
#32885 = DIRECTION('ref_axis',(1.,0.,0.)) ;
#32886 = DIRECTION('',(0.,0.,-1.)) ;
#32887 = DIRECTION('center_axis',(0.,0.,-1.)) ;
#32888 = DIRECTION('ref_axis',(1.,0.,0.)) ;
#32889 = DIRECTION('center_axis',(0.,0.,1.)) ;
#32890 = DIRECTION('ref_axis',(1.,0.,0.)) ;
#32891 = DIRECTION('center_axis',(0.,0.,-1.)) ;
#32892 = DIRECTION('ref_axis',(1.,0.,0.)) ;
#32893 = DIRECTION('',(0.,0.,1.)) ;
#32894 = DIRECTION('center_axis',(0.,0.,1.)) ;
#32895 = DIRECTION('ref_axis',(1.,0.,0.)) ;
#32896 = DIRECTION('center_axis',(0.,0.,1.)) ;
#32897 = DIRECTION('ref_axis',(1.,0.,0.)) ;
#32898 = DIRECTION('center_axis',(0.,0.,1.)) ;
#32899 = DIRECTION('ref_axis',(1.,0.,0.)) ;
#32900 = DIRECTION('',(0.,0.,1.)) ;
#32901 = DIRECTION('center_axis',(0.,0.,-1.)) ;
#32902 = DIRECTION('ref_axis',(1.,0.,0.)) ;
#32903 = DIRECTION('center_axis',(0.,-1.,0.)) ;
#32904 = DIRECTION('ref_axis',(0.,0.,-1.)) ;
#32905 = DIRECTION('',(1.,0.,0.)) ;
#32906 = DIRECTION('',(0.,0.,1.)) ;
#32907 = DIRECTION('',(-1.,0.,0.)) ;
#32908 = DIRECTION('center_axis',(0.,1.,0.)) ;
#32909 = DIRECTION('ref_axis',(0.,0.,1.)) ;
#32910 = DIRECTION('',(-1.,0.,0.)) ;
#32911 = DIRECTION('',(0.,0.,-1.)) ;
#32912 = DIRECTION('',(1.,0.,0.)) ;
#32913 = DIRECTION('center_axis',(0.,-1.,0.)) ;
#32914 = DIRECTION('ref_axis',(0.,0.,-1.)) ;
#32915 = DIRECTION('',(1.,0.,0.)) ;
#32916 = DIRECTION('',(0.,0.,1.)) ;
#32917 = DIRECTION('',(-1.,0.,0.)) ;
#32918 = DIRECTION('center_axis',(0.,1.,0.)) ;
#32919 = DIRECTION('ref_axis',(0.,0.,1.)) ;
#32920 = DIRECTION('',(-1.,0.,0.)) ;
#32921 = DIRECTION('',(0.,0.,-1.)) ;
#32922 = DIRECTION('',(1.,0.,0.)) ;
#32923 = DIRECTION('center_axis',(0.,-1.,0.)) ;
#32924 = DIRECTION('ref_axis',(0.,0.,-1.)) ;
#32925 = DIRECTION('',(1.,0.,0.)) ;
#32926 = DIRECTION('',(0.,0.,1.)) ;
#32927 = DIRECTION('',(-1.,0.,0.)) ;
#32928 = DIRECTION('center_axis',(0.,1.,0.)) ;
#32929 = DIRECTION('ref_axis',(0.,0.,1.)) ;
#32930 = DIRECTION('',(-1.,0.,0.)) ;
#32931 = DIRECTION('',(0.,0.,-1.)) ;
#32932 = DIRECTION('',(1.,0.,0.)) ;
#32933 = DIRECTION('center_axis',(0.,-1.,0.)) ;
#32934 = DIRECTION('ref_axis',(0.,0.,-1.)) ;
#32935 = DIRECTION('',(1.,0.,0.)) ;
#32936 = DIRECTION('',(0.,0.,1.)) ;
#32937 = DIRECTION('',(-1.,0.,0.)) ;
#32938 = DIRECTION('center_axis',(0.,-1.,0.)) ;
#32939 = DIRECTION('ref_axis',(0.,0.,-1.)) ;
#32940 = DIRECTION('',(1.,0.,0.)) ;
#32941 = DIRECTION('',(0.,0.,1.)) ;
#32942 = DIRECTION('',(-1.,0.,0.)) ;
#32943 = DIRECTION('center_axis',(0.,0.,1.)) ;
#32944 = DIRECTION('ref_axis',(1.,0.,0.)) ;
#32945 = DIRECTION('',(0.,1.,0.)) ;
#32946 = DIRECTION('',(-1.,0.,0.)) ;
#32947 = DIRECTION('center_axis',(0.,0.,1.)) ;
#32948 = DIRECTION('ref_axis',(1.,0.,0.)) ;
#32949 = DIRECTION('',(0.,1.,0.)) ;
#32950 = DIRECTION('',(-1.,0.,0.)) ;
#32951 = DIRECTION('center_axis',(0.,0.,1.)) ;
#32952 = DIRECTION('ref_axis',(1.,0.,0.)) ;
#32953 = DIRECTION('',(0.,1.,0.)) ;
#32954 = DIRECTION('',(-1.,0.,0.)) ;
#32955 = DIRECTION('center_axis',(0.,0.,1.)) ;
#32956 = DIRECTION('ref_axis',(1.,0.,0.)) ;
#32957 = DIRECTION('',(0.,1.,0.)) ;
#32958 = DIRECTION('',(-1.,0.,0.)) ;
#32959 = DIRECTION('',(0.,-1.,0.)) ;
#32960 = DIRECTION('center_axis',(0.,0.,1.)) ;
#32961 = DIRECTION('ref_axis',(1.,0.,0.)) ;
#32962 = DIRECTION('',(-1.,0.,0.)) ;
#32963 = DIRECTION('',(0.,-1.,0.)) ;
#32964 = DIRECTION('center_axis',(0.,0.,1.)) ;
#32965 = DIRECTION('ref_axis',(1.,0.,0.)) ;
#32966 = DIRECTION('',(-1.,0.,0.)) ;
#32967 = DIRECTION('',(0.,-1.,0.)) ;
#32968 = DIRECTION('center_axis',(0.,0.,1.)) ;
#32969 = DIRECTION('ref_axis',(1.,0.,0.)) ;
#32970 = DIRECTION('',(-1.,0.,0.)) ;
#32971 = DIRECTION('',(0.,-1.,0.)) ;
#32972 = DIRECTION('center_axis',(0.,0.,1.)) ;
#32973 = DIRECTION('ref_axis',(1.,0.,0.)) ;
#32974 = DIRECTION('',(-1.,0.,0.)) ;
#32975 = DIRECTION('',(0.,-1.,0.)) ;
#32976 = DIRECTION('center_axis',(0.,0.,1.)) ;
#32977 = DIRECTION('ref_axis',(1.,0.,0.)) ;
#32978 = DIRECTION('',(-1.,0.,0.)) ;
#32979 = DIRECTION('',(0.,-1.,0.)) ;
#32980 = DIRECTION('center_axis',(0.,0.,1.)) ;
#32981 = DIRECTION('ref_axis',(1.,0.,0.)) ;
#32982 = DIRECTION('',(-1.,0.,0.)) ;
#32983 = DIRECTION('',(0.,-1.,0.)) ;
#32984 = DIRECTION('center_axis',(0.,0.,1.)) ;
#32985 = DIRECTION('ref_axis',(1.,0.,0.)) ;
#32986 = DIRECTION('',(-1.,0.,0.)) ;
#32987 = DIRECTION('',(0.,-1.,0.)) ;
#32988 = DIRECTION('',(1.,0.,0.)) ;
#32989 = DIRECTION('center_axis',(0.,0.,1.)) ;
#32990 = DIRECTION('ref_axis',(1.,0.,0.)) ;
#32991 = DIRECTION('',(0.,-1.,0.)) ;
#32992 = DIRECTION('',(1.,0.,0.)) ;
#32993 = DIRECTION('center_axis',(0.,0.,1.)) ;
#32994 = DIRECTION('ref_axis',(1.,0.,0.)) ;
#32995 = DIRECTION('',(0.,-1.,0.)) ;
#32996 = DIRECTION('',(1.,0.,0.)) ;
#32997 = DIRECTION('center_axis',(0.,0.,1.)) ;
#32998 = DIRECTION('ref_axis',(1.,0.,0.)) ;
#32999 = DIRECTION('',(0.,-1.,0.)) ;
#33000 = DIRECTION('',(1.,0.,0.)) ;
#33001 = DIRECTION('center_axis',(0.,0.,1.)) ;
#33002 = DIRECTION('ref_axis',(1.,0.,0.)) ;
#33003 = DIRECTION('',(0.,-1.,0.)) ;
#33004 = DIRECTION('',(1.,0.,0.)) ;
#33005 = DIRECTION('center_axis',(0.,0.,1.)) ;
#33006 = DIRECTION('ref_axis',(1.,0.,0.)) ;
#33007 = DIRECTION('',(0.,-1.,0.)) ;
#33008 = DIRECTION('',(1.,0.,0.)) ;
#33009 = DIRECTION('center_axis',(0.,0.,1.)) ;
#33010 = DIRECTION('ref_axis',(1.,0.,0.)) ;
#33011 = DIRECTION('',(0.,-1.,0.)) ;
#33012 = DIRECTION('',(1.,0.,0.)) ;
#33013 = DIRECTION('center_axis',(0.,0.,1.)) ;
#33014 = DIRECTION('ref_axis',(1.,0.,0.)) ;
#33015 = DIRECTION('',(0.,-1.,0.)) ;
#33016 = DIRECTION('',(1.,0.,0.)) ;
#33017 = DIRECTION('',(0.,1.,0.)) ;
#33018 = DIRECTION('center_axis',(0.,0.,1.)) ;
#33019 = DIRECTION('ref_axis',(1.,0.,0.)) ;
#33020 = DIRECTION('',(1.,0.,0.)) ;
#33021 = DIRECTION('',(0.,1.,0.)) ;
#33022 = DIRECTION('center_axis',(0.,0.,1.)) ;
#33023 = DIRECTION('ref_axis',(1.,0.,0.)) ;
#33024 = DIRECTION('',(1.,0.,0.)) ;
#33025 = DIRECTION('',(0.,1.,0.)) ;
#33026 = DIRECTION('center_axis',(0.,0.,1.)) ;
#33027 = DIRECTION('ref_axis',(1.,0.,0.)) ;
#33028 = DIRECTION('',(1.,0.,0.)) ;
#33029 = DIRECTION('',(0.,1.,0.)) ;
#33030 = DIRECTION('center_axis',(0.,0.,1.)) ;
#33031 = DIRECTION('ref_axis',(1.,0.,0.)) ;
#33032 = DIRECTION('center_axis',(0.,0.,1.)) ;
#33033 = DIRECTION('ref_axis',(1.,0.,0.)) ;
#33034 = DIRECTION('',(1.,0.,0.)) ;
#33035 = DIRECTION('',(0.,1.,0.)) ;
#33036 = DIRECTION('center_axis',(0.,0.,1.)) ;
#33037 = DIRECTION('ref_axis',(1.,0.,0.)) ;
#33038 = DIRECTION('',(1.,0.,0.)) ;
#33039 = DIRECTION('',(0.,1.,0.)) ;
#33040 = DIRECTION('center_axis',(0.,0.,1.)) ;
#33041 = DIRECTION('ref_axis',(1.,0.,0.)) ;
#33042 = DIRECTION('',(1.,0.,0.)) ;
#33043 = DIRECTION('',(0.,1.,0.)) ;
#33044 = DIRECTION('',(-1.,0.,0.)) ;
#33045 = DIRECTION('center_axis',(0.,0.,1.)) ;
#33046 = DIRECTION('ref_axis',(1.,0.,0.)) ;
#33047 = DIRECTION('',(0.,1.,0.)) ;
#33048 = DIRECTION('',(-1.,0.,0.)) ;
#33049 = DIRECTION('center_axis',(0.,0.,1.)) ;
#33050 = DIRECTION('ref_axis',(1.,0.,0.)) ;
#33051 = DIRECTION('',(0.,1.,0.)) ;
#33052 = DIRECTION('',(-1.,0.,0.)) ;
#33053 = DIRECTION('',(-1.,0.,0.)) ;
#33054 = DIRECTION('center_axis',(0.,0.,-1.)) ;
#33055 = DIRECTION('ref_axis',(1.,0.,0.)) ;
#33056 = DIRECTION('',(-1.,0.,0.)) ;
#33057 = DIRECTION('center_axis',(0.,0.,-1.)) ;
#33058 = DIRECTION('ref_axis',(1.,0.,0.)) ;
#33059 = DIRECTION('',(-1.,0.,0.)) ;
#33060 = DIRECTION('center_axis',(0.,0.,-1.)) ;
#33061 = DIRECTION('ref_axis',(1.,0.,0.)) ;
#33062 = DIRECTION('',(0.,1.,0.)) ;
#33063 = DIRECTION('',(1.,0.,0.)) ;
#33064 = DIRECTION('',(0.,1.,0.)) ;
#33065 = DIRECTION('',(1.,0.,0.)) ;
#33066 = DIRECTION('',(0.,1.,0.)) ;
#33067 = DIRECTION('',(1.,0.,0.)) ;
#33068 = DIRECTION('',(0.,1.,0.)) ;
#33069 = DIRECTION('',(1.,0.,0.)) ;
#33070 = DIRECTION('',(0.,1.,0.)) ;
#33071 = DIRECTION('',(1.,0.,0.)) ;
#33072 = DIRECTION('center_axis',(0.,0.,-1.)) ;
#33073 = DIRECTION('ref_axis',(1.,0.,0.)) ;
#33074 = DIRECTION('',(0.,1.,0.)) ;
#33075 = DIRECTION('center_axis',(0.,0.,-1.)) ;
#33076 = DIRECTION('ref_axis',(1.,0.,0.)) ;
#33077 = DIRECTION('',(-1.,0.,0.)) ;
#33078 = DIRECTION('',(0.,-1.,0.)) ;
#33079 = DIRECTION('',(-1.,0.,0.)) ;
#33080 = DIRECTION('',(0.,1.,0.)) ;
#33081 = DIRECTION('',(1.,0.,0.)) ;
#33082 = DIRECTION('',(0.,-1.,0.)) ;
#33083 = DIRECTION('',(-1.,0.,0.)) ;
#33084 = DIRECTION('',(0.,1.,0.)) ;
#33085 = DIRECTION('',(1.,0.,0.)) ;
#33086 = DIRECTION('',(0.,-1.,0.)) ;
#33087 = DIRECTION('',(-1.,0.,0.)) ;
#33088 = DIRECTION('',(0.,1.,0.)) ;
#33089 = DIRECTION('',(1.,0.,0.)) ;
#33090 = DIRECTION('',(1.,0.,0.)) ;
#33091 = DIRECTION('',(0.,-1.,0.)) ;
#33092 = DIRECTION('',(-1.,0.,0.)) ;
#33093 = DIRECTION('',(0.,1.,0.)) ;
#33094 = DIRECTION('',(-1.,0.,0.)) ;
#33095 = DIRECTION('',(0.,1.,0.)) ;
#33096 = DIRECTION('center_axis',(0.,0.,-1.)) ;
#33097 = DIRECTION('ref_axis',(1.,0.,0.)) ;
#33098 = DIRECTION('',(0.,-1.,0.)) ;
#33099 = DIRECTION('',(-1.,0.,0.)) ;
#33100 = DIRECTION('',(0.,1.,0.)) ;
#33101 = DIRECTION('center_axis',(0.,0.,-1.)) ;
#33102 = DIRECTION('ref_axis',(1.,0.,0.)) ;
#33103 = DIRECTION('',(0.,-1.,0.)) ;
#33104 = DIRECTION('',(0.,-1.,0.)) ;
#33105 = DIRECTION('',(-1.,0.,0.)) ;
#33106 = DIRECTION('',(0.,1.,0.)) ;
#33107 = DIRECTION('center_axis',(0.,0.,-1.)) ;
#33108 = DIRECTION('ref_axis',(1.,0.,0.)) ;
#33109 = DIRECTION('',(1.,0.,0.)) ;
#33110 = DIRECTION('',(-1.,0.,0.)) ;
#33111 = DIRECTION('center_axis',(0.,0.,-1.)) ;
#33112 = DIRECTION('ref_axis',(1.,0.,0.)) ;
#33113 = DIRECTION('',(0.,-1.,0.)) ;
#33114 = DIRECTION('center_axis',(0.,0.,-1.)) ;
#33115 = DIRECTION('ref_axis',(1.,0.,0.)) ;
#33116 = DIRECTION('',(0.,1.,0.)) ;
#33117 = DIRECTION('',(1.,0.,0.)) ;
#33118 = DIRECTION('',(0.,-1.,0.)) ;
#33119 = DIRECTION('',(0.,-1.,0.)) ;
#33120 = DIRECTION('',(-1.,0.,0.)) ;
#33121 = DIRECTION('',(0.,1.,0.)) ;
#33122 = DIRECTION('',(1.,0.,0.)) ;
#33123 = DIRECTION('',(0.,-1.,0.)) ;
#33124 = DIRECTION('',(-1.,0.,0.)) ;
#33125 = DIRECTION('',(0.,1.,0.)) ;
#33126 = DIRECTION('',(1.,0.,0.)) ;
#33127 = DIRECTION('',(0.,-1.,0.)) ;
#33128 = DIRECTION('',(-1.,0.,0.)) ;
#33129 = DIRECTION('',(0.,1.,0.)) ;
#33130 = DIRECTION('',(1.,0.,0.)) ;
#33131 = DIRECTION('',(0.,-1.,0.)) ;
#33132 = DIRECTION('',(-1.,0.,0.)) ;
#33133 = DIRECTION('',(0.,1.,0.)) ;
#33134 = DIRECTION('',(1.,0.,0.)) ;
#33135 = DIRECTION('',(0.,-1.,0.)) ;
#33136 = DIRECTION('',(-1.,0.,0.)) ;
#33137 = DIRECTION('',(0.,1.,0.)) ;
#33138 = DIRECTION('',(1.,0.,0.)) ;
#33139 = DIRECTION('',(0.,-1.,0.)) ;
#33140 = DIRECTION('',(-1.,0.,0.)) ;
#33141 = DIRECTION('center_axis',(0.,0.,-1.)) ;
#33142 = DIRECTION('ref_axis',(1.,0.,0.)) ;
#33143 = DIRECTION('',(1.,0.,0.)) ;
#33144 = DIRECTION('',(0.,-1.,0.)) ;
#33145 = DIRECTION('',(-1.,0.,0.)) ;
#33146 = DIRECTION('',(0.,1.,0.)) ;
#33147 = DIRECTION('',(1.,0.,0.)) ;
#33148 = DIRECTION('',(0.,-1.,0.)) ;
#33149 = DIRECTION('',(-1.,0.,0.)) ;
#33150 = DIRECTION('',(0.,1.,0.)) ;
#33151 = DIRECTION('',(1.,0.,0.)) ;
#33152 = DIRECTION('',(0.,-1.,0.)) ;
#33153 = DIRECTION('center_axis',(0.,0.,-1.)) ;
#33154 = DIRECTION('ref_axis',(1.,0.,0.)) ;
#33155 = DIRECTION('',(1.,0.,0.)) ;
#33156 = DIRECTION('',(0.,-1.,0.)) ;
#33157 = DIRECTION('',(-1.,0.,0.)) ;
#33158 = DIRECTION('center_axis',(0.,0.,-1.)) ;
#33159 = DIRECTION('ref_axis',(1.,0.,0.)) ;
#33160 = DIRECTION('',(0.,1.,0.)) ;
#33161 = DIRECTION('',(1.,0.,0.)) ;
#33162 = DIRECTION('',(0.,-1.,0.)) ;
#33163 = DIRECTION('center_axis',(0.,0.,-1.)) ;
#33164 = DIRECTION('ref_axis',(1.,0.,0.)) ;
#33165 = DIRECTION('',(1.,0.,0.)) ;
#33166 = DIRECTION('',(0.,-1.,0.)) ;
#33167 = DIRECTION('',(-1.,0.,0.)) ;
#33168 = DIRECTION('',(0.,1.,0.)) ;
#33169 = DIRECTION('',(1.,0.,0.)) ;
#33170 = DIRECTION('',(-1.,0.,0.)) ;
#33171 = DIRECTION('center_axis',(0.,0.,-1.)) ;
#33172 = DIRECTION('ref_axis',(1.,0.,0.)) ;
#33173 = DIRECTION('',(0.,-1.,0.)) ;
#33174 = DIRECTION('',(0.,-1.,0.)) ;
#33175 = DIRECTION('',(-1.,0.,0.)) ;
#33176 = DIRECTION('center_axis',(0.,0.,-1.)) ;
#33177 = DIRECTION('ref_axis',(1.,0.,0.)) ;
#33178 = DIRECTION('',(1.,0.,0.)) ;
#33179 = DIRECTION('',(0.,-1.,0.)) ;
#33180 = DIRECTION('',(-1.,0.,0.)) ;
#33181 = DIRECTION('',(0.,1.,0.)) ;
#33182 = DIRECTION('',(1.,0.,0.)) ;
#33183 = DIRECTION('',(0.,-1.,0.)) ;
#33184 = DIRECTION('',(-1.,0.,0.)) ;
#33185 = DIRECTION('',(0.,1.,0.)) ;
#33186 = DIRECTION('',(1.,0.,0.)) ;
#33187 = DIRECTION('',(0.,-1.,0.)) ;
#33188 = DIRECTION('',(-1.,0.,0.)) ;
#33189 = DIRECTION('',(0.,1.,0.)) ;
#33190 = DIRECTION('',(1.,0.,0.)) ;
#33191 = DIRECTION('',(0.,-1.,0.)) ;
#33192 = DIRECTION('',(-1.,0.,0.)) ;
#33193 = DIRECTION('',(0.,1.,0.)) ;
#33194 = DIRECTION('',(1.,0.,0.)) ;
#33195 = DIRECTION('',(0.,-1.,0.)) ;
#33196 = DIRECTION('',(-1.,0.,0.)) ;
#33197 = DIRECTION('',(0.,1.,0.)) ;
#33198 = DIRECTION('',(1.,0.,0.)) ;
#33199 = DIRECTION('',(0.,-1.,0.)) ;
#33200 = DIRECTION('',(-1.,0.,0.)) ;
#33201 = DIRECTION('',(0.,1.,0.)) ;
#33202 = DIRECTION('',(1.,0.,0.)) ;
#33203 = DIRECTION('',(0.,1.,0.)) ;
#33204 = DIRECTION('',(1.,0.,0.)) ;
#33205 = DIRECTION('center_axis',(0.,0.,-1.)) ;
#33206 = DIRECTION('ref_axis',(1.,0.,0.)) ;
#33207 = DIRECTION('',(0.,-1.,0.)) ;
#33208 = DIRECTION('',(-1.,0.,0.)) ;
#33209 = DIRECTION('',(0.,1.,0.)) ;
#33210 = DIRECTION('',(1.,0.,0.)) ;
#33211 = DIRECTION('center_axis',(0.,0.,-1.)) ;
#33212 = DIRECTION('ref_axis',(1.,0.,0.)) ;
#33213 = DIRECTION('',(0.,1.,0.)) ;
#33214 = DIRECTION('',(1.,0.,0.)) ;
#33215 = DIRECTION('',(0.,-1.,0.)) ;
#33216 = DIRECTION('',(1.,0.,0.)) ;
#33217 = DIRECTION('',(0.,-1.,0.)) ;
#33218 = DIRECTION('',(-1.,0.,0.)) ;
#33219 = DIRECTION('',(0.,1.,0.)) ;
#33220 = DIRECTION('',(0.,-1.,0.)) ;
#33221 = DIRECTION('',(-1.,0.,0.)) ;
#33222 = DIRECTION('',(0.,1.,0.)) ;
#33223 = DIRECTION('',(1.,0.,0.)) ;
#33224 = DIRECTION('',(0.,-1.,0.)) ;
#33225 = DIRECTION('',(-1.,0.,0.)) ;
#33226 = DIRECTION('',(0.,1.,0.)) ;
#33227 = DIRECTION('',(1.,0.,0.)) ;
#33228 = DIRECTION('',(0.,-1.,0.)) ;
#33229 = DIRECTION('',(-1.,0.,0.)) ;
#33230 = DIRECTION('',(0.,1.,0.)) ;
#33231 = DIRECTION('',(1.,0.,0.)) ;
#33232 = DIRECTION('',(0.,-1.,0.)) ;
#33233 = DIRECTION('',(-1.,0.,0.)) ;
#33234 = DIRECTION('',(0.,1.,0.)) ;
#33235 = DIRECTION('',(1.,0.,0.)) ;
#33236 = DIRECTION('',(0.,-1.,0.)) ;
#33237 = DIRECTION('',(-1.,0.,0.)) ;
#33238 = DIRECTION('',(0.,1.,0.)) ;
#33239 = DIRECTION('',(1.,0.,0.)) ;
#33240 = DIRECTION('',(0.,-1.,0.)) ;
#33241 = DIRECTION('',(-1.,0.,0.)) ;
#33242 = DIRECTION('',(0.,1.,0.)) ;
#33243 = DIRECTION('',(1.,0.,0.)) ;
#33244 = DIRECTION('',(0.,-1.,0.)) ;
#33245 = DIRECTION('',(-1.,0.,0.)) ;
#33246 = DIRECTION('',(0.,1.,0.)) ;
#33247 = DIRECTION('',(1.,0.,0.)) ;
#33248 = DIRECTION('',(0.,-1.,0.)) ;
#33249 = DIRECTION('',(-1.,0.,0.)) ;
#33250 = DIRECTION('',(0.,1.,0.)) ;
#33251 = DIRECTION('',(1.,0.,0.)) ;
#33252 = DIRECTION('center_axis',(0.,0.,-1.)) ;
#33253 = DIRECTION('ref_axis',(1.,0.,0.)) ;
#33254 = DIRECTION('',(-1.,0.,0.)) ;
#33255 = DIRECTION('',(0.,1.,0.)) ;
#33256 = DIRECTION('',(1.,0.,0.)) ;
#33257 = DIRECTION('center_axis',(0.,0.,1.)) ;
#33258 = DIRECTION('ref_axis',(1.,0.,0.)) ;
#33259 = DIRECTION('center_axis',(0.,0.,1.)) ;
#33260 = DIRECTION('ref_axis',(1.,0.,0.)) ;
#33261 = DIRECTION('',(0.,0.,1.)) ;
#33262 = DIRECTION('center_axis',(0.,0.,-1.)) ;
#33263 = DIRECTION('ref_axis',(-1.,0.,0.)) ;
#33264 = DIRECTION('',(1.,0.,0.)) ;
#33265 = DIRECTION('',(0.,-1.,0.)) ;
#33266 = DIRECTION('center_axis',(0.,0.,-1.)) ;
#33267 = DIRECTION('ref_axis',(1.,0.,0.)) ;
#33268 = DIRECTION('',(1.,0.,0.)) ;
#33269 = DIRECTION('',(0.,-1.,0.)) ;
#33270 = DIRECTION('center_axis',(0.,0.,-1.)) ;
#33271 = DIRECTION('ref_axis',(1.,0.,0.)) ;
#33272 = DIRECTION('',(1.,0.,0.)) ;
#33273 = DIRECTION('',(0.,-1.,0.)) ;
#33274 = DIRECTION('',(-1.,0.,0.)) ;
#33275 = DIRECTION('center_axis',(0.,0.,-1.)) ;
#33276 = DIRECTION('ref_axis',(1.,0.,0.)) ;
#33277 = DIRECTION('',(0.,-1.,0.)) ;
#33278 = DIRECTION('',(-1.,0.,0.)) ;
#33279 = DIRECTION('center_axis',(0.,0.,-1.)) ;
#33280 = DIRECTION('ref_axis',(1.,0.,0.)) ;
#33281 = DIRECTION('',(0.,-1.,0.)) ;
#33282 = DIRECTION('',(-1.,0.,0.)) ;
#33283 = DIRECTION('center_axis',(0.,0.,-1.)) ;
#33284 = DIRECTION('ref_axis',(1.,0.,0.)) ;
#33285 = DIRECTION('center_axis',(0.,0.,-1.)) ;
#33286 = DIRECTION('ref_axis',(1.,0.,0.)) ;
#33287 = DIRECTION('',(0.,-1.,0.)) ;
#33288 = DIRECTION('',(-1.,0.,0.)) ;
#33289 = DIRECTION('center_axis',(0.,0.,-1.)) ;
#33290 = DIRECTION('ref_axis',(1.,0.,0.)) ;
#33291 = DIRECTION('',(0.,-1.,0.)) ;
#33292 = DIRECTION('',(-1.,0.,0.)) ;
#33293 = DIRECTION('center_axis',(0.,0.,-1.)) ;
#33294 = DIRECTION('ref_axis',(1.,0.,0.)) ;
#33295 = DIRECTION('',(0.,-1.,0.)) ;
#33296 = DIRECTION('',(-1.,0.,0.)) ;
#33297 = DIRECTION('center_axis',(0.,0.,-1.)) ;
#33298 = DIRECTION('ref_axis',(1.,0.,0.)) ;
#33299 = DIRECTION('',(0.,-1.,0.)) ;
#33300 = DIRECTION('',(-1.,0.,0.)) ;
#33301 = DIRECTION('',(0.,1.,0.)) ;
#33302 = DIRECTION('center_axis',(0.,0.,-1.)) ;
#33303 = DIRECTION('ref_axis',(1.,0.,0.)) ;
#33304 = DIRECTION('',(-1.,0.,0.)) ;
#33305 = DIRECTION('',(0.,1.,0.)) ;
#33306 = DIRECTION('center_axis',(0.,0.,-1.)) ;
#33307 = DIRECTION('ref_axis',(1.,0.,0.)) ;
#33308 = DIRECTION('',(-1.,0.,0.)) ;
#33309 = DIRECTION('',(0.,1.,0.)) ;
#33310 = DIRECTION('center_axis',(0.,0.,-1.)) ;
#33311 = DIRECTION('ref_axis',(1.,0.,0.)) ;
#33312 = DIRECTION('',(-1.,0.,0.)) ;
#33313 = DIRECTION('',(0.,1.,0.)) ;
#33314 = DIRECTION('center_axis',(0.,0.,-1.)) ;
#33315 = DIRECTION('ref_axis',(1.,0.,0.)) ;
#33316 = DIRECTION('',(-1.,0.,0.)) ;
#33317 = DIRECTION('',(0.,1.,0.)) ;
#33318 = DIRECTION('center_axis',(0.,0.,-1.)) ;
#33319 = DIRECTION('ref_axis',(1.,0.,0.)) ;
#33320 = DIRECTION('',(-1.,0.,0.)) ;
#33321 = DIRECTION('',(0.,1.,0.)) ;
#33322 = DIRECTION('center_axis',(0.,0.,-1.)) ;
#33323 = DIRECTION('ref_axis',(1.,0.,0.)) ;
#33324 = DIRECTION('',(-1.,0.,0.)) ;
#33325 = DIRECTION('',(0.,1.,0.)) ;
#33326 = DIRECTION('center_axis',(0.,0.,-1.)) ;
#33327 = DIRECTION('ref_axis',(1.,0.,0.)) ;
#33328 = DIRECTION('',(-1.,0.,0.)) ;
#33329 = DIRECTION('',(0.,1.,0.)) ;
#33330 = DIRECTION('',(1.,0.,0.)) ;
#33331 = DIRECTION('center_axis',(0.,0.,-1.)) ;
#33332 = DIRECTION('ref_axis',(1.,0.,0.)) ;
#33333 = DIRECTION('',(0.,1.,0.)) ;
#33334 = DIRECTION('',(1.,0.,0.)) ;
#33335 = DIRECTION('center_axis',(0.,0.,-1.)) ;
#33336 = DIRECTION('ref_axis',(1.,0.,0.)) ;
#33337 = DIRECTION('',(0.,1.,0.)) ;
#33338 = DIRECTION('',(1.,0.,0.)) ;
#33339 = DIRECTION('center_axis',(0.,0.,-1.)) ;
#33340 = DIRECTION('ref_axis',(1.,0.,0.)) ;
#33341 = DIRECTION('',(0.,1.,0.)) ;
#33342 = DIRECTION('',(1.,0.,0.)) ;
#33343 = DIRECTION('center_axis',(0.,0.,-1.)) ;
#33344 = DIRECTION('ref_axis',(1.,0.,0.)) ;
#33345 = DIRECTION('',(0.,1.,0.)) ;
#33346 = DIRECTION('',(1.,0.,0.)) ;
#33347 = DIRECTION('center_axis',(0.,0.,-1.)) ;
#33348 = DIRECTION('ref_axis',(1.,0.,0.)) ;
#33349 = DIRECTION('',(0.,1.,0.)) ;
#33350 = DIRECTION('',(1.,0.,0.)) ;
#33351 = DIRECTION('center_axis',(0.,0.,-1.)) ;
#33352 = DIRECTION('ref_axis',(1.,0.,0.)) ;
#33353 = DIRECTION('',(0.,1.,0.)) ;
#33354 = DIRECTION('',(1.,0.,0.)) ;
#33355 = DIRECTION('center_axis',(0.,0.,-1.)) ;
#33356 = DIRECTION('ref_axis',(1.,0.,0.)) ;
#33357 = DIRECTION('',(0.,1.,0.)) ;
#33358 = DIRECTION('',(1.,0.,0.)) ;
#33359 = DIRECTION('',(0.,-1.,0.)) ;
#33360 = DIRECTION('center_axis',(0.,0.,-1.)) ;
#33361 = DIRECTION('ref_axis',(1.,0.,0.)) ;
#33362 = DIRECTION('',(1.,0.,0.)) ;
#33363 = DIRECTION('',(0.,-1.,0.)) ;
#33364 = DIRECTION('center_axis',(0.,0.,-1.)) ;
#33365 = DIRECTION('ref_axis',(1.,0.,0.)) ;
#33366 = DIRECTION('',(1.,0.,0.)) ;
#33367 = DIRECTION('',(0.,-1.,0.)) ;
#33368 = DIRECTION('center_axis',(0.,0.,-1.)) ;
#33369 = DIRECTION('ref_axis',(1.,0.,0.)) ;
#33370 = DIRECTION('',(1.,0.,0.)) ;
#33371 = DIRECTION('',(0.,-1.,0.)) ;
#33372 = DIRECTION('',(-1.,0.,0.)) ;
#33373 = DIRECTION('',(0.,-1.,0.)) ;
#33374 = DIRECTION('',(-1.,0.,0.)) ;
#33375 = DIRECTION('',(0.,-1.,0.)) ;
#33376 = DIRECTION('',(-1.,0.,0.)) ;
#33377 = DIRECTION('',(0.,-1.,0.)) ;
#33378 = DIRECTION('',(-1.,0.,0.)) ;
#33379 = DIRECTION('',(0.,-1.,0.)) ;
#33380 = DIRECTION('center_axis',(0.,0.,1.)) ;
#33381 = DIRECTION('ref_axis',(1.,0.,0.)) ;
#33382 = DIRECTION('',(-1.,0.,0.)) ;
#33383 = DIRECTION('',(0.,-1.,0.)) ;
#33384 = DIRECTION('',(1.,0.,0.)) ;
#33385 = DIRECTION('center_axis',(0.,0.,1.)) ;
#33386 = DIRECTION('ref_axis',(1.,0.,0.)) ;
#33387 = DIRECTION('',(1.,0.,0.)) ;
#33388 = DIRECTION('center_axis',(0.,0.,1.)) ;
#33389 = DIRECTION('ref_axis',(1.,0.,0.)) ;
#33390 = DIRECTION('center_axis',(0.,0.,1.)) ;
#33391 = DIRECTION('ref_axis',(1.,0.,0.)) ;
#33392 = DIRECTION('',(-1.,0.,0.)) ;
#33393 = DIRECTION('',(0.,-1.,0.)) ;
#33394 = DIRECTION('',(1.,0.,0.)) ;
#33395 = DIRECTION('',(1.,0.,0.)) ;
#33396 = DIRECTION('',(-1.,0.,0.)) ;
#33397 = DIRECTION('center_axis',(0.,0.,1.)) ;
#33398 = DIRECTION('ref_axis',(1.,0.,0.)) ;
#33399 = DIRECTION('',(0.,-1.,0.)) ;
#33400 = DIRECTION('',(1.,0.,0.)) ;
#33401 = DIRECTION('',(0.,1.,0.)) ;
#33402 = DIRECTION('',(0.,-1.,0.)) ;
#33403 = DIRECTION('',(1.,0.,0.)) ;
#33404 = DIRECTION('',(0.,1.,0.)) ;
#33405 = DIRECTION('',(-1.,0.,0.)) ;
#33406 = DIRECTION('',(-1.,0.,0.)) ;
#33407 = DIRECTION('',(0.,-1.,0.)) ;
#33408 = DIRECTION('',(1.,0.,0.)) ;
#33409 = DIRECTION('',(0.,1.,0.)) ;
#33410 = DIRECTION('',(-1.,0.,0.)) ;
#33411 = DIRECTION('',(0.,-1.,0.)) ;
#33412 = DIRECTION('',(1.,0.,0.)) ;
#33413 = DIRECTION('',(0.,1.,0.)) ;
#33414 = DIRECTION('',(-1.,0.,0.)) ;
#33415 = DIRECTION('',(0.,-1.,0.)) ;
#33416 = DIRECTION('',(1.,0.,0.)) ;
#33417 = DIRECTION('',(0.,1.,0.)) ;
#33418 = DIRECTION('',(0.,1.,0.)) ;
#33419 = DIRECTION('center_axis',(0.,0.,1.)) ;
#33420 = DIRECTION('ref_axis',(1.,0.,0.)) ;
#33421 = DIRECTION('',(1.,0.,0.)) ;
#33422 = DIRECTION('',(-1.,0.,0.)) ;
#33423 = DIRECTION('',(0.,-1.,0.)) ;
#33424 = DIRECTION('',(1.,0.,0.)) ;
#33425 = DIRECTION('',(0.,1.,0.)) ;
#33426 = DIRECTION('',(-1.,0.,0.)) ;
#33427 = DIRECTION('',(0.,-1.,0.)) ;
#33428 = DIRECTION('',(1.,0.,0.)) ;
#33429 = DIRECTION('',(0.,1.,0.)) ;
#33430 = DIRECTION('',(-1.,0.,0.)) ;
#33431 = DIRECTION('',(0.,-1.,0.)) ;
#33432 = DIRECTION('',(1.,0.,0.)) ;
#33433 = DIRECTION('',(0.,1.,0.)) ;
#33434 = DIRECTION('',(-1.,0.,0.)) ;
#33435 = DIRECTION('',(0.,-1.,0.)) ;
#33436 = DIRECTION('',(1.,0.,0.)) ;
#33437 = DIRECTION('',(0.,1.,0.)) ;
#33438 = DIRECTION('',(-1.,0.,0.)) ;
#33439 = DIRECTION('',(0.,-1.,0.)) ;
#33440 = DIRECTION('',(1.,0.,0.)) ;
#33441 = DIRECTION('',(0.,1.,0.)) ;
#33442 = DIRECTION('',(-1.,0.,0.)) ;
#33443 = DIRECTION('',(0.,-1.,0.)) ;
#33444 = DIRECTION('',(1.,0.,0.)) ;
#33445 = DIRECTION('',(0.,1.,0.)) ;
#33446 = DIRECTION('',(0.,1.,0.)) ;
#33447 = DIRECTION('',(-1.,0.,0.)) ;
#33448 = DIRECTION('',(0.,-1.,0.)) ;
#33449 = DIRECTION('center_axis',(0.,0.,1.)) ;
#33450 = DIRECTION('ref_axis',(1.,0.,0.)) ;
#33451 = DIRECTION('',(-1.,0.,0.)) ;
#33452 = DIRECTION('center_axis',(0.,0.,1.)) ;
#33453 = DIRECTION('ref_axis',(1.,0.,0.)) ;
#33454 = DIRECTION('',(1.,0.,0.)) ;
#33455 = DIRECTION('',(0.,1.,0.)) ;
#33456 = DIRECTION('',(-1.,0.,0.)) ;
#33457 = DIRECTION('',(0.,-1.,0.)) ;
#33458 = DIRECTION('center_axis',(0.,0.,1.)) ;
#33459 = DIRECTION('ref_axis',(1.,0.,0.)) ;
#33460 = DIRECTION('',(1.,0.,0.)) ;
#33461 = DIRECTION('',(0.,1.,0.)) ;
#33462 = DIRECTION('',(-1.,0.,0.)) ;
#33463 = DIRECTION('center_axis',(0.,0.,1.)) ;
#33464 = DIRECTION('ref_axis',(1.,0.,0.)) ;
#33465 = DIRECTION('',(0.,1.,0.)) ;
#33466 = DIRECTION('',(-1.,0.,0.)) ;
#33467 = DIRECTION('',(0.,-1.,0.)) ;
#33468 = DIRECTION('',(1.,0.,0.)) ;
#33469 = DIRECTION('',(0.,1.,0.)) ;
#33470 = DIRECTION('',(-1.,0.,0.)) ;
#33471 = DIRECTION('center_axis',(0.,0.,1.)) ;
#33472 = DIRECTION('ref_axis',(1.,0.,0.)) ;
#33473 = DIRECTION('',(0.,1.,0.)) ;
#33474 = DIRECTION('',(-1.,0.,0.)) ;
#33475 = DIRECTION('',(0.,-1.,0.)) ;
#33476 = DIRECTION('',(1.,0.,0.)) ;
#33477 = DIRECTION('',(0.,1.,0.)) ;
#33478 = DIRECTION('',(-1.,0.,0.)) ;
#33479 = DIRECTION('',(0.,-1.,0.)) ;
#33480 = DIRECTION('',(1.,0.,0.)) ;
#33481 = DIRECTION('',(0.,1.,0.)) ;
#33482 = DIRECTION('',(-1.,0.,0.)) ;
#33483 = DIRECTION('',(0.,-1.,0.)) ;
#33484 = DIRECTION('',(1.,0.,0.)) ;
#33485 = DIRECTION('',(0.,1.,0.)) ;
#33486 = DIRECTION('',(-1.,0.,0.)) ;
#33487 = DIRECTION('',(0.,-1.,0.)) ;
#33488 = DIRECTION('',(1.,0.,0.)) ;
#33489 = DIRECTION('',(0.,1.,0.)) ;
#33490 = DIRECTION('',(-1.,0.,0.)) ;
#33491 = DIRECTION('center_axis',(0.,0.,1.)) ;
#33492 = DIRECTION('ref_axis',(1.,0.,0.)) ;
#33493 = DIRECTION('',(1.,0.,0.)) ;
#33494 = DIRECTION('',(0.,1.,0.)) ;
#33495 = DIRECTION('',(0.,1.,0.)) ;
#33496 = DIRECTION('',(-1.,0.,0.)) ;
#33497 = DIRECTION('',(0.,-1.,0.)) ;
#33498 = DIRECTION('center_axis',(0.,0.,1.)) ;
#33499 = DIRECTION('ref_axis',(1.,0.,0.)) ;
#33500 = DIRECTION('',(-1.,0.,0.)) ;
#33501 = DIRECTION('',(0.,-1.,0.)) ;
#33502 = DIRECTION('',(1.,0.,0.)) ;
#33503 = DIRECTION('',(0.,1.,0.)) ;
#33504 = DIRECTION('',(-1.,0.,0.)) ;
#33505 = DIRECTION('',(0.,-1.,0.)) ;
#33506 = DIRECTION('',(1.,0.,0.)) ;
#33507 = DIRECTION('',(0.,1.,0.)) ;
#33508 = DIRECTION('',(-1.,0.,0.)) ;
#33509 = DIRECTION('',(0.,-1.,0.)) ;
#33510 = DIRECTION('',(1.,0.,0.)) ;
#33511 = DIRECTION('',(0.,1.,0.)) ;
#33512 = DIRECTION('center_axis',(0.,0.,1.)) ;
#33513 = DIRECTION('ref_axis',(1.,0.,0.)) ;
#33514 = DIRECTION('',(-1.,0.,0.)) ;
#33515 = DIRECTION('',(0.,-1.,0.)) ;
#33516 = DIRECTION('',(-1.,0.,0.)) ;
#33517 = DIRECTION('',(0.,-1.,0.)) ;
#33518 = DIRECTION('',(1.,0.,0.)) ;
#33519 = DIRECTION('',(0.,1.,0.)) ;
#33520 = DIRECTION('',(-1.,0.,0.)) ;
#33521 = DIRECTION('',(0.,-1.,0.)) ;
#33522 = DIRECTION('',(1.,0.,0.)) ;
#33523 = DIRECTION('',(0.,1.,0.)) ;
#33524 = DIRECTION('',(-1.,0.,0.)) ;
#33525 = DIRECTION('',(0.,-1.,0.)) ;
#33526 = DIRECTION('',(1.,0.,0.)) ;
#33527 = DIRECTION('',(0.,1.,0.)) ;
#33528 = DIRECTION('',(-1.,0.,0.)) ;
#33529 = DIRECTION('',(0.,-1.,0.)) ;
#33530 = DIRECTION('',(1.,0.,0.)) ;
#33531 = DIRECTION('',(0.,1.,0.)) ;
#33532 = DIRECTION('',(-1.,0.,0.)) ;
#33533 = DIRECTION('',(0.,-1.,0.)) ;
#33534 = DIRECTION('',(1.,0.,0.)) ;
#33535 = DIRECTION('',(0.,1.,0.)) ;
#33536 = DIRECTION('',(-1.,0.,0.)) ;
#33537 = DIRECTION('',(0.,-1.,0.)) ;
#33538 = DIRECTION('',(1.,0.,0.)) ;
#33539 = DIRECTION('',(0.,1.,0.)) ;
#33540 = DIRECTION('',(-1.,0.,0.)) ;
#33541 = DIRECTION('',(0.,-1.,0.)) ;
#33542 = DIRECTION('',(1.,0.,0.)) ;
#33543 = DIRECTION('',(0.,1.,0.)) ;
#33544 = DIRECTION('',(-1.,0.,0.)) ;
#33545 = DIRECTION('',(0.,-1.,0.)) ;
#33546 = DIRECTION('',(1.,0.,0.)) ;
#33547 = DIRECTION('',(0.,1.,0.)) ;
#33548 = DIRECTION('',(-1.,0.,0.)) ;
#33549 = DIRECTION('',(0.,-1.,0.)) ;
#33550 = DIRECTION('',(1.,0.,0.)) ;
#33551 = DIRECTION('',(0.,1.,0.)) ;
#33552 = DIRECTION('',(1.,0.,0.)) ;
#33553 = DIRECTION('center_axis',(0.,0.,1.)) ;
#33554 = DIRECTION('ref_axis',(1.,0.,0.)) ;
#33555 = DIRECTION('',(0.,-1.,0.)) ;
#33556 = DIRECTION('',(0.,1.,0.)) ;
#33557 = DIRECTION('center_axis',(0.,0.,1.)) ;
#33558 = DIRECTION('ref_axis',(1.,0.,0.)) ;
#33559 = DIRECTION('',(1.,0.,0.)) ;
#33560 = DIRECTION('',(0.,1.,0.)) ;
#33561 = DIRECTION('center_axis',(0.,0.,1.)) ;
#33562 = DIRECTION('ref_axis',(1.,0.,0.)) ;
#33563 = DIRECTION('',(0.,-1.,0.)) ;
#33564 = DIRECTION('',(1.,0.,0.)) ;
#33565 = DIRECTION('',(0.,1.,0.)) ;
#33566 = DIRECTION('center_axis',(0.,0.,1.)) ;
#33567 = DIRECTION('ref_axis',(1.,0.,0.)) ;
#33568 = DIRECTION('',(0.,-1.,0.)) ;
#33569 = DIRECTION('',(1.,0.,0.)) ;
#33570 = DIRECTION('',(0.,-1.,0.)) ;
#33571 = DIRECTION('',(1.,0.,0.)) ;
#33572 = DIRECTION('',(0.,1.,0.)) ;
#33573 = DIRECTION('',(-1.,0.,0.)) ;
#33574 = DIRECTION('center_axis',(0.,0.,1.)) ;
#33575 = DIRECTION('ref_axis',(1.,0.,0.)) ;
#33576 = DIRECTION('',(0.,0.,-1.)) ;
#33577 = DIRECTION('center_axis',(0.,0.,1.)) ;
#33578 = DIRECTION('ref_axis',(1.,0.,0.)) ;
#33579 = DIRECTION('',(0.,0.,1.)) ;
#33580 = DIRECTION('center_axis',(-1.,0.,0.)) ;
#33581 = DIRECTION('ref_axis',(0.,0.,1.)) ;
#33582 = DIRECTION('',(0.,0.,-1.)) ;
#33583 = DIRECTION('center_axis',(0.,1.,0.)) ;
#33584 = DIRECTION('ref_axis',(0.,0.,1.)) ;
#33585 = DIRECTION('',(0.,0.,-1.)) ;
#33586 = DIRECTION('',(0.,0.,1.)) ;
#33587 = DIRECTION('center_axis',(0.,1.,0.)) ;
#33588 = DIRECTION('ref_axis',(0.,0.,1.)) ;
#33589 = DIRECTION('',(0.,0.,-1.)) ;
#33590 = DIRECTION('',(0.,0.,1.)) ;
#33591 = DIRECTION('center_axis',(0.,1.,0.)) ;
#33592 = DIRECTION('ref_axis',(0.,0.,1.)) ;
#33593 = DIRECTION('',(0.,0.,-1.)) ;
#33594 = DIRECTION('',(0.,0.,1.)) ;
#33595 = DIRECTION('center_axis',(0.,1.,0.)) ;
#33596 = DIRECTION('ref_axis',(0.,0.,1.)) ;
#33597 = DIRECTION('',(0.,0.,1.)) ;
#33598 = DIRECTION('',(0.,0.,-1.)) ;
#33599 = DIRECTION('center_axis',(0.,1.,0.)) ;
#33600 = DIRECTION('ref_axis',(0.,0.,1.)) ;
#33601 = DIRECTION('',(0.,0.,1.)) ;
#33602 = DIRECTION('',(0.,0.,-1.)) ;
#33603 = DIRECTION('center_axis',(0.,1.,0.)) ;
#33604 = DIRECTION('ref_axis',(0.,0.,1.)) ;
#33605 = DIRECTION('',(0.,0.,-1.)) ;
#33606 = DIRECTION('',(0.,0.,1.)) ;
#33607 = DIRECTION('center_axis',(0.,-1.,0.)) ;
#33608 = DIRECTION('ref_axis',(0.,0.,-1.)) ;
#33609 = DIRECTION('',(0.,0.,1.)) ;
#33610 = DIRECTION('',(0.,0.,-1.)) ;
#33611 = DIRECTION('center_axis',(0.,-1.,0.)) ;
#33612 = DIRECTION('ref_axis',(0.,0.,-1.)) ;
#33613 = DIRECTION('',(0.,0.,1.)) ;
#33614 = DIRECTION('',(0.,0.,-1.)) ;
#33615 = DIRECTION('center_axis',(0.,-1.,0.)) ;
#33616 = DIRECTION('ref_axis',(0.,0.,-1.)) ;
#33617 = DIRECTION('',(0.,0.,1.)) ;
#33618 = DIRECTION('',(0.,0.,-1.)) ;
#33619 = DIRECTION('center_axis',(0.,-1.,0.)) ;
#33620 = DIRECTION('ref_axis',(0.,0.,-1.)) ;
#33621 = DIRECTION('',(0.,0.,1.)) ;
#33622 = DIRECTION('',(0.,0.,-1.)) ;
#33623 = DIRECTION('center_axis',(0.,-1.,0.)) ;
#33624 = DIRECTION('ref_axis',(0.,0.,-1.)) ;
#33625 = DIRECTION('',(0.,0.,-1.)) ;
#33626 = DIRECTION('center_axis',(1.,0.,0.)) ;
#33627 = DIRECTION('ref_axis',(0.,0.,-1.)) ;
#33628 = DIRECTION('',(0.,0.,-1.)) ;
#33629 = DIRECTION('center_axis',(0.,-1.,0.)) ;
#33630 = DIRECTION('ref_axis',(0.,0.,-1.)) ;
#33631 = DIRECTION('',(0.,0.,-1.)) ;
#33632 = DIRECTION('',(0.,0.,1.)) ;
#33633 = DIRECTION('center_axis',(-1.,0.,0.)) ;
#33634 = DIRECTION('ref_axis',(0.,0.,1.)) ;
#33635 = DIRECTION('',(0.,0.,-1.)) ;
#33636 = DIRECTION('center_axis',(1.,0.,0.)) ;
#33637 = DIRECTION('ref_axis',(0.,0.,-1.)) ;
#33638 = DIRECTION('',(0.,0.,1.)) ;
#33639 = DIRECTION('center_axis',(1.,0.,0.)) ;
#33640 = DIRECTION('ref_axis',(0.,0.,-1.)) ;
#33641 = DIRECTION('',(0.,0.,-1.)) ;
#33642 = DIRECTION('center_axis',(0.,0.,1.)) ;
#33643 = DIRECTION('ref_axis',(1.,0.,0.)) ;
#33644 = DIRECTION('center_axis',(0.,0.,1.)) ;
#33645 = DIRECTION('ref_axis',(1.,0.,0.)) ;
#33646 = DIRECTION('',(0.,0.,1.)) ;
#33647 = DIRECTION('center_axis',(-1.,0.,0.)) ;
#33648 = DIRECTION('ref_axis',(0.,0.,1.)) ;
#33649 = DIRECTION('',(0.,0.,-1.)) ;
#33650 = DIRECTION('center_axis',(1.,0.,0.)) ;
#33651 = DIRECTION('ref_axis',(0.,0.,-1.)) ;
#33652 = DIRECTION('',(0.,0.,1.)) ;
#33653 = DIRECTION('center_axis',(-1.,0.,0.)) ;
#33654 = DIRECTION('ref_axis',(0.,0.,1.)) ;
#33655 = DIRECTION('',(0.,0.,-1.)) ;
#33656 = DIRECTION('center_axis',(1.,0.,0.)) ;
#33657 = DIRECTION('ref_axis',(0.,0.,-1.)) ;
#33658 = DIRECTION('',(0.,0.,1.)) ;
#33659 = DIRECTION('center_axis',(1.,0.,0.)) ;
#33660 = DIRECTION('ref_axis',(0.,0.,-1.)) ;
#33661 = DIRECTION('',(0.,0.,1.)) ;
#33662 = DIRECTION('center_axis',(0.,0.,1.)) ;
#33663 = DIRECTION('ref_axis',(1.,0.,0.)) ;
#33664 = DIRECTION('',(0.,0.,1.)) ;
#33665 = DIRECTION('center_axis',(0.,0.,1.)) ;
#33666 = DIRECTION('ref_axis',(1.,0.,0.)) ;
#33667 = DIRECTION('',(0.,0.,-1.)) ;
#33668 = DIRECTION('center_axis',(0.,0.,1.)) ;
#33669 = DIRECTION('ref_axis',(1.,0.,0.)) ;
#33670 = DIRECTION('',(0.,0.,1.)) ;
#33671 = DIRECTION('center_axis',(0.,1.,0.)) ;
#33672 = DIRECTION('ref_axis',(0.,0.,1.)) ;
#33673 = DIRECTION('',(0.,0.,1.)) ;
#33674 = DIRECTION('',(0.,0.,-1.)) ;
#33675 = DIRECTION('center_axis',(-1.,0.,0.)) ;
#33676 = DIRECTION('ref_axis',(0.,0.,1.)) ;
#33677 = DIRECTION('',(0.,0.,-1.)) ;
#33678 = DIRECTION('center_axis',(-1.,0.,0.)) ;
#33679 = DIRECTION('ref_axis',(0.,0.,1.)) ;
#33680 = DIRECTION('',(0.,0.,-1.)) ;
#33681 = DIRECTION('center_axis',(-1.,0.,0.)) ;
#33682 = DIRECTION('ref_axis',(0.,0.,1.)) ;
#33683 = DIRECTION('',(0.,0.,-1.)) ;
#33684 = DIRECTION('',(0.,0.,1.)) ;
#33685 = DIRECTION('center_axis',(-1.,0.,0.)) ;
#33686 = DIRECTION('ref_axis',(0.,0.,1.)) ;
#33687 = DIRECTION('',(0.,0.,-1.)) ;
#33688 = DIRECTION('center_axis',(-1.,0.,0.)) ;
#33689 = DIRECTION('ref_axis',(0.,0.,1.)) ;
#33690 = DIRECTION('',(0.,0.,-1.)) ;
#33691 = DIRECTION('center_axis',(-1.,0.,0.)) ;
#33692 = DIRECTION('ref_axis',(0.,0.,1.)) ;
#33693 = DIRECTION('',(0.,0.,-1.)) ;
#33694 = DIRECTION('center_axis',(-1.,0.,0.)) ;
#33695 = DIRECTION('ref_axis',(0.,0.,1.)) ;
#33696 = DIRECTION('center_axis',(1.,0.,0.)) ;
#33697 = DIRECTION('ref_axis',(0.,0.,-1.)) ;
#33698 = DIRECTION('',(0.,0.,1.)) ;
#33699 = DIRECTION('',(0.,0.,-1.)) ;
#33700 = DIRECTION('center_axis',(1.,0.,0.)) ;
#33701 = DIRECTION('ref_axis',(0.,0.,-1.)) ;
#33702 = DIRECTION('',(0.,0.,1.)) ;
#33703 = DIRECTION('',(0.,0.,-1.)) ;
#33704 = DIRECTION('center_axis',(1.,0.,0.)) ;
#33705 = DIRECTION('ref_axis',(0.,0.,-1.)) ;
#33706 = DIRECTION('',(0.,0.,1.)) ;
#33707 = DIRECTION('',(0.,0.,-1.)) ;
#33708 = DIRECTION('center_axis',(1.,0.,0.)) ;
#33709 = DIRECTION('ref_axis',(0.,0.,-1.)) ;
#33710 = DIRECTION('',(0.,0.,1.)) ;
#33711 = DIRECTION('',(0.,0.,-1.)) ;
#33712 = DIRECTION('center_axis',(1.,0.,0.)) ;
#33713 = DIRECTION('ref_axis',(0.,0.,-1.)) ;
#33714 = DIRECTION('',(0.,0.,1.)) ;
#33715 = DIRECTION('',(0.,0.,-1.)) ;
#33716 = DIRECTION('center_axis',(0.,-1.,0.)) ;
#33717 = DIRECTION('ref_axis',(0.,0.,-1.)) ;
#33718 = DIRECTION('',(0.,0.,-1.)) ;
#33719 = DIRECTION('center_axis',(-1.,0.,0.)) ;
#33720 = DIRECTION('ref_axis',(0.,0.,1.)) ;
#33721 = DIRECTION('',(0.,0.,-1.)) ;
#33722 = DIRECTION('center_axis',(0.,1.,0.)) ;
#33723 = DIRECTION('ref_axis',(0.,0.,1.)) ;
#33724 = DIRECTION('center_axis',(0.,-1.,0.)) ;
#33725 = DIRECTION('ref_axis',(0.,0.,-1.)) ;
#33726 = DIRECTION('',(0.,0.,-1.)) ;
#33727 = DIRECTION('center_axis',(0.,0.,1.)) ;
#33728 = DIRECTION('ref_axis',(1.,0.,0.)) ;
#33729 = DIRECTION('',(0.,0.,1.)) ;
#33730 = DIRECTION('center_axis',(0.,1.,0.)) ;
#33731 = DIRECTION('ref_axis',(0.,0.,1.)) ;
#33732 = DIRECTION('center_axis',(0.,-1.,0.)) ;
#33733 = DIRECTION('ref_axis',(0.,0.,-1.)) ;
#33734 = DIRECTION('',(0.,0.,1.)) ;
#33735 = DIRECTION('center_axis',(0.,1.,0.)) ;
#33736 = DIRECTION('ref_axis',(0.,0.,1.)) ;
#33737 = DIRECTION('center_axis',(0.,-1.,0.)) ;
#33738 = DIRECTION('ref_axis',(0.,0.,-1.)) ;
#33739 = DIRECTION('',(0.,0.,1.)) ;
#33740 = DIRECTION('center_axis',(0.,1.,0.)) ;
#33741 = DIRECTION('ref_axis',(0.,0.,1.)) ;
#33742 = DIRECTION('center_axis',(0.,-1.,0.)) ;
#33743 = DIRECTION('ref_axis',(0.,0.,-1.)) ;
#33744 = DIRECTION('',(0.,0.,1.)) ;
#33745 = DIRECTION('center_axis',(0.,1.,0.)) ;
#33746 = DIRECTION('ref_axis',(0.,0.,1.)) ;
#33747 = DIRECTION('center_axis',(0.,-1.,0.)) ;
#33748 = DIRECTION('ref_axis',(0.,0.,-1.)) ;
#33749 = DIRECTION('',(0.,0.,1.)) ;
#33750 = DIRECTION('center_axis',(0.,0.,1.)) ;
#33751 = DIRECTION('ref_axis',(1.,0.,0.)) ;
#33752 = DIRECTION('',(0.,0.,1.)) ;
#33753 = DIRECTION('center_axis',(0.,-1.,0.)) ;
#33754 = DIRECTION('ref_axis',(0.,0.,-1.)) ;
#33755 = DIRECTION('',(0.,0.,1.)) ;
#33756 = DIRECTION('center_axis',(-1.,0.,0.)) ;
#33757 = DIRECTION('ref_axis',(0.,0.,1.)) ;
#33758 = DIRECTION('',(0.,0.,1.)) ;
#33759 = DIRECTION('',(0.,0.,-1.)) ;
#33760 = DIRECTION('center_axis',(0.,-1.,0.)) ;
#33761 = DIRECTION('ref_axis',(0.,0.,-1.)) ;
#33762 = DIRECTION('',(0.,0.,1.)) ;
#33763 = DIRECTION('',(0.,0.,-1.)) ;
#33764 = DIRECTION('center_axis',(0.,-1.,0.)) ;
#33765 = DIRECTION('ref_axis',(0.,0.,-1.)) ;
#33766 = DIRECTION('',(0.,0.,-1.)) ;
#33767 = DIRECTION('center_axis',(0.,-1.,0.)) ;
#33768 = DIRECTION('ref_axis',(0.,0.,-1.)) ;
#33769 = DIRECTION('',(0.,0.,-1.)) ;
#33770 = DIRECTION('center_axis',(0.,-1.,0.)) ;
#33771 = DIRECTION('ref_axis',(0.,0.,-1.)) ;
#33772 = DIRECTION('',(0.,0.,-1.)) ;
#33773 = DIRECTION('center_axis',(0.,-1.,0.)) ;
#33774 = DIRECTION('ref_axis',(0.,0.,-1.)) ;
#33775 = DIRECTION('center_axis',(0.,-1.,0.)) ;
#33776 = DIRECTION('ref_axis',(0.,0.,-1.)) ;
#33777 = DIRECTION('',(0.,0.,-1.)) ;
#33778 = DIRECTION('center_axis',(0.,1.,0.)) ;
#33779 = DIRECTION('ref_axis',(0.,0.,1.)) ;
#33780 = DIRECTION('',(0.,0.,1.)) ;
#33781 = DIRECTION('',(0.,0.,-1.)) ;
#33782 = DIRECTION('center_axis',(0.,1.,0.)) ;
#33783 = DIRECTION('ref_axis',(0.,0.,1.)) ;
#33784 = DIRECTION('',(0.,0.,-1.)) ;
#33785 = DIRECTION('',(0.,0.,1.)) ;
#33786 = DIRECTION('center_axis',(0.,1.,0.)) ;
#33787 = DIRECTION('ref_axis',(0.,0.,1.)) ;
#33788 = DIRECTION('',(0.,0.,1.)) ;
#33789 = DIRECTION('center_axis',(0.,1.,0.)) ;
#33790 = DIRECTION('ref_axis',(0.,0.,1.)) ;
#33791 = DIRECTION('',(0.,0.,-1.)) ;
#33792 = DIRECTION('',(0.,0.,1.)) ;
#33793 = DIRECTION('center_axis',(0.,1.,0.)) ;
#33794 = DIRECTION('ref_axis',(0.,0.,1.)) ;
#33795 = DIRECTION('',(0.,0.,-1.)) ;
#33796 = DIRECTION('',(0.,0.,1.)) ;
#33797 = DIRECTION('center_axis',(1.,0.,0.)) ;
#33798 = DIRECTION('ref_axis',(0.,0.,-1.)) ;
#33799 = DIRECTION('',(0.,0.,-1.)) ;
#33800 = DIRECTION('center_axis',(-1.,0.,0.)) ;
#33801 = DIRECTION('ref_axis',(0.,0.,1.)) ;
#33802 = DIRECTION('center_axis',(1.,0.,0.)) ;
#33803 = DIRECTION('ref_axis',(0.,0.,-1.)) ;
#33804 = DIRECTION('',(0.,0.,1.)) ;
#33805 = DIRECTION('center_axis',(1.,0.,0.)) ;
#33806 = DIRECTION('ref_axis',(0.,0.,-1.)) ;
#33807 = DIRECTION('',(0.,0.,-1.)) ;
#33808 = DIRECTION('center_axis',(-1.,0.,0.)) ;
#33809 = DIRECTION('ref_axis',(0.,0.,1.)) ;
#33810 = DIRECTION('center_axis',(1.,0.,0.)) ;
#33811 = DIRECTION('ref_axis',(0.,0.,-1.)) ;
#33812 = DIRECTION('',(0.,0.,1.)) ;
#33813 = DIRECTION('center_axis',(0.,0.,1.)) ;
#33814 = DIRECTION('ref_axis',(1.,0.,0.)) ;
#33815 = DIRECTION('center_axis',(0.,0.,1.)) ;
#33816 = DIRECTION('ref_axis',(1.,0.,0.)) ;
#33817 = DIRECTION('',(0.,0.,-1.)) ;
#33818 = DIRECTION('center_axis',(-1.,0.,0.)) ;
#33819 = DIRECTION('ref_axis',(0.,0.,1.)) ;
#33820 = DIRECTION('',(0.,0.,-1.)) ;
#33821 = DIRECTION('center_axis',(0.,0.,1.)) ;
#33822 = DIRECTION('ref_axis',(1.,0.,0.)) ;
#33823 = DIRECTION('',(0.,0.,-1.)) ;
#33824 = DIRECTION('center_axis',(0.,0.,1.)) ;
#33825 = DIRECTION('ref_axis',(1.,0.,0.)) ;
#33826 = DIRECTION('',(0.,0.,1.)) ;
#33827 = DIRECTION('center_axis',(-1.,0.,0.)) ;
#33828 = DIRECTION('ref_axis',(0.,0.,1.)) ;
#33829 = DIRECTION('center_axis',(1.,0.,0.)) ;
#33830 = DIRECTION('ref_axis',(0.,0.,-1.)) ;
#33831 = DIRECTION('',(0.,0.,1.)) ;
#33832 = DIRECTION('center_axis',(-1.,0.,0.)) ;
#33833 = DIRECTION('ref_axis',(0.,0.,1.)) ;
#33834 = DIRECTION('center_axis',(1.,0.,0.)) ;
#33835 = DIRECTION('ref_axis',(0.,0.,-1.)) ;
#33836 = DIRECTION('',(0.,0.,1.)) ;
#33837 = DIRECTION('center_axis',(0.,1.,0.)) ;
#33838 = DIRECTION('ref_axis',(0.,0.,1.)) ;
#33839 = DIRECTION('',(0.,0.,1.)) ;
#33840 = DIRECTION('',(0.,0.,-1.)) ;
#33841 = DIRECTION('center_axis',(-1.,0.,0.)) ;
#33842 = DIRECTION('ref_axis',(0.,0.,1.)) ;
#33843 = DIRECTION('',(0.,0.,-1.)) ;
#33844 = DIRECTION('center_axis',(-1.,0.,0.)) ;
#33845 = DIRECTION('ref_axis',(0.,0.,1.)) ;
#33846 = DIRECTION('',(0.,0.,1.)) ;
#33847 = DIRECTION('',(0.,0.,-1.)) ;
#33848 = DIRECTION('center_axis',(-1.,0.,0.)) ;
#33849 = DIRECTION('ref_axis',(0.,0.,1.)) ;
#33850 = DIRECTION('',(0.,0.,-1.)) ;
#33851 = DIRECTION('center_axis',(-1.,0.,0.)) ;
#33852 = DIRECTION('ref_axis',(0.,0.,1.)) ;
#33853 = DIRECTION('',(0.,0.,-1.)) ;
#33854 = DIRECTION('center_axis',(-1.,0.,0.)) ;
#33855 = DIRECTION('ref_axis',(0.,0.,1.)) ;
#33856 = DIRECTION('',(0.,0.,-1.)) ;
#33857 = DIRECTION('center_axis',(-1.,0.,0.)) ;
#33858 = DIRECTION('ref_axis',(0.,0.,1.)) ;
#33859 = DIRECTION('',(0.,0.,-1.)) ;
#33860 = DIRECTION('center_axis',(-1.,0.,0.)) ;
#33861 = DIRECTION('ref_axis',(0.,0.,1.)) ;
#33862 = DIRECTION('center_axis',(1.,0.,0.)) ;
#33863 = DIRECTION('ref_axis',(0.,0.,-1.)) ;
#33864 = DIRECTION('',(0.,0.,1.)) ;
#33865 = DIRECTION('',(0.,0.,-1.)) ;
#33866 = DIRECTION('center_axis',(1.,0.,0.)) ;
#33867 = DIRECTION('ref_axis',(0.,0.,-1.)) ;
#33868 = DIRECTION('',(0.,0.,1.)) ;
#33869 = DIRECTION('',(0.,0.,-1.)) ;
#33870 = DIRECTION('center_axis',(1.,0.,0.)) ;
#33871 = DIRECTION('ref_axis',(0.,0.,-1.)) ;
#33872 = DIRECTION('',(0.,0.,1.)) ;
#33873 = DIRECTION('',(0.,0.,-1.)) ;
#33874 = DIRECTION('center_axis',(1.,0.,0.)) ;
#33875 = DIRECTION('ref_axis',(0.,0.,-1.)) ;
#33876 = DIRECTION('',(0.,0.,1.)) ;
#33877 = DIRECTION('',(0.,0.,-1.)) ;
#33878 = DIRECTION('center_axis',(1.,0.,0.)) ;
#33879 = DIRECTION('ref_axis',(0.,0.,-1.)) ;
#33880 = DIRECTION('',(0.,0.,-1.)) ;
#33881 = DIRECTION('',(0.,0.,1.)) ;
#33882 = DIRECTION('center_axis',(0.,-1.,0.)) ;
#33883 = DIRECTION('ref_axis',(0.,0.,-1.)) ;
#33884 = DIRECTION('',(0.,0.,-1.)) ;
#33885 = DIRECTION('center_axis',(-1.,0.,0.)) ;
#33886 = DIRECTION('ref_axis',(0.,0.,1.)) ;
#33887 = DIRECTION('',(0.,0.,-1.)) ;
#33888 = DIRECTION('center_axis',(0.,1.,0.)) ;
#33889 = DIRECTION('ref_axis',(0.,0.,1.)) ;
#33890 = DIRECTION('center_axis',(0.,-1.,0.)) ;
#33891 = DIRECTION('ref_axis',(0.,0.,-1.)) ;
#33892 = DIRECTION('center_axis',(0.,-1.,0.)) ;
#33893 = DIRECTION('ref_axis',(0.,0.,-1.)) ;
#33894 = DIRECTION('',(0.,0.,-1.)) ;
#33895 = DIRECTION('center_axis',(0.,0.,1.)) ;
#33896 = DIRECTION('ref_axis',(1.,0.,0.)) ;
#33897 = DIRECTION('',(0.,0.,1.)) ;
#33898 = DIRECTION('center_axis',(0.,0.,1.)) ;
#33899 = DIRECTION('ref_axis',(1.,0.,0.)) ;
#33900 = DIRECTION('center_axis',(0.,0.,1.)) ;
#33901 = DIRECTION('ref_axis',(1.,0.,0.)) ;
#33902 = DIRECTION('',(0.,0.,-1.)) ;
#33903 = DIRECTION('center_axis',(0.,0.,1.)) ;
#33904 = DIRECTION('ref_axis',(1.,0.,0.)) ;
#33905 = DIRECTION('',(0.,0.,1.)) ;
#33906 = DIRECTION('center_axis',(0.,1.,0.)) ;
#33907 = DIRECTION('ref_axis',(0.,0.,1.)) ;
#33908 = DIRECTION('center_axis',(0.,-1.,0.)) ;
#33909 = DIRECTION('ref_axis',(0.,0.,-1.)) ;
#33910 = DIRECTION('',(0.,0.,1.)) ;
#33911 = DIRECTION('center_axis',(0.,1.,0.)) ;
#33912 = DIRECTION('ref_axis',(0.,0.,1.)) ;
#33913 = DIRECTION('center_axis',(0.,-1.,0.)) ;
#33914 = DIRECTION('ref_axis',(0.,0.,-1.)) ;
#33915 = DIRECTION('',(0.,0.,1.)) ;
#33916 = DIRECTION('center_axis',(0.,1.,0.)) ;
#33917 = DIRECTION('ref_axis',(0.,0.,1.)) ;
#33918 = DIRECTION('center_axis',(0.,-1.,0.)) ;
#33919 = DIRECTION('ref_axis',(0.,0.,-1.)) ;
#33920 = DIRECTION('',(0.,0.,1.)) ;
#33921 = DIRECTION('center_axis',(0.,1.,0.)) ;
#33922 = DIRECTION('ref_axis',(0.,0.,1.)) ;
#33923 = DIRECTION('center_axis',(0.,-1.,0.)) ;
#33924 = DIRECTION('ref_axis',(0.,0.,-1.)) ;
#33925 = DIRECTION('',(0.,0.,1.)) ;
#33926 = DIRECTION('center_axis',(-1.,0.,0.)) ;
#33927 = DIRECTION('ref_axis',(0.,0.,1.)) ;
#33928 = DIRECTION('',(0.,0.,1.)) ;
#33929 = DIRECTION('',(0.,0.,-1.)) ;
#33930 = DIRECTION('center_axis',(0.,1.,0.)) ;
#33931 = DIRECTION('ref_axis',(0.,0.,1.)) ;
#33932 = DIRECTION('',(0.,0.,-1.)) ;
#33933 = DIRECTION('',(0.,0.,1.)) ;
#33934 = DIRECTION('center_axis',(0.,1.,0.)) ;
#33935 = DIRECTION('ref_axis',(0.,0.,1.)) ;
#33936 = DIRECTION('',(0.,0.,-1.)) ;
#33937 = DIRECTION('',(0.,0.,1.)) ;
#33938 = DIRECTION('center_axis',(0.,1.,0.)) ;
#33939 = DIRECTION('ref_axis',(0.,0.,1.)) ;
#33940 = DIRECTION('',(0.,0.,-1.)) ;
#33941 = DIRECTION('',(0.,0.,1.)) ;
#33942 = DIRECTION('center_axis',(0.,1.,0.)) ;
#33943 = DIRECTION('ref_axis',(0.,0.,1.)) ;
#33944 = DIRECTION('',(0.,0.,1.)) ;
#33945 = DIRECTION('center_axis',(0.,1.,0.)) ;
#33946 = DIRECTION('ref_axis',(0.,0.,1.)) ;
#33947 = DIRECTION('',(0.,0.,-1.)) ;
#33948 = DIRECTION('',(0.,0.,1.)) ;
#33949 = DIRECTION('center_axis',(0.,-1.,0.)) ;
#33950 = DIRECTION('ref_axis',(0.,0.,-1.)) ;
#33951 = DIRECTION('',(0.,0.,-1.)) ;
#33952 = DIRECTION('center_axis',(0.,-1.,0.)) ;
#33953 = DIRECTION('ref_axis',(0.,0.,-1.)) ;
#33954 = DIRECTION('',(0.,0.,1.)) ;
#33955 = DIRECTION('',(0.,0.,-1.)) ;
#33956 = DIRECTION('center_axis',(0.,-1.,0.)) ;
#33957 = DIRECTION('ref_axis',(0.,0.,-1.)) ;
#33958 = DIRECTION('',(0.,0.,-1.)) ;
#33959 = DIRECTION('center_axis',(0.,-1.,0.)) ;
#33960 = DIRECTION('ref_axis',(0.,0.,-1.)) ;
#33961 = DIRECTION('',(0.,0.,-1.)) ;
#33962 = DIRECTION('center_axis',(0.,-1.,0.)) ;
#33963 = DIRECTION('ref_axis',(0.,0.,-1.)) ;
#33964 = DIRECTION('',(0.,0.,-1.)) ;
#33965 = DIRECTION('center_axis',(0.,-1.,0.)) ;
#33966 = DIRECTION('ref_axis',(0.,0.,-1.)) ;
#33967 = DIRECTION('center_axis',(1.,0.,0.)) ;
#33968 = DIRECTION('ref_axis',(0.,0.,-1.)) ;
#33969 = DIRECTION('',(0.,0.,-1.)) ;
#33970 = DIRECTION('center_axis',(-1.,0.,0.)) ;
#33971 = DIRECTION('ref_axis',(0.,0.,1.)) ;
#33972 = DIRECTION('center_axis',(1.,0.,0.)) ;
#33973 = DIRECTION('ref_axis',(0.,0.,-1.)) ;
#33974 = DIRECTION('',(0.,0.,1.)) ;
#33975 = DIRECTION('center_axis',(1.,0.,0.)) ;
#33976 = DIRECTION('ref_axis',(0.,0.,-1.)) ;
#33977 = DIRECTION('',(0.,0.,-1.)) ;
#33978 = DIRECTION('center_axis',(0.,0.,1.)) ;
#33979 = DIRECTION('ref_axis',(1.,0.,0.)) ;
#33980 = DIRECTION('center_axis',(0.,0.,1.)) ;
#33981 = DIRECTION('ref_axis',(1.,0.,0.)) ;
#33982 = DIRECTION('',(0.,0.,1.)) ;
#33983 = DIRECTION('center_axis',(0.,0.,1.)) ;
#33984 = DIRECTION('ref_axis',(1.,0.,0.)) ;
#33985 = DIRECTION('',(0.,0.,-1.)) ;
#33986 = DIRECTION('center_axis',(-1.,0.,0.)) ;
#33987 = DIRECTION('ref_axis',(0.,0.,1.)) ;
#33988 = DIRECTION('center_axis',(1.,0.,0.)) ;
#33989 = DIRECTION('ref_axis',(0.,0.,-1.)) ;
#33990 = DIRECTION('',(0.,0.,1.)) ;
#33991 = DIRECTION('center_axis',(-1.,0.,0.)) ;
#33992 = DIRECTION('ref_axis',(0.,0.,1.)) ;
#33993 = DIRECTION('center_axis',(1.,0.,0.)) ;
#33994 = DIRECTION('ref_axis',(0.,0.,-1.)) ;
#33995 = DIRECTION('',(0.,0.,1.)) ;
#33996 = DIRECTION('center_axis',(-1.,0.,0.)) ;
#33997 = DIRECTION('ref_axis',(0.,0.,1.)) ;
#33998 = DIRECTION('center_axis',(1.,0.,0.)) ;
#33999 = DIRECTION('ref_axis',(0.,0.,-1.)) ;
#34000 = DIRECTION('',(0.,0.,1.)) ;
#34001 = DIRECTION('center_axis',(0.,0.,1.)) ;
#34002 = DIRECTION('ref_axis',(1.,0.,0.)) ;
#34003 = DIRECTION('',(0.,0.,1.)) ;
#34004 = DIRECTION('center_axis',(0.,0.,1.)) ;
#34005 = DIRECTION('ref_axis',(1.,0.,0.)) ;
#34006 = DIRECTION('',(0.,0.,1.)) ;
#34007 = DIRECTION('center_axis',(-1.,0.,0.)) ;
#34008 = DIRECTION('ref_axis',(0.,0.,1.)) ;
#34009 = DIRECTION('',(0.,0.,-1.)) ;
#34010 = DIRECTION('center_axis',(-1.,0.,0.)) ;
#34011 = DIRECTION('ref_axis',(0.,0.,1.)) ;
#34012 = DIRECTION('',(0.,0.,-1.)) ;
#34013 = DIRECTION('center_axis',(-1.,0.,0.)) ;
#34014 = DIRECTION('ref_axis',(0.,0.,1.)) ;
#34015 = DIRECTION('',(0.,0.,-1.)) ;
#34016 = DIRECTION('center_axis',(-1.,0.,0.)) ;
#34017 = DIRECTION('ref_axis',(0.,0.,1.)) ;
#34018 = DIRECTION('',(0.,0.,-1.)) ;
#34019 = DIRECTION('',(0.,0.,-1.)) ;
#34020 = DIRECTION('center_axis',(-1.,0.,0.)) ;
#34021 = DIRECTION('ref_axis',(0.,0.,1.)) ;
#34022 = DIRECTION('',(0.,0.,-1.)) ;
#34023 = DIRECTION('center_axis',(-1.,0.,0.)) ;
#34024 = DIRECTION('ref_axis',(0.,0.,1.)) ;
#34025 = DIRECTION('center_axis',(-1.,0.,0.)) ;
#34026 = DIRECTION('ref_axis',(0.,0.,1.)) ;
#34027 = DIRECTION('',(0.,0.,-1.)) ;
#34028 = DIRECTION('center_axis',(1.,0.,0.)) ;
#34029 = DIRECTION('ref_axis',(0.,0.,-1.)) ;
#34030 = DIRECTION('',(0.,0.,1.)) ;
#34031 = DIRECTION('',(0.,0.,-1.)) ;
#34032 = DIRECTION('center_axis',(1.,0.,0.)) ;
#34033 = DIRECTION('ref_axis',(0.,0.,-1.)) ;
#34034 = DIRECTION('',(0.,0.,1.)) ;
#34035 = DIRECTION('',(0.,0.,-1.)) ;
#34036 = DIRECTION('center_axis',(1.,0.,0.)) ;
#34037 = DIRECTION('ref_axis',(0.,0.,-1.)) ;
#34038 = DIRECTION('',(0.,0.,1.)) ;
#34039 = DIRECTION('',(0.,0.,-1.)) ;
#34040 = DIRECTION('center_axis',(1.,0.,0.)) ;
#34041 = DIRECTION('ref_axis',(0.,0.,-1.)) ;
#34042 = DIRECTION('',(0.,0.,-1.)) ;
#34043 = DIRECTION('',(0.,0.,1.)) ;
#34044 = DIRECTION('center_axis',(1.,0.,0.)) ;
#34045 = DIRECTION('ref_axis',(0.,0.,-1.)) ;
#34046 = DIRECTION('',(0.,0.,1.)) ;
#34047 = DIRECTION('',(0.,0.,-1.)) ;
#34048 = DIRECTION('center_axis',(1.,0.,0.)) ;
#34049 = DIRECTION('ref_axis',(0.,0.,-1.)) ;
#34050 = DIRECTION('',(0.,0.,-1.)) ;
#34051 = DIRECTION('',(0.,0.,-1.)) ;
#34052 = DIRECTION('center_axis',(0.,1.,0.)) ;
#34053 = DIRECTION('ref_axis',(0.,0.,1.)) ;
#34054 = DIRECTION('center_axis',(0.,-1.,0.)) ;
#34055 = DIRECTION('ref_axis',(0.,0.,-1.)) ;
#34056 = DIRECTION('center_axis',(0.,-1.,0.)) ;
#34057 = DIRECTION('ref_axis',(0.,0.,-1.)) ;
#34058 = DIRECTION('',(0.,0.,-1.)) ;
#34059 = DIRECTION('center_axis',(0.,1.,0.)) ;
#34060 = DIRECTION('ref_axis',(0.,0.,1.)) ;
#34061 = DIRECTION('',(0.,0.,1.)) ;
#34062 = DIRECTION('center_axis',(0.,1.,0.)) ;
#34063 = DIRECTION('ref_axis',(0.,0.,1.)) ;
#34064 = DIRECTION('center_axis',(0.,0.,1.)) ;
#34065 = DIRECTION('ref_axis',(1.,0.,0.)) ;
#34066 = DIRECTION('center_axis',(0.,0.,1.)) ;
#34067 = DIRECTION('ref_axis',(1.,0.,0.)) ;
#34068 = DIRECTION('',(0.,0.,1.)) ;
#34069 = DIRECTION('center_axis',(0.,1.,0.)) ;
#34070 = DIRECTION('ref_axis',(0.,0.,1.)) ;
#34071 = DIRECTION('center_axis',(0.,-1.,0.)) ;
#34072 = DIRECTION('ref_axis',(0.,0.,-1.)) ;
#34073 = DIRECTION('',(0.,0.,1.)) ;
#34074 = DIRECTION('center_axis',(0.,0.,1.)) ;
#34075 = DIRECTION('ref_axis',(1.,0.,0.)) ;
#34076 = DIRECTION('center_axis',(0.,0.,1.)) ;
#34077 = DIRECTION('ref_axis',(1.,0.,0.)) ;
#34078 = DIRECTION('',(0.,0.,-1.)) ;
#34079 = DIRECTION('center_axis',(0.,0.,1.)) ;
#34080 = DIRECTION('ref_axis',(1.,0.,0.)) ;
#34081 = DIRECTION('',(0.,0.,1.)) ;
#34082 = DIRECTION('center_axis',(0.,1.,0.)) ;
#34083 = DIRECTION('ref_axis',(0.,0.,1.)) ;
#34084 = DIRECTION('center_axis',(0.,-1.,0.)) ;
#34085 = DIRECTION('ref_axis',(0.,0.,-1.)) ;
#34086 = DIRECTION('',(0.,0.,1.)) ;
#34087 = DIRECTION('center_axis',(0.,1.,0.)) ;
#34088 = DIRECTION('ref_axis',(0.,0.,1.)) ;
#34089 = DIRECTION('center_axis',(0.,-1.,0.)) ;
#34090 = DIRECTION('ref_axis',(0.,0.,-1.)) ;
#34091 = DIRECTION('',(0.,0.,1.)) ;
#34092 = DIRECTION('center_axis',(0.,-1.,0.)) ;
#34093 = DIRECTION('ref_axis',(0.,0.,-1.)) ;
#34094 = DIRECTION('',(0.,0.,-1.)) ;
#34095 = DIRECTION('center_axis',(0.,-1.,0.)) ;
#34096 = DIRECTION('ref_axis',(0.,0.,-1.)) ;
#34097 = DIRECTION('',(0.,0.,-1.)) ;
#34098 = DIRECTION('center_axis',(0.,-1.,0.)) ;
#34099 = DIRECTION('ref_axis',(0.,0.,-1.)) ;
#34100 = DIRECTION('',(0.,0.,-1.)) ;
#34101 = DIRECTION('center_axis',(0.,-1.,0.)) ;
#34102 = DIRECTION('ref_axis',(0.,0.,-1.)) ;
#34103 = DIRECTION('',(0.,0.,-1.)) ;
#34104 = DIRECTION('center_axis',(0.,-1.,0.)) ;
#34105 = DIRECTION('ref_axis',(0.,0.,-1.)) ;
#34106 = DIRECTION('',(0.,0.,-1.)) ;
#34107 = DIRECTION('center_axis',(0.,-1.,0.)) ;
#34108 = DIRECTION('ref_axis',(0.,0.,-1.)) ;
#34109 = DIRECTION('center_axis',(0.,1.,0.)) ;
#34110 = DIRECTION('ref_axis',(0.,0.,1.)) ;
#34111 = DIRECTION('',(0.,0.,1.)) ;
#34112 = DIRECTION('',(0.,0.,-1.)) ;
#34113 = DIRECTION('center_axis',(0.,1.,0.)) ;
#34114 = DIRECTION('ref_axis',(0.,0.,1.)) ;
#34115 = DIRECTION('',(0.,0.,-1.)) ;
#34116 = DIRECTION('',(0.,0.,-1.)) ;
#34117 = DIRECTION('center_axis',(0.,1.,0.)) ;
#34118 = DIRECTION('ref_axis',(0.,0.,1.)) ;
#34119 = DIRECTION('',(0.,0.,-1.)) ;
#34120 = DIRECTION('',(0.,0.,1.)) ;
#34121 = DIRECTION('center_axis',(0.,1.,0.)) ;
#34122 = DIRECTION('ref_axis',(0.,0.,1.)) ;
#34123 = DIRECTION('',(0.,0.,-1.)) ;
#34124 = DIRECTION('',(0.,0.,1.)) ;
#34125 = DIRECTION('center_axis',(0.,1.,0.)) ;
#34126 = DIRECTION('ref_axis',(0.,0.,1.)) ;
#34127 = DIRECTION('',(0.,0.,-1.)) ;
#34128 = DIRECTION('',(0.,0.,1.)) ;
#34129 = DIRECTION('center_axis',(1.,0.,0.)) ;
#34130 = DIRECTION('ref_axis',(0.,0.,-1.)) ;
#34131 = DIRECTION('center_axis',(-1.,0.,0.)) ;
#34132 = DIRECTION('ref_axis',(0.,0.,1.)) ;
#34133 = DIRECTION('center_axis',(1.,0.,0.)) ;
#34134 = DIRECTION('ref_axis',(0.,0.,-1.)) ;
#34135 = DIRECTION('',(0.,0.,-1.)) ;
#34136 = DIRECTION('center_axis',(-1.,0.,0.)) ;
#34137 = DIRECTION('ref_axis',(0.,0.,1.)) ;
#34138 = DIRECTION('center_axis',(-1.,0.,0.)) ;
#34139 = DIRECTION('ref_axis',(0.,0.,1.)) ;
#34140 = DIRECTION('center_axis',(-1.,0.,0.)) ;
#34141 = DIRECTION('ref_axis',(0.,0.,1.)) ;
#34142 = DIRECTION('center_axis',(1.,0.,0.)) ;
#34143 = DIRECTION('ref_axis',(0.,0.,-1.)) ;
#34144 = DIRECTION('',(0.,0.,1.)) ;
#34145 = DIRECTION('center_axis',(0.,0.,1.)) ;
#34146 = DIRECTION('ref_axis',(1.,0.,0.)) ;
#34147 = DIRECTION('',(0.,0.,1.)) ;
#34148 = DIRECTION('center_axis',(-1.,0.,0.)) ;
#34149 = DIRECTION('ref_axis',(0.,0.,1.)) ;
#34150 = DIRECTION('center_axis',(1.,0.,0.)) ;
#34151 = DIRECTION('ref_axis',(0.,0.,-1.)) ;
#34152 = DIRECTION('',(0.,0.,1.)) ;
#34153 = DIRECTION('center_axis',(0.,0.,1.)) ;
#34154 = DIRECTION('ref_axis',(1.,0.,0.)) ;
#34155 = DIRECTION('',(0.,0.,-1.)) ;
#34156 = DIRECTION('center_axis',(0.,0.,1.)) ;
#34157 = DIRECTION('ref_axis',(1.,0.,0.)) ;
#34158 = DIRECTION('center_axis',(0.,0.,1.)) ;
#34159 = DIRECTION('ref_axis',(1.,0.,0.)) ;
#34160 = DIRECTION('',(0.,0.,1.)) ;
#34161 = DIRECTION('center_axis',(0.,-1.,0.)) ;
#34162 = DIRECTION('ref_axis',(0.,0.,-1.)) ;
#34163 = DIRECTION('',(0.,0.,-1.)) ;
#34164 = DIRECTION('center_axis',(1.,0.,0.)) ;
#34165 = DIRECTION('ref_axis',(0.,0.,-1.)) ;
#34166 = DIRECTION('',(0.,0.,1.)) ;
#34167 = DIRECTION('',(0.,0.,-1.)) ;
#34168 = DIRECTION('center_axis',(1.,0.,0.)) ;
#34169 = DIRECTION('ref_axis',(0.,0.,-1.)) ;
#34170 = DIRECTION('',(0.,0.,1.)) ;
#34171 = DIRECTION('',(0.,0.,-1.)) ;
#34172 = DIRECTION('center_axis',(1.,0.,0.)) ;
#34173 = DIRECTION('ref_axis',(0.,0.,-1.)) ;
#34174 = DIRECTION('',(0.,0.,1.)) ;
#34175 = DIRECTION('',(0.,0.,-1.)) ;
#34176 = DIRECTION('center_axis',(1.,0.,0.)) ;
#34177 = DIRECTION('ref_axis',(0.,0.,-1.)) ;
#34178 = DIRECTION('',(0.,0.,-1.)) ;
#34179 = DIRECTION('center_axis',(1.,0.,0.)) ;
#34180 = DIRECTION('ref_axis',(0.,0.,-1.)) ;
#34181 = DIRECTION('',(0.,0.,1.)) ;
#34182 = DIRECTION('',(0.,0.,-1.)) ;
#34183 = DIRECTION('center_axis',(1.,0.,0.)) ;
#34184 = DIRECTION('ref_axis',(0.,0.,-1.)) ;
#34185 = DIRECTION('center_axis',(-1.,0.,0.)) ;
#34186 = DIRECTION('ref_axis',(0.,0.,1.)) ;
#34187 = DIRECTION('',(0.,0.,-1.)) ;
#34188 = DIRECTION('center_axis',(-1.,0.,0.)) ;
#34189 = DIRECTION('ref_axis',(0.,0.,1.)) ;
#34190 = DIRECTION('',(0.,0.,-1.)) ;
#34191 = DIRECTION('center_axis',(0.,1.,0.)) ;
#34192 = DIRECTION('ref_axis',(0.,0.,1.)) ;
#34193 = DIRECTION('center_axis',(-1.,0.,0.)) ;
#34194 = DIRECTION('ref_axis',(0.,0.,1.)) ;
#34195 = DIRECTION('',(0.,0.,-1.)) ;
#34196 = DIRECTION('center_axis',(0.,1.,0.)) ;
#34197 = DIRECTION('ref_axis',(0.,0.,1.)) ;
#34198 = DIRECTION('center_axis',(0.,-1.,0.)) ;
#34199 = DIRECTION('ref_axis',(0.,0.,-1.)) ;
#34200 = DIRECTION('center_axis',(0.,-1.,0.)) ;
#34201 = DIRECTION('ref_axis',(0.,0.,-1.)) ;
#34202 = DIRECTION('',(0.,0.,-1.)) ;
#34203 = DIRECTION('center_axis',(0.,1.,0.)) ;
#34204 = DIRECTION('ref_axis',(0.,0.,1.)) ;
#34205 = DIRECTION('center_axis',(0.,-1.,0.)) ;
#34206 = DIRECTION('ref_axis',(0.,0.,-1.)) ;
#34207 = DIRECTION('',(0.,0.,1.)) ;
#34208 = DIRECTION('center_axis',(0.,0.,1.)) ;
#34209 = DIRECTION('ref_axis',(1.,0.,0.)) ;
#34210 = DIRECTION('',(0.,0.,1.)) ;
#34211 = DIRECTION('center_axis',(0.,-1.,0.)) ;
#34212 = DIRECTION('ref_axis',(0.,0.,-1.)) ;
#34213 = DIRECTION('',(0.,0.,1.)) ;
#34214 = DIRECTION('center_axis',(0.,1.,0.)) ;
#34215 = DIRECTION('ref_axis',(0.,0.,1.)) ;
#34216 = DIRECTION('center_axis',(0.,0.,1.)) ;
#34217 = DIRECTION('ref_axis',(1.,0.,0.)) ;
#34218 = DIRECTION('',(0.,0.,-1.)) ;
#34219 = DIRECTION('center_axis',(0.,0.,1.)) ;
#34220 = DIRECTION('ref_axis',(1.,0.,0.)) ;
#34221 = DIRECTION('',(0.,0.,1.)) ;
#34222 = DIRECTION('center_axis',(1.,0.,0.)) ;
#34223 = DIRECTION('ref_axis',(0.,0.,-1.)) ;
#34224 = DIRECTION('',(0.,0.,-1.)) ;
#34225 = DIRECTION('center_axis',(0.,-1.,0.)) ;
#34226 = DIRECTION('ref_axis',(0.,0.,-1.)) ;
#34227 = DIRECTION('center_axis',(0.,-1.,0.)) ;
#34228 = DIRECTION('ref_axis',(0.,0.,-1.)) ;
#34229 = DIRECTION('',(0.,0.,-1.)) ;
#34230 = DIRECTION('center_axis',(0.,1.,0.)) ;
#34231 = DIRECTION('ref_axis',(0.,0.,1.)) ;
#34232 = DIRECTION('',(0.,0.,-1.)) ;
#34233 = DIRECTION('center_axis',(0.,1.,0.)) ;
#34234 = DIRECTION('ref_axis',(0.,0.,1.)) ;
#34235 = DIRECTION('',(0.,0.,-1.)) ;
#34236 = DIRECTION('',(0.,0.,1.)) ;
#34237 = DIRECTION('center_axis',(0.,1.,0.)) ;
#34238 = DIRECTION('ref_axis',(0.,0.,1.)) ;
#34239 = DIRECTION('',(0.,0.,1.)) ;
#34240 = DIRECTION('',(0.,0.,-1.)) ;
#34241 = DIRECTION('center_axis',(0.,1.,0.)) ;
#34242 = DIRECTION('ref_axis',(0.,0.,1.)) ;
#34243 = DIRECTION('',(0.,0.,-1.)) ;
#34244 = DIRECTION('',(0.,0.,1.)) ;
#34245 = DIRECTION('center_axis',(0.,1.,0.)) ;
#34246 = DIRECTION('ref_axis',(0.,0.,1.)) ;
#34247 = DIRECTION('',(0.,0.,1.)) ;
#34248 = DIRECTION('center_axis',(-1.,0.,0.)) ;
#34249 = DIRECTION('ref_axis',(0.,0.,1.)) ;
#34250 = DIRECTION('',(0.,0.,-1.)) ;
#34251 = DIRECTION('center_axis',(-1.,0.,0.)) ;
#34252 = DIRECTION('ref_axis',(0.,0.,1.)) ;
#34253 = DIRECTION('center_axis',(1.,0.,0.)) ;
#34254 = DIRECTION('ref_axis',(0.,0.,-1.)) ;
#34255 = DIRECTION('',(0.,0.,-1.)) ;
#34256 = DIRECTION('center_axis',(0.,0.,1.)) ;
#34257 = DIRECTION('ref_axis',(1.,0.,0.)) ;
#34258 = DIRECTION('center_axis',(0.,0.,1.)) ;
#34259 = DIRECTION('ref_axis',(1.,0.,0.)) ;
#34260 = DIRECTION('',(0.,0.,-1.)) ;
#34261 = DIRECTION('center_axis',(0.,0.,1.)) ;
#34262 = DIRECTION('ref_axis',(1.,0.,0.)) ;
#34263 = DIRECTION('center_axis',(-1.,0.,0.)) ;
#34264 = DIRECTION('ref_axis',(0.,0.,1.)) ;
#34265 = DIRECTION('center_axis',(1.,0.,0.)) ;
#34266 = DIRECTION('ref_axis',(0.,0.,-1.)) ;
#34267 = DIRECTION('',(0.,0.,-1.)) ;
#34268 = DIRECTION('center_axis',(0.,0.,1.)) ;
#34269 = DIRECTION('ref_axis',(1.,0.,0.)) ;
#34270 = DIRECTION('',(0.,0.,1.)) ;
#34271 = DIRECTION('center_axis',(0.,0.,1.)) ;
#34272 = DIRECTION('ref_axis',(1.,0.,0.)) ;
#34273 = DIRECTION('center_axis',(0.,-1.,0.)) ;
#34274 = DIRECTION('ref_axis',(0.,0.,-1.)) ;
#34275 = DIRECTION('',(0.,0.,-1.)) ;
#34276 = DIRECTION('center_axis',(-1.,0.,0.)) ;
#34277 = DIRECTION('ref_axis',(0.,0.,1.)) ;
#34278 = DIRECTION('center_axis',(1.,0.,0.)) ;
#34279 = DIRECTION('ref_axis',(0.,0.,-1.)) ;
#34280 = DIRECTION('',(0.,0.,1.)) ;
#34281 = DIRECTION('',(0.,0.,-1.)) ;
#34282 = DIRECTION('center_axis',(1.,0.,0.)) ;
#34283 = DIRECTION('ref_axis',(0.,0.,-1.)) ;
#34284 = DIRECTION('center_axis',(1.,0.,0.)) ;
#34285 = DIRECTION('ref_axis',(0.,0.,-1.)) ;
#34286 = DIRECTION('',(0.,0.,1.)) ;
#34287 = DIRECTION('',(0.,0.,-1.)) ;
#34288 = DIRECTION('center_axis',(0.,1.,0.)) ;
#34289 = DIRECTION('ref_axis',(0.,0.,1.)) ;
#34290 = DIRECTION('center_axis',(-1.,0.,0.)) ;
#34291 = DIRECTION('ref_axis',(0.,0.,1.)) ;
#34292 = DIRECTION('',(0.,0.,-1.)) ;
#34293 = DIRECTION('center_axis',(0.,1.,0.)) ;
#34294 = DIRECTION('ref_axis',(0.,0.,1.)) ;
#34295 = DIRECTION('center_axis',(0.,-1.,0.)) ;
#34296 = DIRECTION('ref_axis',(0.,0.,-1.)) ;
#34297 = DIRECTION('',(0.,0.,-1.)) ;
#34298 = DIRECTION('center_axis',(0.,0.,1.)) ;
#34299 = DIRECTION('ref_axis',(1.,0.,0.)) ;
#34300 = DIRECTION('center_axis',(0.,-1.,0.)) ;
#34301 = DIRECTION('ref_axis',(0.,0.,-1.)) ;
#34302 = DIRECTION('',(0.,0.,-1.)) ;
#34303 = DIRECTION('center_axis',(0.,0.,1.)) ;
#34304 = DIRECTION('ref_axis',(1.,0.,0.)) ;
#34305 = DIRECTION('',(0.,0.,-1.)) ;
#34306 = DIRECTION('center_axis',(1.,0.,0.)) ;
#34307 = DIRECTION('ref_axis',(0.,0.,-1.)) ;
#34308 = DIRECTION('',(0.,0.,-1.)) ;
#34309 = DIRECTION('center_axis',(0.,1.,0.)) ;
#34310 = DIRECTION('ref_axis',(0.,0.,1.)) ;
#34311 = DIRECTION('',(0.,0.,-1.)) ;
#34312 = DIRECTION('center_axis',(0.,1.,0.)) ;
#34313 = DIRECTION('ref_axis',(0.,0.,1.)) ;
#34314 = DIRECTION('',(0.,0.,-1.)) ;
#34315 = DIRECTION('center_axis',(0.,1.,0.)) ;
#34316 = DIRECTION('ref_axis',(0.,0.,1.)) ;
#34317 = DIRECTION('',(0.,0.,1.)) ;
#34318 = DIRECTION('center_axis',(-1.,0.,0.)) ;
#34319 = DIRECTION('ref_axis',(0.,0.,1.)) ;
#34320 = DIRECTION('center_axis',(-1.,0.,0.)) ;
#34321 = DIRECTION('ref_axis',(0.,0.,1.)) ;
#34322 = DIRECTION('',(0.,0.,1.)) ;
#34323 = DIRECTION('center_axis',(-1.,0.,0.)) ;
#34324 = DIRECTION('ref_axis',(0.,0.,1.)) ;
#34325 = DIRECTION('center_axis',(0.,0.,1.)) ;
#34326 = DIRECTION('ref_axis',(1.,0.,0.)) ;
#34327 = DIRECTION('',(0.,0.,1.)) ;
#34328 = DIRECTION('center_axis',(0.,-1.,0.)) ;
#34329 = DIRECTION('ref_axis',(0.,0.,-1.)) ;
#34330 = DIRECTION('',(0.,0.,-1.)) ;
#34331 = DIRECTION('center_axis',(1.,0.,0.)) ;
#34332 = DIRECTION('ref_axis',(0.,0.,-1.)) ;
#34333 = DIRECTION('center_axis',(1.,0.,0.)) ;
#34334 = DIRECTION('ref_axis',(0.,0.,-1.)) ;
#34335 = DIRECTION('center_axis',(1.,0.,0.)) ;
#34336 = DIRECTION('ref_axis',(0.,0.,-1.)) ;
#34337 = DIRECTION('',(0.,0.,-1.)) ;
#34338 = DIRECTION('center_axis',(0.,1.,0.)) ;
#34339 = DIRECTION('ref_axis',(0.,0.,1.)) ;
#34340 = DIRECTION('',(0.,0.,-1.)) ;
#34341 = DIRECTION('center_axis',(0.,0.,1.)) ;
#34342 = DIRECTION('ref_axis',(1.,0.,0.)) ;
#34343 = DIRECTION('',(0.,0.,1.)) ;
#34344 = DIRECTION('center_axis',(0.,0.,1.)) ;
#34345 = DIRECTION('ref_axis',(1.,0.,0.)) ;
#34346 = DIRECTION('center_axis',(0.,-1.,0.)) ;
#34347 = DIRECTION('ref_axis',(0.,0.,-1.)) ;
#34348 = DIRECTION('center_axis',(1.,0.,0.)) ;
#34349 = DIRECTION('ref_axis',(0.,0.,-1.)) ;
#34350 = DIRECTION('',(0.,0.,-1.)) ;
#34351 = DIRECTION('center_axis',(0.,1.,0.)) ;
#34352 = DIRECTION('ref_axis',(0.,0.,1.)) ;
#34353 = DIRECTION('',(0.,0.,-1.)) ;
#34354 = DIRECTION('center_axis',(0.,1.,0.)) ;
#34355 = DIRECTION('ref_axis',(0.,0.,1.)) ;
#34356 = DIRECTION('center_axis',(0.,1.,0.)) ;
#34357 = DIRECTION('ref_axis',(0.,0.,1.)) ;
#34358 = DIRECTION('center_axis',(-1.,0.,0.)) ;
#34359 = DIRECTION('ref_axis',(0.,0.,1.)) ;
#34360 = DIRECTION('axis',(0.,0.,1.)) ;
#34361 = DIRECTION('refdir',(1.,0.,0.)) ;
#34362 = DIRECTION('center_axis',(0.,0.,1.)) ;
#34363 = DIRECTION('ref_axis',(1.,0.,0.)) ;
#34364 = DIRECTION('center_axis',(0.111964476103308,0.993712209893243,0.)) ;
#34365 = DIRECTION('ref_axis',(0.993712209893243,-0.111964476103308,0.)) ;
#34366 = DIRECTION('center_axis',(0.111964476103307,-0.993712209893243,0.)) ;
#34367 = DIRECTION('ref_axis',(0.993712209893243,0.111964476103307,0.)) ;
#34368 = DIRECTION('center_axis',(0.,0.,1.)) ;
#34369 = DIRECTION('ref_axis',(1.,0.,0.)) ;
#34370 = DIRECTION('center_axis',(-0.111964476103308,-0.993712209893243,0.)) ;
#34371 = DIRECTION('ref_axis',(0.993712209893243,-0.111964476103308,0.)) ;
#34372 = DIRECTION('center_axis',(0.330279061955167,0.943883330308368,0.)) ;
#34373 = DIRECTION('ref_axis',(0.943883330308368,-0.330279061955167,0.)) ;
#34374 = DIRECTION('center_axis',(0.,0.,1.)) ;
#34375 = DIRECTION('ref_axis',(1.,0.,0.)) ;
#34376 = DIRECTION('center_axis',(-0.330279061955167,-0.943883330308368,0.)) ;
#34377 = DIRECTION('ref_axis',(0.943883330308368,-0.330279061955167,0.)) ;
#34378 = DIRECTION('center_axis',(0.532032076515336,0.846724199228284,0.)) ;
#34379 = DIRECTION('ref_axis',(0.846724199228285,-0.532032076515336,0.)) ;
#34380 = DIRECTION('center_axis',(0.,0.,1.)) ;
#34381 = DIRECTION('ref_axis',(1.,0.,0.)) ;
#34382 = DIRECTION('center_axis',(-0.532032076515336,-0.846724199228284,0.)) ;
#34383 = DIRECTION('ref_axis',(0.846724199228285,-0.532032076515336,0.)) ;
#34384 = DIRECTION('center_axis',(0.707106781186548,0.707106781186547,0.)) ;
#34385 = DIRECTION('ref_axis',(0.707106781186547,-0.707106781186548,0.)) ;
#34386 = DIRECTION('center_axis',(0.,0.,1.)) ;
#34387 = DIRECTION('ref_axis',(1.,0.,0.)) ;
#34388 = DIRECTION('center_axis',(-0.707106781186548,-0.707106781186547,0.)) ;
#34389 = DIRECTION('ref_axis',(0.707106781186547,-0.707106781186548,0.)) ;
#34390 = DIRECTION('center_axis',(0.846724199228284,0.532032076515337,0.)) ;
#34391 = DIRECTION('ref_axis',(0.532032076515337,-0.846724199228284,0.)) ;
#34392 = DIRECTION('center_axis',(0.,0.,1.)) ;
#34393 = DIRECTION('ref_axis',(1.,0.,0.)) ;
#34394 = DIRECTION('center_axis',(-0.846724199228284,-0.532032076515337,0.)) ;
#34395 = DIRECTION('ref_axis',(0.532032076515337,-0.846724199228284,0.)) ;
#34396 = DIRECTION('center_axis',(0.943883330308368,0.330279061955166,0.)) ;
#34397 = DIRECTION('ref_axis',(0.330279061955166,-0.943883330308368,0.)) ;
#34398 = DIRECTION('center_axis',(0.,0.,1.)) ;
#34399 = DIRECTION('ref_axis',(1.,0.,0.)) ;
#34400 = DIRECTION('center_axis',(-0.943883330308368,-0.330279061955166,0.)) ;
#34401 = DIRECTION('ref_axis',(0.330279061955166,-0.943883330308368,0.)) ;
#34402 = DIRECTION('center_axis',(0.993712209893243,0.111964476103307,0.)) ;
#34403 = DIRECTION('ref_axis',(0.111964476103307,-0.993712209893243,0.)) ;
#34404 = DIRECTION('center_axis',(6.12323399573676E-17,0.,1.)) ;
#34405 = DIRECTION('ref_axis',(1.,0.,0.)) ;
#34406 = DIRECTION('center_axis',(-0.993712209893243,-0.111964476103307,0.)) ;
#34407 = DIRECTION('ref_axis',(0.111964476103307,-0.993712209893243,0.)) ;
#34408 = DIRECTION('center_axis',(0.993712209893243,-0.111964476103307,0.)) ;
#34409 = DIRECTION('ref_axis',(0.111964476103307,0.993712209893243,0.)) ;
#34410 = DIRECTION('center_axis',(0.993712209893243,-0.111964476103307,0.)) ;
#34411 = DIRECTION('ref_axis',(0.111964476103307,0.993712209893243,0.)) ;
#34412 = DIRECTION('center_axis',(0.,0.,1.)) ;
#34413 = DIRECTION('ref_axis',(1.,0.,0.)) ;
#34414 = DIRECTION('center_axis',(-0.993712209893243,0.111964476103307,0.)) ;
#34415 = DIRECTION('ref_axis',(0.111964476103307,0.993712209893243,0.)) ;
#34416 = DIRECTION('center_axis',(-0.993712209893243,0.111964476103307,0.)) ;
#34417 = DIRECTION('ref_axis',(0.111964476103307,0.993712209893243,0.)) ;
#34418 = DIRECTION('center_axis',(0.943883330308367,-0.330279061955168,0.)) ;
#34419 = DIRECTION('ref_axis',(0.330279061955168,0.943883330308367,0.)) ;
#34420 = DIRECTION('center_axis',(0.943883330308367,-0.330279061955168,0.)) ;
#34421 = DIRECTION('ref_axis',(0.330279061955168,0.943883330308367,0.)) ;
#34422 = DIRECTION('center_axis',(0.,0.,1.)) ;
#34423 = DIRECTION('ref_axis',(1.,0.,0.)) ;
#34424 = DIRECTION('center_axis',(-0.943883330308367,0.330279061955168,0.)) ;
#34425 = DIRECTION('ref_axis',(0.330279061955168,0.943883330308367,0.)) ;
#34426 = DIRECTION('center_axis',(-0.943883330308367,0.330279061955168,0.)) ;
#34427 = DIRECTION('ref_axis',(0.330279061955168,0.943883330308367,0.)) ;
#34428 = DIRECTION('center_axis',(0.846724199228284,-0.532032076515337,0.)) ;
#34429 = DIRECTION('ref_axis',(0.532032076515337,0.846724199228284,0.)) ;
#34430 = DIRECTION('center_axis',(0.846724199228284,-0.532032076515337,0.)) ;
#34431 = DIRECTION('ref_axis',(0.532032076515337,0.846724199228284,0.)) ;
#34432 = DIRECTION('center_axis',(0.,0.,1.)) ;
#34433 = DIRECTION('ref_axis',(1.,0.,0.)) ;
#34434 = DIRECTION('center_axis',(-0.846724199228284,0.532032076515337,0.)) ;
#34435 = DIRECTION('ref_axis',(0.532032076515337,0.846724199228284,0.)) ;
#34436 = DIRECTION('center_axis',(-0.846724199228284,0.532032076515337,0.)) ;
#34437 = DIRECTION('ref_axis',(0.532032076515337,0.846724199228284,0.)) ;
#34438 = DIRECTION('center_axis',(0.707106781186548,-0.707106781186547,0.)) ;
#34439 = DIRECTION('ref_axis',(0.707106781186547,0.707106781186548,0.)) ;
#34440 = DIRECTION('center_axis',(0.707106781186548,-0.707106781186547,0.)) ;
#34441 = DIRECTION('ref_axis',(0.707106781186547,0.707106781186548,0.)) ;
#34442 = DIRECTION('center_axis',(0.,0.,1.)) ;
#34443 = DIRECTION('ref_axis',(1.,0.,0.)) ;
#34444 = DIRECTION('center_axis',(-0.707106781186548,0.707106781186547,0.)) ;
#34445 = DIRECTION('ref_axis',(0.707106781186547,0.707106781186548,0.)) ;
#34446 = DIRECTION('center_axis',(-0.707106781186548,0.707106781186547,0.)) ;
#34447 = DIRECTION('ref_axis',(0.707106781186547,0.707106781186548,0.)) ;
#34448 = DIRECTION('center_axis',(0.532032076515336,-0.846724199228284,0.)) ;
#34449 = DIRECTION('ref_axis',(0.846724199228284,0.532032076515336,0.)) ;
#34450 = DIRECTION('center_axis',(0.532032076515336,-0.846724199228284,0.)) ;
#34451 = DIRECTION('ref_axis',(0.846724199228284,0.532032076515336,0.)) ;
#34452 = DIRECTION('center_axis',(0.,0.,1.)) ;
#34453 = DIRECTION('ref_axis',(1.,0.,0.)) ;
#34454 = DIRECTION('center_axis',(-0.532032076515336,0.846724199228284,0.)) ;
#34455 = DIRECTION('ref_axis',(0.846724199228284,0.532032076515336,0.)) ;
#34456 = DIRECTION('center_axis',(-0.532032076515336,0.846724199228284,0.)) ;
#34457 = DIRECTION('ref_axis',(0.846724199228284,0.532032076515336,0.)) ;
#34458 = DIRECTION('center_axis',(0.330279061955167,-0.943883330308368,0.)) ;
#34459 = DIRECTION('ref_axis',(0.943883330308368,0.330279061955167,0.)) ;
#34460 = DIRECTION('center_axis',(0.330279061955167,-0.943883330308368,0.)) ;
#34461 = DIRECTION('ref_axis',(0.943883330308368,0.330279061955167,0.)) ;
#34462 = DIRECTION('center_axis',(0.,0.,1.)) ;
#34463 = DIRECTION('ref_axis',(1.,0.,0.)) ;
#34464 = DIRECTION('center_axis',(-0.330279061955167,0.943883330308368,0.)) ;
#34465 = DIRECTION('ref_axis',(0.943883330308368,0.330279061955167,0.)) ;
#34466 = DIRECTION('center_axis',(-0.330279061955167,0.943883330308368,0.)) ;
#34467 = DIRECTION('ref_axis',(0.943883330308368,0.330279061955167,0.)) ;
#34468 = DIRECTION('center_axis',(0.111964476103307,-0.993712209893243,0.)) ;
#34469 = DIRECTION('ref_axis',(0.993712209893243,0.111964476103307,0.)) ;
#34470 = DIRECTION('center_axis',(0.111964476103307,-0.993712209893243,0.)) ;
#34471 = DIRECTION('ref_axis',(0.993712209893243,0.111964476103307,0.)) ;
#34472 = DIRECTION('center_axis',(0.,-1.32134201624519E-28,1.)) ;
#34473 = DIRECTION('ref_axis',(-1.,-2.15839602455122E-12,0.)) ;
#34474 = DIRECTION('center_axis',(-0.111964476103307,0.993712209893243,0.)) ;
#34475 = DIRECTION('ref_axis',(0.993712209893243,0.111964476103307,0.)) ;
#34476 = DIRECTION('center_axis',(-0.111964476103307,0.993712209893243,0.)) ;
#34477 = DIRECTION('ref_axis',(0.993712209893243,0.111964476103307,0.)) ;
#34478 = DIRECTION('center_axis',(-0.111964476103307,-0.993712209893243,0.)) ;
#34479 = DIRECTION('ref_axis',(0.993712209893243,-0.111964476103307,0.)) ;
#34480 = DIRECTION('center_axis',(-0.111964476103307,-0.993712209893243,0.)) ;
#34481 = DIRECTION('ref_axis',(0.993712209893243,-0.111964476103307,0.)) ;
#34482 = DIRECTION('center_axis',(0.,0.,1.)) ;
#34483 = DIRECTION('ref_axis',(1.,0.,0.)) ;
#34484 = DIRECTION('center_axis',(0.111964476103307,0.993712209893243,0.)) ;
#34485 = DIRECTION('ref_axis',(0.993712209893243,-0.111964476103307,0.)) ;
#34486 = DIRECTION('center_axis',(0.111964476103307,0.993712209893243,0.)) ;
#34487 = DIRECTION('ref_axis',(0.993712209893243,-0.111964476103307,0.)) ;
#34488 = DIRECTION('center_axis',(-0.330279061955167,-0.943883330308367,0.)) ;
#34489 = DIRECTION('ref_axis',(0.943883330308368,-0.330279061955167,0.)) ;
#34490 = DIRECTION('center_axis',(-0.330279061955167,-0.943883330308367,0.)) ;
#34491 = DIRECTION('ref_axis',(0.943883330308368,-0.330279061955167,0.)) ;
#34492 = DIRECTION('center_axis',(0.,0.,1.)) ;
#34493 = DIRECTION('ref_axis',(1.,0.,0.)) ;
#34494 = DIRECTION('center_axis',(0.330279061955167,0.943883330308367,0.)) ;
#34495 = DIRECTION('ref_axis',(0.943883330308368,-0.330279061955167,0.)) ;
#34496 = DIRECTION('center_axis',(0.330279061955167,0.943883330308367,0.)) ;
#34497 = DIRECTION('ref_axis',(0.943883330308368,-0.330279061955167,0.)) ;
#34498 = DIRECTION('center_axis',(-0.532032076515337,-0.846724199228284,0.)) ;
#34499 = DIRECTION('ref_axis',(0.846724199228284,-0.532032076515337,0.)) ;
#34500 = DIRECTION('center_axis',(-0.532032076515337,-0.846724199228284,0.)) ;
#34501 = DIRECTION('ref_axis',(0.846724199228284,-0.532032076515337,0.)) ;
#34502 = DIRECTION('center_axis',(0.,0.,1.)) ;
#34503 = DIRECTION('ref_axis',(1.,0.,0.)) ;
#34504 = DIRECTION('center_axis',(0.532032076515337,0.846724199228284,0.)) ;
#34505 = DIRECTION('ref_axis',(0.846724199228284,-0.532032076515337,0.)) ;
#34506 = DIRECTION('center_axis',(0.532032076515337,0.846724199228284,0.)) ;
#34507 = DIRECTION('ref_axis',(0.846724199228284,-0.532032076515337,0.)) ;
#34508 = DIRECTION('center_axis',(-0.707106781186548,-0.707106781186548,0.)) ;
#34509 = DIRECTION('ref_axis',(0.707106781186548,-0.707106781186548,0.)) ;
#34510 = DIRECTION('center_axis',(-0.707106781186548,-0.707106781186548,0.)) ;
#34511 = DIRECTION('ref_axis',(0.707106781186548,-0.707106781186548,0.)) ;
#34512 = DIRECTION('center_axis',(0.,0.,1.)) ;
#34513 = DIRECTION('ref_axis',(1.,0.,0.)) ;
#34514 = DIRECTION('center_axis',(0.707106781186548,0.707106781186548,0.)) ;
#34515 = DIRECTION('ref_axis',(0.707106781186548,-0.707106781186548,0.)) ;
#34516 = DIRECTION('center_axis',(0.707106781186548,0.707106781186548,0.)) ;
#34517 = DIRECTION('ref_axis',(0.707106781186548,-0.707106781186548,0.)) ;
#34518 = DIRECTION('center_axis',(-0.846724199228285,-0.532032076515336,0.)) ;
#34519 = DIRECTION('ref_axis',(0.532032076515336,-0.846724199228285,0.)) ;
#34520 = DIRECTION('center_axis',(-0.846724199228285,-0.532032076515336,0.)) ;
#34521 = DIRECTION('ref_axis',(0.532032076515336,-0.846724199228285,0.)) ;
#34522 = DIRECTION('center_axis',(0.,0.,1.)) ;
#34523 = DIRECTION('ref_axis',(1.,0.,0.)) ;
#34524 = DIRECTION('center_axis',(0.846724199228285,0.532032076515336,0.)) ;
#34525 = DIRECTION('ref_axis',(0.532032076515336,-0.846724199228285,0.)) ;
#34526 = DIRECTION('center_axis',(0.846724199228285,0.532032076515336,0.)) ;
#34527 = DIRECTION('ref_axis',(0.532032076515336,-0.846724199228285,0.)) ;
#34528 = DIRECTION('center_axis',(-0.943883330308367,-0.330279061955168,0.)) ;
#34529 = DIRECTION('ref_axis',(0.330279061955168,-0.943883330308367,0.)) ;
#34530 = DIRECTION('center_axis',(-0.943883330308367,-0.330279061955168,0.)) ;
#34531 = DIRECTION('ref_axis',(0.330279061955168,-0.943883330308367,0.)) ;
#34532 = DIRECTION('center_axis',(0.,0.,1.)) ;
#34533 = DIRECTION('ref_axis',(1.,0.,0.)) ;
#34534 = DIRECTION('center_axis',(0.943883330308367,0.330279061955168,0.)) ;
#34535 = DIRECTION('ref_axis',(0.330279061955168,-0.943883330308367,0.)) ;
#34536 = DIRECTION('center_axis',(0.943883330308367,0.330279061955168,0.)) ;
#34537 = DIRECTION('ref_axis',(0.330279061955168,-0.943883330308367,0.)) ;
#34538 = DIRECTION('center_axis',(-0.993712209893243,-0.111964476103307,0.)) ;
#34539 = DIRECTION('ref_axis',(0.111964476103307,-0.993712209893243,0.)) ;
#34540 = DIRECTION('center_axis',(-0.993712209893243,-0.111964476103307,0.)) ;
#34541 = DIRECTION('ref_axis',(0.111964476103307,-0.993712209893243,0.)) ;
#34542 = DIRECTION('center_axis',(6.12323399573676E-17,0.,1.)) ;
#34543 = DIRECTION('ref_axis',(1.,0.,0.)) ;
#34544 = DIRECTION('center_axis',(0.993712209893243,0.111964476103307,0.)) ;
#34545 = DIRECTION('ref_axis',(0.111964476103307,-0.993712209893243,0.)) ;
#34546 = DIRECTION('center_axis',(0.993712209893243,0.111964476103307,0.)) ;
#34547 = DIRECTION('ref_axis',(0.111964476103307,-0.993712209893243,0.)) ;
#34548 = DIRECTION('center_axis',(-0.993712209893243,0.111964476103307,0.)) ;
#34549 = DIRECTION('ref_axis',(0.111964476103307,0.993712209893243,0.)) ;
#34550 = DIRECTION('center_axis',(0.,0.,1.)) ;
#34551 = DIRECTION('ref_axis',(1.,0.,0.)) ;
#34552 = DIRECTION('center_axis',(0.993712209893243,-0.111964476103307,0.)) ;
#34553 = DIRECTION('ref_axis',(0.111964476103307,0.993712209893243,0.)) ;
#34554 = DIRECTION('center_axis',(-0.943883330308367,0.330279061955168,0.)) ;
#34555 = DIRECTION('ref_axis',(0.330279061955168,0.943883330308367,0.)) ;
#34556 = DIRECTION('center_axis',(0.,0.,1.)) ;
#34557 = DIRECTION('ref_axis',(1.,0.,0.)) ;
#34558 = DIRECTION('center_axis',(0.943883330308367,-0.330279061955168,0.)) ;
#34559 = DIRECTION('ref_axis',(0.330279061955168,0.943883330308367,0.)) ;
#34560 = DIRECTION('center_axis',(-0.846724199228284,0.532032076515336,0.)) ;
#34561 = DIRECTION('ref_axis',(0.532032076515336,0.846724199228284,0.)) ;
#34562 = DIRECTION('center_axis',(0.,0.,1.)) ;
#34563 = DIRECTION('ref_axis',(1.,0.,0.)) ;
#34564 = DIRECTION('center_axis',(0.846724199228284,-0.532032076515336,0.)) ;
#34565 = DIRECTION('ref_axis',(0.532032076515336,0.846724199228284,0.)) ;
#34566 = DIRECTION('center_axis',(-0.707106781186547,0.707106781186548,0.)) ;
#34567 = DIRECTION('ref_axis',(0.707106781186548,0.707106781186547,0.)) ;
#34568 = DIRECTION('center_axis',(0.,0.,1.)) ;
#34569 = DIRECTION('ref_axis',(1.,0.,0.)) ;
#34570 = DIRECTION('center_axis',(0.707106781186547,-0.707106781186548,0.)) ;
#34571 = DIRECTION('ref_axis',(0.707106781186548,0.707106781186547,0.)) ;
#34572 = DIRECTION('center_axis',(-0.532032076515336,0.846724199228284,0.)) ;
#34573 = DIRECTION('ref_axis',(0.846724199228284,0.532032076515336,0.)) ;
#34574 = DIRECTION('center_axis',(0.,0.,1.)) ;
#34575 = DIRECTION('ref_axis',(1.,0.,0.)) ;
#34576 = DIRECTION('center_axis',(0.532032076515336,-0.846724199228284,0.)) ;
#34577 = DIRECTION('ref_axis',(0.846724199228284,0.532032076515336,0.)) ;
#34578 = DIRECTION('center_axis',(-0.330279061955168,0.943883330308367,0.)) ;
#34579 = DIRECTION('ref_axis',(0.943883330308367,0.330279061955168,0.)) ;
#34580 = DIRECTION('center_axis',(0.,0.,1.)) ;
#34581 = DIRECTION('ref_axis',(1.,0.,0.)) ;
#34582 = DIRECTION('center_axis',(0.330279061955168,-0.943883330308367,0.)) ;
#34583 = DIRECTION('ref_axis',(0.943883330308367,0.330279061955168,0.)) ;
#34584 = DIRECTION('center_axis',(-0.111964476103307,0.993712209893243,0.)) ;
#34585 = DIRECTION('ref_axis',(0.993712209893243,0.111964476103307,0.)) ;
#34586 = DIRECTION('center_axis',(0.111964476103308,0.993712209893243,0.)) ;
#34587 = DIRECTION('ref_axis',(0.993712209893243,-0.111964476103308,0.)) ;
#34588 = DIRECTION('center_axis',(1.39008514084603E-14,1.,0.)) ;
#34589 = DIRECTION('ref_axis',(1.,-1.39008514084603E-14,0.)) ;
#34590 = DIRECTION('center_axis',(1.39008514084603E-14,1.,0.)) ;
#34591 = DIRECTION('ref_axis',(1.,-1.39008514084603E-14,0.)) ;
#34592 = DIRECTION('',(-0.111964476103308,-0.993712209893243,0.)) ;
#34593 = DIRECTION('center_axis',(-0.222520933956317,-0.974927912181823,0.)) ;
#34594 = DIRECTION('ref_axis',(0.974927912181823,-0.222520933956317,0.)) ;
#34595 = DIRECTION('center_axis',(-0.222520933956317,-0.974927912181823,0.)) ;
#34596 = DIRECTION('ref_axis',(0.974927912181823,-0.222520933956317,0.)) ;
#34597 = DIRECTION('center_axis',(0.330279061955167,0.943883330308368,0.)) ;
#34598 = DIRECTION('ref_axis',(0.943883330308368,-0.330279061955167,0.)) ;
#34599 = DIRECTION('',(-0.330279061955167,-0.943883330308368,0.)) ;
#34600 = DIRECTION('center_axis',(-0.433883739117561,-0.900968867902418,0.)) ;
#34601 = DIRECTION('ref_axis',(0.900968867902418,-0.433883739117561,0.)) ;
#34602 = DIRECTION('center_axis',(-0.433883739117561,-0.900968867902418,0.)) ;
#34603 = DIRECTION('ref_axis',(0.900968867902418,-0.433883739117561,0.)) ;
#34604 = DIRECTION('center_axis',(0.532032076515336,0.846724199228284,0.)) ;
#34605 = DIRECTION('ref_axis',(0.846724199228285,-0.532032076515336,0.)) ;
#34606 = DIRECTION('',(-0.532032076515336,-0.846724199228284,0.)) ;
#34607 = DIRECTION('center_axis',(-0.623489801858739,-0.781831482468025,0.)) ;
#34608 = DIRECTION('ref_axis',(0.781831482468025,-0.623489801858739,0.)) ;
#34609 = DIRECTION('center_axis',(-0.623489801858739,-0.781831482468025,0.)) ;
#34610 = DIRECTION('ref_axis',(0.781831482468025,-0.623489801858739,0.)) ;
#34611 = DIRECTION('center_axis',(0.707106781186548,0.707106781186547,0.)) ;
#34612 = DIRECTION('ref_axis',(0.707106781186547,-0.707106781186548,0.)) ;
#34613 = DIRECTION('',(-0.707106781186548,-0.707106781186547,0.)) ;
#34614 = DIRECTION('center_axis',(-0.781831482468025,-0.623489801858739,0.)) ;
#34615 = DIRECTION('ref_axis',(0.623489801858739,-0.781831482468025,0.)) ;
#34616 = DIRECTION('center_axis',(-0.781831482468025,-0.623489801858739,0.)) ;
#34617 = DIRECTION('ref_axis',(0.623489801858739,-0.781831482468025,0.)) ;
#34618 = DIRECTION('center_axis',(0.846724199228284,0.532032076515337,0.)) ;
#34619 = DIRECTION('ref_axis',(0.532032076515337,-0.846724199228284,0.)) ;
#34620 = DIRECTION('',(-0.846724199228284,-0.532032076515337,0.)) ;
#34621 = DIRECTION('center_axis',(-0.900968867902421,-0.433883739117553,0.)) ;
#34622 = DIRECTION('ref_axis',(0.433883739117553,-0.900968867902422,0.)) ;
#34623 = DIRECTION('center_axis',(-0.900968867902421,-0.433883739117553,0.)) ;
#34624 = DIRECTION('ref_axis',(0.433883739117553,-0.900968867902422,0.)) ;
#34625 = DIRECTION('center_axis',(0.943883330308368,0.330279061955166,0.)) ;
#34626 = DIRECTION('ref_axis',(0.330279061955166,-0.943883330308368,0.)) ;
#34627 = DIRECTION('',(-0.943883330308368,-0.330279061955166,0.)) ;
#34628 = DIRECTION('center_axis',(-0.974927912181825,-0.222520933956307,0.)) ;
#34629 = DIRECTION('ref_axis',(0.222520933956307,-0.974927912181825,0.)) ;
#34630 = DIRECTION('center_axis',(-0.974927912181825,-0.222520933956307,0.)) ;
#34631 = DIRECTION('ref_axis',(0.222520933956307,-0.974927912181825,0.)) ;
#34632 = DIRECTION('center_axis',(0.993712209893243,0.111964476103307,0.)) ;
#34633 = DIRECTION('ref_axis',(0.111964476103307,-0.993712209893243,0.)) ;
#34634 = DIRECTION('',(-0.993712209893243,-0.111964476103307,0.)) ;
#34635 = DIRECTION('center_axis',(-1.,1.19150154929659E-14,0.)) ;
#34636 = DIRECTION('ref_axis',(-1.19150154929659E-14,-1.,0.)) ;
#34637 = DIRECTION('center_axis',(-1.,1.19150154929659E-14,0.)) ;
#34638 = DIRECTION('ref_axis',(-1.19150154929659E-14,-1.,0.)) ;
#34639 = DIRECTION('center_axis',(0.993712209893243,-0.111964476103307,0.)) ;
#34640 = DIRECTION('ref_axis',(0.111964476103307,0.993712209893243,0.)) ;
#34641 = DIRECTION('',(-0.993712209893243,0.111964476103307,0.)) ;
#34642 = DIRECTION('center_axis',(-0.974927912181822,0.22252093395632,0.)) ;
#34643 = DIRECTION('ref_axis',(0.22252093395632,0.974927912181822,0.)) ;
#34644 = DIRECTION('center_axis',(0.943883330308367,-0.330279061955168,0.)) ;
#34645 = DIRECTION('ref_axis',(0.330279061955168,0.943883330308367,0.)) ;
#34646 = DIRECTION('',(-0.943883330308367,0.330279061955168,0.)) ;
#34647 = DIRECTION('center_axis',(-0.900968867902414,0.433883739117568,0.)) ;
#34648 = DIRECTION('ref_axis',(0.433883739117568,0.900968867902414,0.)) ;
#34649 = DIRECTION('center_axis',(0.846724199228284,-0.532032076515337,0.)) ;
#34650 = DIRECTION('ref_axis',(0.532032076515337,0.846724199228284,0.)) ;
#34651 = DIRECTION('',(-0.846724199228284,0.532032076515337,0.)) ;
#34652 = DIRECTION('center_axis',(-0.781831482468023,0.623489801858742,0.)) ;
#34653 = DIRECTION('ref_axis',(0.623489801858742,0.781831482468023,0.)) ;
#34654 = DIRECTION('center_axis',(0.707106781186548,-0.707106781186547,0.)) ;
#34655 = DIRECTION('ref_axis',(0.707106781186547,0.707106781186548,0.)) ;
#34656 = DIRECTION('',(-0.707106781186548,0.707106781186547,0.)) ;
#34657 = DIRECTION('center_axis',(-0.62348980185874,0.781831482468024,0.)) ;
#34658 = DIRECTION('ref_axis',(0.781831482468024,0.62348980185874,0.)) ;
#34659 = DIRECTION('center_axis',(0.532032076515336,-0.846724199228284,0.)) ;
#34660 = DIRECTION('ref_axis',(0.846724199228284,0.532032076515336,0.)) ;
#34661 = DIRECTION('',(-0.532032076515336,0.846724199228284,0.)) ;
#34662 = DIRECTION('center_axis',(-0.433883739117548,0.900968867902424,0.)) ;
#34663 = DIRECTION('ref_axis',(0.900968867902424,0.433883739117548,0.)) ;
#34664 = DIRECTION('center_axis',(0.330279061955167,-0.943883330308368,0.)) ;
#34665 = DIRECTION('ref_axis',(0.943883330308368,0.330279061955167,0.)) ;
#34666 = DIRECTION('',(-0.330279061955167,0.943883330308368,0.)) ;
#34667 = DIRECTION('center_axis',(-0.222520933956297,0.974927912181828,0.)) ;
#34668 = DIRECTION('ref_axis',(0.974927912181828,0.222520933956297,0.)) ;
#34669 = DIRECTION('center_axis',(0.111964476103307,-0.993712209893243,0.)) ;
#34670 = DIRECTION('ref_axis',(0.993712209893243,0.111964476103307,0.)) ;
#34671 = DIRECTION('',(-0.111964476103307,0.993712209893243,0.)) ;
#34672 = DIRECTION('center_axis',(1.14737186228561E-14,1.,0.)) ;
#34673 = DIRECTION('ref_axis',(1.,-1.1487509150047E-14,0.)) ;
#34674 = DIRECTION('center_axis',(-0.111964476103307,-0.993712209893243,0.)) ;
#34675 = DIRECTION('ref_axis',(0.993712209893243,-0.111964476103307,0.)) ;
#34676 = DIRECTION('',(0.111964476103307,0.993712209893243,0.)) ;
#34677 = DIRECTION('center_axis',(0.22252093395631,0.974927912181825,0.)) ;
#34678 = DIRECTION('ref_axis',(0.974927912181825,-0.22252093395631,0.)) ;
#34679 = DIRECTION('center_axis',(-0.330279061955167,-0.943883330308367,0.)) ;
#34680 = DIRECTION('ref_axis',(0.943883330308368,-0.330279061955167,0.)) ;
#34681 = DIRECTION('',(0.330279061955167,0.943883330308367,0.)) ;
#34682 = DIRECTION('center_axis',(0.433883739117568,0.900968867902414,0.)) ;
#34683 = DIRECTION('ref_axis',(0.900968867902414,-0.433883739117568,0.)) ;
#34684 = DIRECTION('center_axis',(-0.532032076515337,-0.846724199228284,0.)) ;
#34685 = DIRECTION('ref_axis',(0.846724199228284,-0.532032076515337,0.)) ;
#34686 = DIRECTION('',(0.532032076515337,0.846724199228284,0.)) ;
#34687 = DIRECTION('center_axis',(0.623489801858745,0.78183148246802,0.)) ;
#34688 = DIRECTION('ref_axis',(0.78183148246802,-0.623489801858745,0.)) ;
#34689 = DIRECTION('center_axis',(-0.707106781186548,-0.707106781186548,0.)) ;
#34690 = DIRECTION('ref_axis',(0.707106781186548,-0.707106781186548,0.)) ;
#34691 = DIRECTION('',(0.707106781186548,0.707106781186548,0.)) ;
#34692 = DIRECTION('center_axis',(0.781831482468033,0.623489801858729,0.)) ;
#34693 = DIRECTION('ref_axis',(0.623489801858729,-0.781831482468033,0.)) ;
#34694 = DIRECTION('center_axis',(-0.846724199228285,-0.532032076515336,0.)) ;
#34695 = DIRECTION('ref_axis',(0.532032076515336,-0.846724199228285,0.)) ;
#34696 = DIRECTION('',(0.846724199228285,0.532032076515336,0.)) ;
#34697 = DIRECTION('center_axis',(0.900968867902424,0.433883739117548,0.)) ;
#34698 = DIRECTION('ref_axis',(0.433883739117548,-0.900968867902424,0.)) ;
#34699 = DIRECTION('center_axis',(-0.943883330308367,-0.330279061955168,0.)) ;
#34700 = DIRECTION('ref_axis',(0.330279061955168,-0.943883330308367,0.)) ;
#34701 = DIRECTION('',(0.943883330308367,0.330279061955168,0.)) ;
#34702 = DIRECTION('center_axis',(0.974927912181826,0.222520933956302,0.)) ;
#34703 = DIRECTION('ref_axis',(0.222520933956302,-0.974927912181826,0.)) ;
#34704 = DIRECTION('center_axis',(-0.993712209893243,-0.111964476103307,0.)) ;
#34705 = DIRECTION('ref_axis',(0.111964476103307,-0.993712209893243,0.)) ;
#34706 = DIRECTION('',(0.993712209893243,0.111964476103307,0.)) ;
#34707 = DIRECTION('center_axis',(1.,-1.34595545383504E-14,0.)) ;
#34708 = DIRECTION('ref_axis',(-1.34733450655413E-14,-1.,0.)) ;
#34709 = DIRECTION('center_axis',(1.,-1.34595545383504E-14,0.)) ;
#34710 = DIRECTION('ref_axis',(-1.34733450655413E-14,-1.,0.)) ;
#34711 = DIRECTION('center_axis',(-0.993712209893243,0.111964476103307,0.)) ;
#34712 = DIRECTION('ref_axis',(0.111964476103307,0.993712209893243,0.)) ;
#34713 = DIRECTION('',(0.993712209893243,-0.111964476103307,0.)) ;
#34714 = DIRECTION('center_axis',(0.974927912181822,-0.222520933956322,0.)) ;
#34715 = DIRECTION('ref_axis',(0.222520933956322,0.974927912181822,0.)) ;
#34716 = DIRECTION('center_axis',(0.974927912181822,-0.222520933956322,0.)) ;
#34717 = DIRECTION('ref_axis',(0.222520933956322,0.974927912181822,0.)) ;
#34718 = DIRECTION('center_axis',(-0.943883330308367,0.330279061955168,0.)) ;
#34719 = DIRECTION('ref_axis',(0.330279061955168,0.943883330308367,0.)) ;
#34720 = DIRECTION('',(0.943883330308367,-0.330279061955168,0.)) ;
#34721 = DIRECTION('center_axis',(0.900968867902422,-0.433883739117553,0.)) ;
#34722 = DIRECTION('ref_axis',(0.433883739117553,0.900968867902422,0.)) ;
#34723 = DIRECTION('center_axis',(0.900968867902422,-0.433883739117553,0.)) ;
#34724 = DIRECTION('ref_axis',(0.433883739117553,0.900968867902422,0.)) ;
#34725 = DIRECTION('center_axis',(-0.846724199228284,0.532032076515336,0.)) ;
#34726 = DIRECTION('ref_axis',(0.532032076515336,0.846724199228284,0.)) ;
#34727 = DIRECTION('',(0.846724199228284,-0.532032076515336,0.)) ;
#34728 = DIRECTION('center_axis',(0.781831482468019,-0.623489801858747,0.)) ;
#34729 = DIRECTION('ref_axis',(0.623489801858747,0.781831482468019,0.)) ;
#34730 = DIRECTION('center_axis',(0.781831482468019,-0.623489801858747,0.)) ;
#34731 = DIRECTION('ref_axis',(0.623489801858747,0.781831482468019,0.)) ;
#34732 = DIRECTION('center_axis',(-0.707106781186547,0.707106781186548,0.)) ;
#34733 = DIRECTION('ref_axis',(0.707106781186548,0.707106781186547,0.)) ;
#34734 = DIRECTION('',(0.707106781186547,-0.707106781186548,0.)) ;
#34735 = DIRECTION('center_axis',(0.623489801858735,-0.781831482468028,0.)) ;
#34736 = DIRECTION('ref_axis',(0.781831482468028,0.623489801858735,0.)) ;
#34737 = DIRECTION('center_axis',(0.623489801858735,-0.781831482468028,0.)) ;
#34738 = DIRECTION('ref_axis',(0.781831482468028,0.623489801858735,0.)) ;
#34739 = DIRECTION('center_axis',(-0.532032076515336,0.846724199228284,0.)) ;
#34740 = DIRECTION('ref_axis',(0.846724199228284,0.532032076515336,0.)) ;
#34741 = DIRECTION('',(0.532032076515336,-0.846724199228284,0.)) ;
#34742 = DIRECTION('center_axis',(0.433883739117553,-0.900968867902422,0.)) ;
#34743 = DIRECTION('ref_axis',(0.900968867902422,0.433883739117553,0.)) ;
#34744 = DIRECTION('center_axis',(0.433883739117553,-0.900968867902422,0.)) ;
#34745 = DIRECTION('ref_axis',(0.900968867902422,0.433883739117553,0.)) ;
#34746 = DIRECTION('center_axis',(-0.330279061955168,0.943883330308367,0.)) ;
#34747 = DIRECTION('ref_axis',(0.943883330308367,0.330279061955168,0.)) ;
#34748 = DIRECTION('',(0.330279061955168,-0.943883330308367,0.)) ;
#34749 = DIRECTION('center_axis',(0.222520933956303,-0.974927912181826,0.)) ;
#34750 = DIRECTION('ref_axis',(0.974927912181826,0.222520933956303,0.)) ;
#34751 = DIRECTION('center_axis',(0.222520933956303,-0.974927912181826,0.)) ;
#34752 = DIRECTION('ref_axis',(0.974927912181826,0.222520933956303,0.)) ;
#34753 = DIRECTION('center_axis',(-0.111964476103307,0.993712209893243,0.)) ;
#34754 = DIRECTION('ref_axis',(0.993712209893243,0.111964476103307,0.)) ;
#34755 = DIRECTION('',(0.111964476103307,-0.993712209893243,0.)) ;
#34756 = DIRECTION('',(0.,0.,1.)) ;
#34757 = DIRECTION('',(1.,0.,0.)) ;
#34758 = DIRECTION('',(0.,0.,1.)) ;
#34759 = DIRECTION('',(1.,0.,0.)) ;
#34760 = DIRECTION('',(0.,0.,1.)) ;
#34761 = DIRECTION('',(1.,0.,0.)) ;
#34762 = DIRECTION('',(0.,0.,1.)) ;
#34763 = DIRECTION('',(1.,0.,0.)) ;
#34764 = DIRECTION('',(0.,0.,1.)) ;
#34765 = DIRECTION('',(1.,0.,0.)) ;
#34766 = DIRECTION('',(0.,0.,1.)) ;
#34767 = DIRECTION('',(1.,0.,0.)) ;
#34768 = DIRECTION('axis',(0.,0.,1.)) ;
#34769 = DIRECTION('refdir',(1.,0.,0.)) ;
#34770 = DIRECTION('axis',(0.,0.,1.)) ;
#34771 = DIRECTION('refdir',(1.,0.,0.)) ;
#34772 = DIRECTION('center_axis',(0.,0.,1.)) ;
#34773 = DIRECTION('ref_axis',(1.,0.,0.)) ;
#34774 = DIRECTION('center_axis',(0.,0.,1.)) ;
#34775 = DIRECTION('ref_axis',(1.,0.,0.)) ;
#34776 = DIRECTION('',(0.,0.,1.)) ;
#34777 = DIRECTION('center_axis',(0.,0.,-1.)) ;
#34778 = DIRECTION('ref_axis',(1.,0.,0.)) ;
#34779 = DIRECTION('center_axis',(0.,0.,1.)) ;
#34780 = DIRECTION('ref_axis',(1.,0.,0.)) ;
#34781 = DIRECTION('center_axis',(0.,0.,1.)) ;
#34782 = DIRECTION('ref_axis',(1.,0.,0.)) ;
#34783 = DIRECTION('',(0.,0.,1.)) ;
#34784 = DIRECTION('center_axis',(0.,0.,-1.)) ;
#34785 = DIRECTION('ref_axis',(1.,0.,0.)) ;
#34786 = DIRECTION('center_axis',(0.,0.,1.)) ;
#34787 = DIRECTION('ref_axis',(1.,0.,0.)) ;
#34788 = DIRECTION('center_axis',(0.,0.,1.)) ;
#34789 = DIRECTION('ref_axis',(1.,0.,0.)) ;
#34790 = DIRECTION('',(0.,0.,1.)) ;
#34791 = DIRECTION('center_axis',(0.,0.,-1.)) ;
#34792 = DIRECTION('ref_axis',(1.,0.,0.)) ;
#34793 = DIRECTION('center_axis',(0.,0.,1.)) ;
#34794 = DIRECTION('ref_axis',(1.,0.,0.)) ;
#34795 = DIRECTION('center_axis',(0.,0.,1.)) ;
#34796 = DIRECTION('ref_axis',(1.,0.,0.)) ;
#34797 = DIRECTION('',(0.,0.,1.)) ;
#34798 = DIRECTION('center_axis',(0.,0.,-1.)) ;
#34799 = DIRECTION('ref_axis',(1.,0.,0.)) ;
#34800 = DIRECTION('center_axis',(0.,0.,1.)) ;
#34801 = DIRECTION('ref_axis',(1.,0.,0.)) ;
#34802 = DIRECTION('center_axis',(0.,0.,1.)) ;
#34803 = DIRECTION('ref_axis',(1.,0.,0.)) ;
#34804 = DIRECTION('',(0.,0.,1.)) ;
#34805 = DIRECTION('center_axis',(0.,0.,-1.)) ;
#34806 = DIRECTION('ref_axis',(1.,0.,0.)) ;
#34807 = DIRECTION('center_axis',(0.,0.,1.)) ;
#34808 = DIRECTION('ref_axis',(1.,0.,0.)) ;
#34809 = DIRECTION('center_axis',(0.,0.,1.)) ;
#34810 = DIRECTION('ref_axis',(1.,0.,0.)) ;
#34811 = DIRECTION('',(0.,0.,1.)) ;
#34812 = DIRECTION('center_axis',(0.,0.,-1.)) ;
#34813 = DIRECTION('ref_axis',(1.,0.,0.)) ;
#34814 = DIRECTION('center_axis',(0.,1.,0.)) ;
#34815 = DIRECTION('ref_axis',(1.,0.,0.)) ;
#34816 = DIRECTION('',(0.,-1.,0.)) ;
#34817 = DIRECTION('center_axis',(0.,1.,0.)) ;
#34818 = DIRECTION('ref_axis',(1.,0.,0.)) ;
#34819 = DIRECTION('',(0.,1.,0.)) ;
#34820 = DIRECTION('center_axis',(0.,-1.,0.)) ;
#34821 = DIRECTION('ref_axis',(1.,0.,0.)) ;
#34822 = DIRECTION('center_axis',(-1.,0.,0.)) ;
#34823 = DIRECTION('ref_axis',(0.,0.,1.)) ;
#34824 = DIRECTION('',(0.,0.,-1.)) ;
#34825 = DIRECTION('',(0.,1.,0.)) ;
#34826 = DIRECTION('',(0.,0.,-1.)) ;
#34827 = DIRECTION('',(0.,-1.,0.)) ;
#34828 = DIRECTION('center_axis',(0.,-1.,0.)) ;
#34829 = DIRECTION('ref_axis',(0.,0.,-1.)) ;
#34830 = DIRECTION('',(1.,0.,0.)) ;
#34831 = DIRECTION('',(-1.,0.,0.)) ;
#34832 = DIRECTION('',(0.,0.,-1.)) ;
#34833 = DIRECTION('',(1.,0.,0.)) ;
#34834 = DIRECTION('center_axis',(1.,0.,0.)) ;
#34835 = DIRECTION('ref_axis',(0.,0.,-1.)) ;
#34836 = DIRECTION('',(0.,-1.,0.)) ;
#34837 = DIRECTION('',(0.,0.,-1.)) ;
#34838 = DIRECTION('',(0.,1.,0.)) ;
#34839 = DIRECTION('center_axis',(0.,0.,1.)) ;
#34840 = DIRECTION('ref_axis',(1.,0.,0.)) ;
#34841 = DIRECTION('',(-1.,0.,0.)) ;
#34842 = DIRECTION('center_axis',(0.,0.,1.)) ;
#34843 = DIRECTION('ref_axis',(1.,0.,0.)) ;
#34844 = DIRECTION('',(1.,0.,0.)) ;
#34845 = DIRECTION('center_axis',(0.,0.,1.)) ;
#34846 = DIRECTION('ref_axis',(1.,0.,0.)) ;
#34847 = DIRECTION('',(-1.,0.,0.)) ;
#34848 = DIRECTION('center_axis',(0.,1.,0.)) ;
#34849 = DIRECTION('ref_axis',(0.,0.,1.)) ;
#34850 = DIRECTION('center_axis',(0.,0.,1.)) ;
#34851 = DIRECTION('ref_axis',(1.,0.,0.)) ;
#34852 = DIRECTION('center_axis',(0.,0.,1.)) ;
#34853 = DIRECTION('ref_axis',(1.,0.,0.)) ;
#34854 = DIRECTION('',(0.,0.,1.)) ;
#34855 = DIRECTION('center_axis',(0.,0.,-1.)) ;
#34856 = DIRECTION('ref_axis',(1.,0.,0.)) ;
#34857 = DIRECTION('center_axis',(0.,0.,1.)) ;
#34858 = DIRECTION('ref_axis',(1.,0.,0.)) ;
#34859 = DIRECTION('center_axis',(0.,0.,1.)) ;
#34860 = DIRECTION('ref_axis',(1.,0.,0.)) ;
#34861 = DIRECTION('',(0.,0.,1.)) ;
#34862 = DIRECTION('center_axis',(0.,0.,-1.)) ;
#34863 = DIRECTION('ref_axis',(1.,0.,0.)) ;
#34864 = DIRECTION('center_axis',(0.,1.,0.)) ;
#34865 = DIRECTION('ref_axis',(1.,0.,0.)) ;
#34866 = DIRECTION('',(0.,-1.,0.)) ;
#34867 = DIRECTION('center_axis',(0.,1.,0.)) ;
#34868 = DIRECTION('ref_axis',(1.,0.,0.)) ;
#34869 = DIRECTION('',(0.,1.,0.)) ;
#34870 = DIRECTION('center_axis',(0.,-1.,0.)) ;
#34871 = DIRECTION('ref_axis',(1.,0.,0.)) ;
#34872 = DIRECTION('center_axis',(-1.,0.,0.)) ;
#34873 = DIRECTION('ref_axis',(0.,0.,1.)) ;
#34874 = DIRECTION('',(0.,0.,-1.)) ;
#34875 = DIRECTION('',(0.,1.,0.)) ;
#34876 = DIRECTION('',(0.,0.,-1.)) ;
#34877 = DIRECTION('',(0.,-1.,0.)) ;
#34878 = DIRECTION('center_axis',(0.,-1.,0.)) ;
#34879 = DIRECTION('ref_axis',(0.,0.,-1.)) ;
#34880 = DIRECTION('',(1.,0.,0.)) ;
#34881 = DIRECTION('',(-1.,0.,0.)) ;
#34882 = DIRECTION('',(0.,0.,-1.)) ;
#34883 = DIRECTION('',(1.,0.,0.)) ;
#34884 = DIRECTION('center_axis',(1.,0.,0.)) ;
#34885 = DIRECTION('ref_axis',(0.,0.,-1.)) ;
#34886 = DIRECTION('',(0.,-1.,0.)) ;
#34887 = DIRECTION('',(0.,0.,-1.)) ;
#34888 = DIRECTION('',(0.,1.,0.)) ;
#34889 = DIRECTION('center_axis',(0.,0.,1.)) ;
#34890 = DIRECTION('ref_axis',(1.,0.,0.)) ;
#34891 = DIRECTION('',(-1.,0.,0.)) ;
#34892 = DIRECTION('center_axis',(0.,0.,1.)) ;
#34893 = DIRECTION('ref_axis',(1.,0.,0.)) ;
#34894 = DIRECTION('',(1.,0.,0.)) ;
#34895 = DIRECTION('center_axis',(0.,0.,1.)) ;
#34896 = DIRECTION('ref_axis',(1.,0.,0.)) ;
#34897 = DIRECTION('',(-1.,0.,0.)) ;
#34898 = DIRECTION('center_axis',(0.,1.,0.)) ;
#34899 = DIRECTION('ref_axis',(0.,0.,1.)) ;
#34900 = DIRECTION('center_axis',(0.,1.,0.)) ;
#34901 = DIRECTION('ref_axis',(1.,0.,0.)) ;
#34902 = DIRECTION('center_axis',(0.,1.,0.)) ;
#34903 = DIRECTION('ref_axis',(1.,0.,0.)) ;
#34904 = DIRECTION('',(0.,1.,0.)) ;
#34905 = DIRECTION('center_axis',(0.,-1.,0.)) ;
#34906 = DIRECTION('ref_axis',(1.,0.,0.)) ;
#34907 = DIRECTION('center_axis',(0.,1.,0.)) ;
#34908 = DIRECTION('ref_axis',(1.,0.,0.)) ;
#34909 = DIRECTION('center_axis',(0.,1.,0.)) ;
#34910 = DIRECTION('ref_axis',(1.,0.,0.)) ;
#34911 = DIRECTION('',(0.,1.,0.)) ;
#34912 = DIRECTION('center_axis',(0.,-1.,0.)) ;
#34913 = DIRECTION('ref_axis',(1.,0.,0.)) ;
#34914 = DIRECTION('center_axis',(0.,0.,1.)) ;
#34915 = DIRECTION('ref_axis',(1.,0.,0.)) ;
#34916 = DIRECTION('center_axis',(0.,0.,1.)) ;
#34917 = DIRECTION('ref_axis',(1.,0.,0.)) ;
#34918 = DIRECTION('',(0.,0.,1.)) ;
#34919 = DIRECTION('center_axis',(0.,0.,-1.)) ;
#34920 = DIRECTION('ref_axis',(1.,0.,0.)) ;
#34921 = DIRECTION('center_axis',(0.,0.,1.)) ;
#34922 = DIRECTION('ref_axis',(1.,0.,0.)) ;
#34923 = DIRECTION('center_axis',(0.,0.,1.)) ;
#34924 = DIRECTION('ref_axis',(1.,0.,0.)) ;
#34925 = DIRECTION('',(0.,0.,-1.)) ;
#34926 = DIRECTION('center_axis',(0.,0.,-1.)) ;
#34927 = DIRECTION('ref_axis',(1.,0.,0.)) ;
#34928 = DIRECTION('center_axis',(0.,0.,1.)) ;
#34929 = DIRECTION('ref_axis',(1.,0.,0.)) ;
#34930 = DIRECTION('center_axis',(0.,0.,1.)) ;
#34931 = DIRECTION('ref_axis',(1.,0.,0.)) ;
#34932 = DIRECTION('',(0.,1.,0.)) ;
#34933 = DIRECTION('',(-1.,0.,0.)) ;
#34934 = DIRECTION('',(0.,-1.,0.)) ;
#34935 = DIRECTION('',(-1.,0.,0.)) ;
#34936 = DIRECTION('',(1.,0.,0.)) ;
#34937 = DIRECTION('center_axis',(0.,0.,-1.)) ;
#34938 = DIRECTION('ref_axis',(1.,0.,0.)) ;
#34939 = DIRECTION('center_axis',(0.,0.,1.)) ;
#34940 = DIRECTION('ref_axis',(1.,0.,0.)) ;
#34941 = DIRECTION('center_axis',(0.,0.,1.)) ;
#34942 = DIRECTION('ref_axis',(1.,0.,0.)) ;
#34943 = DIRECTION('',(0.,0.,1.)) ;
#34944 = DIRECTION('center_axis',(0.,0.,-1.)) ;
#34945 = DIRECTION('ref_axis',(1.,0.,0.)) ;
#34946 = DIRECTION('center_axis',(0.,0.,1.)) ;
#34947 = DIRECTION('ref_axis',(1.,0.,0.)) ;
#34948 = DIRECTION('center_axis',(0.,0.,1.)) ;
#34949 = DIRECTION('ref_axis',(1.,0.,0.)) ;
#34950 = DIRECTION('',(0.,0.,-1.)) ;
#34951 = DIRECTION('center_axis',(0.,0.,1.)) ;
#34952 = DIRECTION('ref_axis',(1.,0.,0.)) ;
#34953 = DIRECTION('center_axis',(0.,0.,1.)) ;
#34954 = DIRECTION('ref_axis',(1.,0.,0.)) ;
#34955 = DIRECTION('center_axis',(0.,-1.,0.)) ;
#34956 = DIRECTION('ref_axis',(0.,0.,-1.)) ;
#34957 = DIRECTION('',(1.,0.,0.)) ;
#34958 = DIRECTION('',(0.,0.,-1.)) ;
#34959 = DIRECTION('',(-1.,0.,0.)) ;
#34960 = DIRECTION('',(0.,0.,-1.)) ;
#34961 = DIRECTION('center_axis',(-1.,0.,0.)) ;
#34962 = DIRECTION('ref_axis',(0.,0.,1.)) ;
#34963 = DIRECTION('',(0.,-1.,0.)) ;
#34964 = DIRECTION('',(0.,1.,0.)) ;
#34965 = DIRECTION('',(0.,0.,-1.)) ;
#34966 = DIRECTION('center_axis',(0.,1.,0.)) ;
#34967 = DIRECTION('ref_axis',(0.,0.,1.)) ;
#34968 = DIRECTION('',(-1.,0.,0.)) ;
#34969 = DIRECTION('',(1.,0.,0.)) ;
#34970 = DIRECTION('',(0.,0.,-1.)) ;
#34971 = DIRECTION('center_axis',(1.,0.,0.)) ;
#34972 = DIRECTION('ref_axis',(0.,0.,-1.)) ;
#34973 = DIRECTION('',(0.,1.,0.)) ;
#34974 = DIRECTION('',(0.,-1.,0.)) ;
#34975 = DIRECTION('center_axis',(0.,0.,1.)) ;
#34976 = DIRECTION('ref_axis',(1.,0.,0.)) ;
#34977 = DIRECTION('',(0.,-1.,0.)) ;
#34978 = DIRECTION('',(-1.,0.,0.)) ;
#34979 = DIRECTION('',(0.,1.,0.)) ;
#34980 = DIRECTION('',(1.,0.,0.)) ;
#34981 = DIRECTION('center_axis',(1.,0.,0.)) ;
#34982 = DIRECTION('ref_axis',(0.,0.,-1.)) ;
#34983 = DIRECTION('',(0.,0.,-1.)) ;
#34984 = DIRECTION('',(0.,0.,-1.)) ;
#34985 = DIRECTION('',(0.,-1.,0.)) ;
#34986 = DIRECTION('center_axis',(-1.,0.,0.)) ;
#34987 = DIRECTION('ref_axis',(0.,0.,1.)) ;
#34988 = DIRECTION('',(0.,0.,-1.)) ;
#34989 = DIRECTION('',(0.,0.,-1.)) ;
#34990 = DIRECTION('',(0.,1.,0.)) ;
#34991 = DIRECTION('center_axis',(0.,0.,1.)) ;
#34992 = DIRECTION('ref_axis',(1.,0.,0.)) ;
#34993 = DIRECTION('',(-1.,0.,0.)) ;
#34994 = DIRECTION('',(1.,0.,0.)) ;
#34995 = DIRECTION('',(0.,-1.,0.)) ;
#34996 = DIRECTION('',(1.,0.,0.)) ;
#34997 = DIRECTION('center_axis',(0.,0.,1.)) ;
#34998 = DIRECTION('ref_axis',(1.,0.,0.)) ;
#34999 = DIRECTION('center_axis',(0.,0.,1.)) ;
#35000 = DIRECTION('ref_axis',(1.,0.,0.)) ;
#35001 = DIRECTION('',(0.,1.,0.)) ;
#35002 = DIRECTION('',(-1.,0.,0.)) ;
#35003 = DIRECTION('',(0.,1.,0.)) ;
#35004 = DIRECTION('',(-1.,0.,0.)) ;
#35005 = DIRECTION('center_axis',(0.,0.,1.)) ;
#35006 = DIRECTION('ref_axis',(1.,0.,0.)) ;
#35007 = DIRECTION('center_axis',(0.,0.,1.)) ;
#35008 = DIRECTION('ref_axis',(1.,0.,0.)) ;
#35009 = DIRECTION('center_axis',(0.,0.,1.)) ;
#35010 = DIRECTION('ref_axis',(1.,0.,0.)) ;
#35011 = DIRECTION('',(0.,1.,0.)) ;
#35012 = DIRECTION('',(1.,0.,0.)) ;
#35013 = DIRECTION('',(0.,-1.,0.)) ;
#35014 = DIRECTION('',(-1.,0.,0.)) ;
#35015 = DIRECTION('center_axis',(0.,1.,0.)) ;
#35016 = DIRECTION('ref_axis',(0.,0.,1.)) ;
#35017 = DIRECTION('center_axis',(0.,-1.,0.)) ;
#35018 = DIRECTION('ref_axis',(1.,0.,0.)) ;
#35019 = DIRECTION('',(-1.,0.,0.)) ;
#35020 = DIRECTION('',(0.,0.,-1.)) ;
#35021 = DIRECTION('',(-1.,0.,0.)) ;
#35022 = DIRECTION('',(0.,0.,-1.)) ;
#35023 = DIRECTION('',(0.,0.,-1.)) ;
#35024 = DIRECTION('',(1.,0.,0.)) ;
#35025 = DIRECTION('',(0.,0.,-1.)) ;
#35026 = DIRECTION('center_axis',(0.,-1.,0.)) ;
#35027 = DIRECTION('ref_axis',(0.,0.,-1.)) ;
#35028 = DIRECTION('',(0.,0.,-1.)) ;
#35029 = DIRECTION('',(-1.,0.,0.)) ;
#35030 = DIRECTION('',(0.,0.,-1.)) ;
#35031 = DIRECTION('',(0.,0.,-1.)) ;
#35032 = DIRECTION('',(1.,0.,0.)) ;
#35033 = DIRECTION('',(0.,0.,-1.)) ;
#35034 = DIRECTION('',(1.,0.,0.)) ;
#35035 = DIRECTION('center_axis',(-1.,0.,0.)) ;
#35036 = DIRECTION('ref_axis',(0.,0.,1.)) ;
#35037 = DIRECTION('',(0.,1.,0.)) ;
#35038 = DIRECTION('center_axis',(0.,1.,0.)) ;
#35039 = DIRECTION('ref_axis',(0.,0.,1.)) ;
#35040 = DIRECTION('',(-1.,0.,0.)) ;
#35041 = DIRECTION('center_axis',(0.,1.,0.)) ;
#35042 = DIRECTION('ref_axis',(1.,0.,0.)) ;
#35043 = DIRECTION('',(1.,0.,0.)) ;
#35044 = DIRECTION('',(0.,0.,-1.)) ;
#35045 = DIRECTION('center_axis',(0.,1.,0.)) ;
#35046 = DIRECTION('ref_axis',(0.,0.,1.)) ;
#35047 = DIRECTION('',(0.,0.,-1.)) ;
#35048 = DIRECTION('',(1.,0.,0.)) ;
#35049 = DIRECTION('center_axis',(0.,1.,0.)) ;
#35050 = DIRECTION('ref_axis',(1.,0.,0.)) ;
#35051 = DIRECTION('center_axis',(0.,0.,1.)) ;
#35052 = DIRECTION('ref_axis',(1.,0.,0.)) ;
#35053 = DIRECTION('',(0.,1.,0.)) ;
#35054 = DIRECTION('',(-1.,0.,0.)) ;
#35055 = DIRECTION('',(0.,1.,0.)) ;
#35056 = DIRECTION('center_axis',(0.,0.,1.)) ;
#35057 = DIRECTION('ref_axis',(1.,0.,0.)) ;
#35058 = DIRECTION('',(-1.,0.,0.)) ;
#35059 = DIRECTION('',(0.,1.,0.)) ;
#35060 = DIRECTION('',(1.,0.,0.)) ;
#35061 = DIRECTION('',(0.,-1.,0.)) ;
#35062 = DIRECTION('center_axis',(0.,0.,1.)) ;
#35063 = DIRECTION('ref_axis',(1.,0.,0.)) ;
#35064 = DIRECTION('',(-1.,0.,0.)) ;
#35065 = DIRECTION('',(0.,1.,0.)) ;
#35066 = DIRECTION('',(1.,0.,0.)) ;
#35067 = DIRECTION('',(0.,-1.,0.)) ;
#35068 = DIRECTION('center_axis',(0.,0.,1.)) ;
#35069 = DIRECTION('ref_axis',(1.,0.,0.)) ;
#35070 = DIRECTION('',(-1.,0.,0.)) ;
#35071 = DIRECTION('',(0.,-1.,0.)) ;
#35072 = DIRECTION('',(1.,0.,0.)) ;
#35073 = DIRECTION('',(0.,1.,0.)) ;
#35074 = DIRECTION('center_axis',(0.,0.,1.)) ;
#35075 = DIRECTION('ref_axis',(1.,0.,0.)) ;
#35076 = DIRECTION('',(0.,-1.,0.)) ;
#35077 = DIRECTION('',(-1.,0.,0.)) ;
#35078 = DIRECTION('',(0.,-1.,0.)) ;
#35079 = DIRECTION('center_axis',(0.,-1.,0.)) ;
#35080 = DIRECTION('ref_axis',(0.,0.,-1.)) ;
#35081 = DIRECTION('',(0.,0.,-1.)) ;
#35082 = DIRECTION('',(-1.,0.,0.)) ;
#35083 = DIRECTION('',(0.,0.,-1.)) ;
#35084 = DIRECTION('center_axis',(0.,-1.,0.)) ;
#35085 = DIRECTION('ref_axis',(1.,0.,0.)) ;
#35086 = DIRECTION('center_axis',(0.,-1.,0.)) ;
#35087 = DIRECTION('ref_axis',(0.,0.,-1.)) ;
#35088 = DIRECTION('',(0.,0.,-1.)) ;
#35089 = DIRECTION('',(1.,0.,0.)) ;
#35090 = DIRECTION('',(0.,0.,-1.)) ;
#35091 = DIRECTION('center_axis',(0.,-1.,0.)) ;
#35092 = DIRECTION('ref_axis',(1.,0.,0.)) ;
#35093 = DIRECTION('center_axis',(1.,0.,0.)) ;
#35094 = DIRECTION('ref_axis',(0.,0.,-1.)) ;
#35095 = DIRECTION('',(0.,0.,1.)) ;
#35096 = DIRECTION('',(0.,-1.,0.)) ;
#35097 = DIRECTION('',(0.,0.,-1.)) ;
#35098 = DIRECTION('',(0.,1.,0.)) ;
#35099 = DIRECTION('',(0.,0.,1.)) ;
#35100 = DIRECTION('',(0.,-1.,0.)) ;
#35101 = DIRECTION('',(0.,1.,0.)) ;
#35102 = DIRECTION('',(0.,0.,-1.)) ;
#35103 = DIRECTION('',(0.,0.,-1.)) ;
#35104 = DIRECTION('',(0.,1.,0.)) ;
#35105 = DIRECTION('',(0.,0.,-1.)) ;
#35106 = DIRECTION('',(0.,0.,-1.)) ;
#35107 = DIRECTION('',(0.,-1.,0.)) ;
#35108 = DIRECTION('',(0.,0.,-1.)) ;
#35109 = DIRECTION('',(0.,1.,0.)) ;
#35110 = DIRECTION('',(0.,0.,-1.)) ;
#35111 = DIRECTION('',(0.,1.,0.)) ;
#35112 = DIRECTION('',(0.,0.,-1.)) ;
#35113 = DIRECTION('',(0.,0.,-1.)) ;
#35114 = DIRECTION('',(0.,1.,0.)) ;
#35115 = DIRECTION('',(0.,0.,-1.)) ;
#35116 = DIRECTION('',(0.,-1.,0.)) ;
#35117 = DIRECTION('center_axis',(0.,1.,0.)) ;
#35118 = DIRECTION('ref_axis',(0.,0.,1.)) ;
#35119 = DIRECTION('center_axis',(0.,1.,0.)) ;
#35120 = DIRECTION('ref_axis',(1.,0.,0.)) ;
#35121 = DIRECTION('',(0.,0.,-1.)) ;
#35122 = DIRECTION('',(1.,0.,0.)) ;
#35123 = DIRECTION('center_axis',(0.,1.,0.)) ;
#35124 = DIRECTION('ref_axis',(0.,0.,1.)) ;
#35125 = DIRECTION('',(-1.,0.,0.)) ;
#35126 = DIRECTION('',(0.,0.,-1.)) ;
#35127 = DIRECTION('center_axis',(0.,-1.,0.)) ;
#35128 = DIRECTION('ref_axis',(0.,0.,-1.)) ;
#35129 = DIRECTION('',(0.,0.,-1.)) ;
#35130 = DIRECTION('',(1.,0.,0.)) ;
#35131 = DIRECTION('center_axis',(1.,0.,0.)) ;
#35132 = DIRECTION('ref_axis',(0.,0.,-1.)) ;
#35133 = DIRECTION('',(0.,0.,-1.)) ;
#35134 = DIRECTION('',(0.,-1.,0.)) ;
#35135 = DIRECTION('',(0.,0.,-1.)) ;
#35136 = DIRECTION('center_axis',(0.,-1.,0.)) ;
#35137 = DIRECTION('ref_axis',(0.,0.,-1.)) ;
#35138 = DIRECTION('',(-1.,0.,0.)) ;
#35139 = DIRECTION('',(0.,0.,-1.)) ;
#35140 = DIRECTION('center_axis',(1.,0.,0.)) ;
#35141 = DIRECTION('ref_axis',(0.,0.,-1.)) ;
#35142 = DIRECTION('',(0.,0.,-1.)) ;
#35143 = DIRECTION('',(0.,-1.,0.)) ;
#35144 = DIRECTION('',(0.,0.,-1.)) ;
#35145 = DIRECTION('center_axis',(0.,-1.,0.)) ;
#35146 = DIRECTION('ref_axis',(0.,0.,-1.)) ;
#35147 = DIRECTION('',(-1.,0.,0.)) ;
#35148 = DIRECTION('',(0.,0.,-1.)) ;
#35149 = DIRECTION('center_axis',(0.,0.,1.)) ;
#35150 = DIRECTION('ref_axis',(1.,0.,0.)) ;
#35151 = DIRECTION('',(0.,-1.,0.)) ;
#35152 = DIRECTION('',(1.,0.,0.)) ;
#35153 = DIRECTION('',(0.,1.,0.)) ;
#35154 = DIRECTION('center_axis',(0.,0.,1.)) ;
#35155 = DIRECTION('ref_axis',(1.,0.,0.)) ;
#35156 = DIRECTION('',(1.,0.,0.)) ;
#35157 = DIRECTION('',(0.,1.,0.)) ;
#35158 = DIRECTION('center_axis',(0.,-1.,0.)) ;
#35159 = DIRECTION('ref_axis',(0.,0.,-1.)) ;
#35160 = DIRECTION('center_axis',(0.,1.,0.)) ;
#35161 = DIRECTION('ref_axis',(1.,0.,0.)) ;
#35162 = DIRECTION('center_axis',(0.,1.,0.)) ;
#35163 = DIRECTION('ref_axis',(0.,0.,1.)) ;
#35164 = DIRECTION('center_axis',(0.,-1.,0.)) ;
#35165 = DIRECTION('ref_axis',(1.,0.,0.)) ;
#35166 = DIRECTION('center_axis',(0.,0.,1.)) ;
#35167 = DIRECTION('ref_axis',(1.,0.,0.)) ;
#35168 = DIRECTION('',(0.,-1.,0.)) ;
#35169 = DIRECTION('',(-1.,0.,0.)) ;
#35170 = DIRECTION('',(1.,0.,0.)) ;
#35171 = DIRECTION('',(0.,1.,0.)) ;
#35172 = DIRECTION('center_axis',(0.,0.,1.)) ;
#35173 = DIRECTION('ref_axis',(1.,0.,0.)) ;
#35174 = DIRECTION('',(-1.,0.,0.)) ;
#35175 = DIRECTION('',(0.,-1.,0.)) ;
#35176 = DIRECTION('',(1.,0.,0.)) ;
#35177 = DIRECTION('center_axis',(0.,1.,0.)) ;
#35178 = DIRECTION('ref_axis',(0.,0.,1.)) ;
#35179 = DIRECTION('',(1.,0.,0.)) ;
#35180 = DIRECTION('',(0.,0.,-1.)) ;
#35181 = DIRECTION('center_axis',(0.,1.,0.)) ;
#35182 = DIRECTION('ref_axis',(0.,0.,1.)) ;
#35183 = DIRECTION('',(0.,0.,-1.)) ;
#35184 = DIRECTION('center_axis',(0.,1.,0.)) ;
#35185 = DIRECTION('ref_axis',(1.,0.,0.)) ;
#35186 = DIRECTION('center_axis',(0.,1.,0.)) ;
#35187 = DIRECTION('ref_axis',(0.,0.,1.)) ;
#35188 = DIRECTION('',(0.,0.,-1.)) ;
#35189 = DIRECTION('center_axis',(-1.,0.,0.)) ;
#35190 = DIRECTION('ref_axis',(0.,0.,1.)) ;
#35191 = DIRECTION('center_axis',(0.,1.,0.)) ;
#35192 = DIRECTION('ref_axis',(0.,0.,1.)) ;
#35193 = DIRECTION('',(0.,0.,-1.)) ;
#35194 = DIRECTION('center_axis',(-1.,0.,0.)) ;
#35195 = DIRECTION('ref_axis',(0.,0.,1.)) ;
#35196 = DIRECTION('center_axis',(0.,1.,0.)) ;
#35197 = DIRECTION('ref_axis',(1.,0.,0.)) ;
#35198 = DIRECTION('center_axis',(0.,1.,0.)) ;
#35199 = DIRECTION('ref_axis',(1.,0.,0.)) ;
#35200 = DIRECTION('center_axis',(0.,-1.,0.)) ;
#35201 = DIRECTION('ref_axis',(1.,0.,0.)) ;
#35202 = DIRECTION('center_axis',(0.,-1.,0.)) ;
#35203 = DIRECTION('ref_axis',(-1.,0.,0.)) ;
#35204 = DIRECTION('center_axis',(0.,-1.,0.)) ;
#35205 = DIRECTION('ref_axis',(1.,0.,0.)) ;
#35206 = DIRECTION('center_axis',(0.,1.,0.)) ;
#35207 = DIRECTION('ref_axis',(1.,0.,0.)) ;
#35208 = DIRECTION('center_axis',(0.,1.,0.)) ;
#35209 = DIRECTION('ref_axis',(1.,0.,0.)) ;
#35210 = DIRECTION('',(0.,-1.,0.)) ;
#35211 = DIRECTION('center_axis',(0.,1.,0.)) ;
#35212 = DIRECTION('ref_axis',(1.,0.,0.)) ;
#35213 = DIRECTION('',(0.,-1.,0.)) ;
#35214 = DIRECTION('center_axis',(0.,1.,0.)) ;
#35215 = DIRECTION('ref_axis',(1.,0.,0.)) ;
#35216 = DIRECTION('',(0.,1.,0.)) ;
#35217 = DIRECTION('center_axis',(0.,1.,0.)) ;
#35218 = DIRECTION('ref_axis',(1.,0.,0.)) ;
#35219 = DIRECTION('',(0.,1.,0.)) ;
#35220 = DIRECTION('center_axis',(0.,0.,1.)) ;
#35221 = DIRECTION('ref_axis',(1.,0.,0.)) ;
#35222 = DIRECTION('',(1.,0.,0.)) ;
#35223 = DIRECTION('',(0.,1.,0.)) ;
#35224 = DIRECTION('',(-1.,0.,0.)) ;
#35225 = DIRECTION('center_axis',(-1.,0.,0.)) ;
#35226 = DIRECTION('ref_axis',(0.,0.,1.)) ;
#35227 = DIRECTION('',(0.,0.,-1.)) ;
#35228 = DIRECTION('',(0.,-1.,0.)) ;
#35229 = DIRECTION('',(0.,0.,-1.)) ;
#35230 = DIRECTION('',(0.,1.,0.)) ;
#35231 = DIRECTION('center_axis',(1.,0.,0.)) ;
#35232 = DIRECTION('ref_axis',(0.,0.,-1.)) ;
#35233 = DIRECTION('',(0.,0.,-1.)) ;
#35234 = DIRECTION('',(0.,1.,0.)) ;
#35235 = DIRECTION('',(0.,0.,-1.)) ;
#35236 = DIRECTION('',(0.,-1.,0.)) ;
#35237 = DIRECTION('center_axis',(0.,0.,1.)) ;
#35238 = DIRECTION('ref_axis',(1.,0.,0.)) ;
#35239 = DIRECTION('',(-1.,0.,0.)) ;
#35240 = DIRECTION('',(1.,0.,0.)) ;
#35241 = DIRECTION('center_axis',(0.,0.,1.)) ;
#35242 = DIRECTION('ref_axis',(1.,0.,0.)) ;
#35243 = DIRECTION('',(0.,-1.,0.)) ;
#35244 = DIRECTION('',(1.,0.,0.)) ;
#35245 = DIRECTION('',(-1.,0.,0.)) ;
#35246 = DIRECTION('center_axis',(0.,0.,1.)) ;
#35247 = DIRECTION('ref_axis',(1.,0.,0.)) ;
#35248 = DIRECTION('',(-1.,0.,0.)) ;
#35249 = DIRECTION('',(1.,0.,0.)) ;
#35250 = DIRECTION('center_axis',(0.,1.,0.)) ;
#35251 = DIRECTION('ref_axis',(0.,0.,1.)) ;
#35252 = DIRECTION('',(0.,0.,1.)) ;
#35253 = DIRECTION('center_axis',(0.,-1.,0.)) ;
#35254 = DIRECTION('ref_axis',(0.,0.,-1.)) ;
#35255 = DIRECTION('',(0.,0.,-1.)) ;
#35256 = DIRECTION('center_axis',(0.,0.,1.)) ;
#35257 = DIRECTION('ref_axis',(1.,0.,0.)) ;
#35258 = DIRECTION('',(1.,0.,0.)) ;
#35259 = DIRECTION('',(0.,-1.,0.)) ;
#35260 = DIRECTION('',(-1.,0.,0.)) ;
#35261 = DIRECTION('',(0.,1.,0.)) ;
#35262 = DIRECTION('center_axis',(0.,0.,1.)) ;
#35263 = DIRECTION('ref_axis',(1.,0.,0.)) ;
#35264 = DIRECTION('',(0.,-1.,0.)) ;
#35265 = DIRECTION('',(0.,-1.,0.)) ;
#35266 = DIRECTION('center_axis',(-1.,0.,0.)) ;
#35267 = DIRECTION('ref_axis',(0.,0.,1.)) ;
#35268 = DIRECTION('',(0.,-1.,0.)) ;
#35269 = DIRECTION('center_axis',(1.,0.,0.)) ;
#35270 = DIRECTION('ref_axis',(0.,0.,-1.)) ;
#35271 = DIRECTION('',(0.,1.,0.)) ;
#35272 = DIRECTION('center_axis',(0.,0.,1.)) ;
#35273 = DIRECTION('ref_axis',(1.,0.,0.)) ;
#35274 = DIRECTION('',(1.,0.,0.)) ;
#35275 = DIRECTION('',(0.,1.,0.)) ;
#35276 = DIRECTION('',(-1.,0.,0.)) ;
#35277 = DIRECTION('',(0.,-1.,0.)) ;
#35278 = DIRECTION('center_axis',(1.,0.,0.)) ;
#35279 = DIRECTION('ref_axis',(0.,0.,-1.)) ;
#35280 = DIRECTION('',(0.,0.,-1.)) ;
#35281 = DIRECTION('',(0.,0.,-1.)) ;
#35282 = DIRECTION('center_axis',(0.,1.,0.)) ;
#35283 = DIRECTION('ref_axis',(0.,0.,1.)) ;
#35284 = DIRECTION('',(0.,0.,-1.)) ;
#35285 = DIRECTION('center_axis',(-1.,0.,0.)) ;
#35286 = DIRECTION('ref_axis',(0.,0.,1.)) ;
#35287 = DIRECTION('',(0.,0.,-1.)) ;
#35288 = DIRECTION('center_axis',(0.,-1.,0.)) ;
#35289 = DIRECTION('ref_axis',(0.,0.,-1.)) ;
#35290 = DIRECTION('center_axis',(0.,0.,1.)) ;
#35291 = DIRECTION('ref_axis',(1.,0.,0.)) ;
#35292 = DIRECTION('center_axis',(0.,0.,1.)) ;
#35293 = DIRECTION('ref_axis',(1.,0.,0.)) ;
#35294 = DIRECTION('center_axis',(0.,0.,1.)) ;
#35295 = DIRECTION('ref_axis',(1.,0.,0.)) ;
#35296 = DIRECTION('center_axis',(0.,0.,1.)) ;
#35297 = DIRECTION('ref_axis',(1.,0.,0.)) ;
#35298 = DIRECTION('center_axis',(0.,0.,-1.)) ;
#35299 = DIRECTION('ref_axis',(1.,0.,0.)) ;
#35300 = DIRECTION('center_axis',(0.,0.,1.)) ;
#35301 = DIRECTION('ref_axis',(1.,0.,0.)) ;
#35302 = DIRECTION('',(0.,0.,-1.)) ;
#35303 = DIRECTION('center_axis',(0.,0.,-1.)) ;
#35304 = DIRECTION('ref_axis',(1.,0.,0.)) ;
#35305 = DIRECTION('center_axis',(0.,0.,1.)) ;
#35306 = DIRECTION('ref_axis',(1.,0.,0.)) ;
#35307 = DIRECTION('',(0.,0.,1.)) ;
#35308 = DIRECTION('center_axis',(0.,0.,1.)) ;
#35309 = DIRECTION('ref_axis',(1.,0.,0.)) ;
#35310 = DIRECTION('center_axis',(0.,0.,-1.)) ;
#35311 = DIRECTION('ref_axis',(1.,0.,0.)) ;
#35312 = DIRECTION('center_axis',(0.,0.,1.)) ;
#35313 = DIRECTION('ref_axis',(1.,0.,0.)) ;
#35314 = DIRECTION('center_axis',(0.,0.,1.)) ;
#35315 = DIRECTION('ref_axis',(1.,0.,0.)) ;
#35316 = DIRECTION('center_axis',(0.,0.,-1.)) ;
#35317 = DIRECTION('ref_axis',(1.,0.,0.)) ;
#35318 = DIRECTION('center_axis',(0.,0.,1.)) ;
#35319 = DIRECTION('ref_axis',(1.,0.,0.)) ;
#35320 = DIRECTION('',(0.,0.,-1.)) ;
#35321 = DIRECTION('center_axis',(0.,0.,1.)) ;
#35322 = DIRECTION('ref_axis',(1.,0.,0.)) ;
#35323 = DIRECTION('',(0.,0.,1.)) ;
#35324 = DIRECTION('center_axis',(0.,1.,0.)) ;
#35325 = DIRECTION('ref_axis',(1.,0.,0.)) ;
#35326 = DIRECTION('',(0.,1.,0.)) ;
#35327 = DIRECTION('center_axis',(0.,1.,0.)) ;
#35328 = DIRECTION('ref_axis',(1.,0.,0.)) ;
#35329 = DIRECTION('center_axis',(0.,-1.,0.)) ;
#35330 = DIRECTION('ref_axis',(1.,0.,0.)) ;
#35331 = DIRECTION('center_axis',(0.,-1.,0.)) ;
#35332 = DIRECTION('ref_axis',(1.,0.,0.)) ;
#35333 = DIRECTION('center_axis',(0.,-1.,0.)) ;
#35334 = DIRECTION('ref_axis',(0.,0.,-1.)) ;
#35335 = DIRECTION('',(1.,0.,0.)) ;
#35336 = DIRECTION('center_axis',(0.,-1.,0.)) ;
#35337 = DIRECTION('ref_axis',(0.,0.,-1.)) ;
#35338 = DIRECTION('',(0.,0.,-1.)) ;
#35339 = DIRECTION('center_axis',(0.,-1.,0.)) ;
#35340 = DIRECTION('ref_axis',(0.,0.,-1.)) ;
#35341 = DIRECTION('',(0.,0.,-1.)) ;
#35342 = DIRECTION('center_axis',(-1.,0.,0.)) ;
#35343 = DIRECTION('ref_axis',(0.,0.,1.)) ;
#35344 = DIRECTION('',(0.,0.,-1.)) ;
#35345 = DIRECTION('',(0.,-1.,0.)) ;
#35346 = DIRECTION('',(0.,0.,-1.)) ;
#35347 = DIRECTION('center_axis',(0.,-1.,0.)) ;
#35348 = DIRECTION('ref_axis',(0.,0.,-1.)) ;
#35349 = DIRECTION('',(1.,0.,0.)) ;
#35350 = DIRECTION('',(1.,0.,0.)) ;
#35351 = DIRECTION('center_axis',(0.,0.,1.)) ;
#35352 = DIRECTION('ref_axis',(1.,0.,0.)) ;
#35353 = DIRECTION('center_axis',(0.,0.,1.)) ;
#35354 = DIRECTION('ref_axis',(1.,0.,0.)) ;
#35355 = DIRECTION('center_axis',(0.,0.,1.)) ;
#35356 = DIRECTION('ref_axis',(1.,0.,0.)) ;
#35357 = DIRECTION('',(-1.,0.,0.)) ;
#35358 = DIRECTION('center_axis',(0.,1.,0.)) ;
#35359 = DIRECTION('ref_axis',(0.,0.,1.)) ;
#35360 = DIRECTION('',(0.,0.,-1.)) ;
#35361 = DIRECTION('center_axis',(0.,0.,1.)) ;
#35362 = DIRECTION('ref_axis',(1.,0.,0.)) ;
#35363 = DIRECTION('',(-1.,0.,0.)) ;
#35364 = DIRECTION('',(0.,1.,0.)) ;
#35365 = DIRECTION('center_axis',(-1.,0.,0.)) ;
#35366 = DIRECTION('ref_axis',(0.,0.,1.)) ;
#35367 = DIRECTION('',(0.,0.,-1.)) ;
#35368 = DIRECTION('',(0.,-1.,0.)) ;
#35369 = DIRECTION('',(0.,0.,1.)) ;
#35370 = DIRECTION('center_axis',(-1.,0.,0.)) ;
#35371 = DIRECTION('ref_axis',(0.,0.,1.)) ;
#35372 = DIRECTION('',(0.,0.,-1.)) ;
#35373 = DIRECTION('',(0.,-1.,0.)) ;
#35374 = DIRECTION('',(0.,0.,-1.)) ;
#35375 = DIRECTION('',(0.,1.,0.)) ;
#35376 = DIRECTION('center_axis',(1.,0.,0.)) ;
#35377 = DIRECTION('ref_axis',(0.,0.,-1.)) ;
#35378 = DIRECTION('',(0.,0.,-1.)) ;
#35379 = DIRECTION('',(0.,1.,0.)) ;
#35380 = DIRECTION('',(0.,0.,-1.)) ;
#35381 = DIRECTION('',(0.,-1.,0.)) ;
#35382 = DIRECTION('center_axis',(0.,1.,0.)) ;
#35383 = DIRECTION('ref_axis',(0.,0.,1.)) ;
#35384 = DIRECTION('',(-1.,0.,0.)) ;
#35385 = DIRECTION('',(1.,0.,0.)) ;
#35386 = DIRECTION('',(-1.,0.,0.)) ;
#35387 = DIRECTION('center_axis',(0.,0.,1.)) ;
#35388 = DIRECTION('ref_axis',(1.,0.,0.)) ;
#35389 = DIRECTION('',(1.,0.,0.)) ;
#35390 = DIRECTION('center_axis',(0.,0.,1.)) ;
#35391 = DIRECTION('ref_axis',(1.,0.,0.)) ;
#35392 = DIRECTION('',(-1.,0.,0.)) ;
#35393 = DIRECTION('center_axis',(0.,-1.,0.)) ;
#35394 = DIRECTION('ref_axis',(0.,0.,-1.)) ;
#35395 = DIRECTION('',(1.,0.,0.)) ;
#35396 = DIRECTION('center_axis',(0.,0.,1.)) ;
#35397 = DIRECTION('ref_axis',(1.,0.,0.)) ;
#35398 = DIRECTION('center_axis',(0.,1.,0.)) ;
#35399 = DIRECTION('ref_axis',(1.,0.,0.)) ;
#35400 = DIRECTION('center_axis',(0.,-1.,0.)) ;
#35401 = DIRECTION('ref_axis',(1.,0.,0.)) ;
#35402 = DIRECTION('',(0.,-1.,0.)) ;
#35403 = DIRECTION('center_axis',(0.,1.,0.)) ;
#35404 = DIRECTION('ref_axis',(1.,0.,0.)) ;
#35405 = DIRECTION('',(0.,1.,0.)) ;
#35406 = DIRECTION('center_axis',(1.,0.,0.)) ;
#35407 = DIRECTION('ref_axis',(0.,0.,-1.)) ;
#35408 = DIRECTION('',(0.,0.,-1.)) ;
#35409 = DIRECTION('',(0.,-1.,0.)) ;
#35410 = DIRECTION('',(0.,0.,-1.)) ;
#35411 = DIRECTION('center_axis',(0.,-1.,0.)) ;
#35412 = DIRECTION('ref_axis',(0.,0.,-1.)) ;
#35413 = DIRECTION('',(0.,0.,-1.)) ;
#35414 = DIRECTION('',(-1.,0.,0.)) ;
#35415 = DIRECTION('center_axis',(-1.,0.,0.)) ;
#35416 = DIRECTION('ref_axis',(0.,0.,1.)) ;
#35417 = DIRECTION('',(0.,0.,-1.)) ;
#35418 = DIRECTION('',(0.,1.,0.)) ;
#35419 = DIRECTION('center_axis',(0.,1.,0.)) ;
#35420 = DIRECTION('ref_axis',(0.,0.,1.)) ;
#35421 = DIRECTION('',(1.,0.,0.)) ;
#35422 = DIRECTION('center_axis',(0.,0.,1.)) ;
#35423 = DIRECTION('ref_axis',(1.,0.,0.)) ;
#35424 = DIRECTION('center_axis',(0.,0.,1.)) ;
#35425 = DIRECTION('ref_axis',(1.,0.,0.)) ;
#35426 = DIRECTION('',(-1.,0.,0.)) ;
#35427 = DIRECTION('',(0.,1.,0.)) ;
#35428 = DIRECTION('',(1.,0.,0.)) ;
#35429 = DIRECTION('',(0.,-1.,0.)) ;
#35430 = DIRECTION('center_axis',(0.,1.,0.)) ;
#35431 = DIRECTION('ref_axis',(0.,0.,1.)) ;
#35432 = DIRECTION('center_axis',(0.,-1.,0.)) ;
#35433 = DIRECTION('ref_axis',(1.,0.,0.)) ;
#35434 = DIRECTION('',(0.,0.,-1.)) ;
#35435 = DIRECTION('',(0.,0.,-1.)) ;
#35436 = DIRECTION('center_axis',(-1.,0.,0.)) ;
#35437 = DIRECTION('ref_axis',(0.,0.,1.)) ;
#35438 = DIRECTION('',(0.,-1.,0.)) ;
#35439 = DIRECTION('',(0.,0.,-1.)) ;
#35440 = DIRECTION('center_axis',(0.,-1.,0.)) ;
#35441 = DIRECTION('ref_axis',(0.,0.,-1.)) ;
#35442 = DIRECTION('center_axis',(0.,1.,0.)) ;
#35443 = DIRECTION('ref_axis',(1.,0.,0.)) ;
#35444 = DIRECTION('',(0.,0.,-1.)) ;
#35445 = DIRECTION('center_axis',(1.,0.,0.)) ;
#35446 = DIRECTION('ref_axis',(0.,0.,-1.)) ;
#35447 = DIRECTION('',(0.,1.,0.)) ;
#35448 = DIRECTION('center_axis',(0.,1.,0.)) ;
#35449 = DIRECTION('ref_axis',(1.,0.,0.)) ;
#35450 = DIRECTION('center_axis',(0.,-1.,0.)) ;
#35451 = DIRECTION('ref_axis',(0.,0.,-1.)) ;
#35452 = DIRECTION('center_axis',(0.,1.,0.)) ;
#35453 = DIRECTION('ref_axis',(1.,0.,0.)) ;
#35454 = DIRECTION('',(1.,0.,0.)) ;
#35455 = DIRECTION('center_axis',(0.,1.,0.)) ;
#35456 = DIRECTION('ref_axis',(0.,0.,1.)) ;
#35457 = DIRECTION('center_axis',(0.,-1.,0.)) ;
#35458 = DIRECTION('ref_axis',(1.,0.,0.)) ;
#35459 = DIRECTION('',(-1.,0.,0.)) ;
#35460 = DIRECTION('center_axis',(0.,0.,1.)) ;
#35461 = DIRECTION('ref_axis',(1.,0.,0.)) ;
#35462 = DIRECTION('',(0.,-1.,0.)) ;
#35463 = DIRECTION('',(0.,1.,0.)) ;
#35464 = DIRECTION('center_axis',(0.,1.,0.)) ;
#35465 = DIRECTION('ref_axis',(1.,0.,0.)) ;
#35466 = DIRECTION('center_axis',(0.,0.,1.)) ;
#35467 = DIRECTION('ref_axis',(1.,0.,0.)) ;
#35468 = DIRECTION('',(1.,0.,0.)) ;
#35469 = DIRECTION('',(0.,1.,0.)) ;
#35470 = DIRECTION('',(-1.,0.,0.)) ;
#35471 = DIRECTION('',(0.,-1.,0.)) ;
#35472 = DIRECTION('center_axis',(-1.,0.,0.)) ;
#35473 = DIRECTION('ref_axis',(0.,0.,1.)) ;
#35474 = DIRECTION('',(0.,0.,1.)) ;
#35475 = DIRECTION('',(0.,0.,-1.)) ;
#35476 = DIRECTION('',(0.,-1.,0.)) ;
#35477 = DIRECTION('center_axis',(0.,1.,0.)) ;
#35478 = DIRECTION('ref_axis',(0.,0.,1.)) ;
#35479 = DIRECTION('center_axis',(0.,1.,0.)) ;
#35480 = DIRECTION('ref_axis',(1.,0.,0.)) ;
#35481 = DIRECTION('center_axis',(0.,-1.,0.)) ;
#35482 = DIRECTION('ref_axis',(0.,0.,-1.)) ;
#35483 = DIRECTION('center_axis',(0.,-1.,0.)) ;
#35484 = DIRECTION('ref_axis',(1.,0.,0.)) ;
#35485 = DIRECTION('center_axis',(0.,1.,0.)) ;
#35486 = DIRECTION('ref_axis',(1.,0.,0.)) ;
#35487 = DIRECTION('center_axis',(0.,-1.,0.)) ;
#35488 = DIRECTION('ref_axis',(0.,0.,-1.)) ;
#35489 = DIRECTION('',(1.,0.,0.)) ;
#35490 = DIRECTION('center_axis',(0.,1.,0.)) ;
#35491 = DIRECTION('ref_axis',(1.,0.,0.)) ;
#35492 = DIRECTION('',(0.,0.,-1.)) ;
#35493 = DIRECTION('center_axis',(1.,0.,0.)) ;
#35494 = DIRECTION('ref_axis',(0.,0.,-1.)) ;
#35495 = DIRECTION('',(0.,1.,0.)) ;
#35496 = DIRECTION('',(0.,-1.,0.)) ;
#35497 = DIRECTION('',(0.,0.,-1.)) ;
#35498 = DIRECTION('center_axis',(0.,1.,0.)) ;
#35499 = DIRECTION('ref_axis',(0.,0.,1.)) ;
#35500 = DIRECTION('',(-1.,0.,0.)) ;
#35501 = DIRECTION('center_axis',(0.,-1.,0.)) ;
#35502 = DIRECTION('ref_axis',(1.,0.,0.)) ;
#35503 = DIRECTION('center_axis',(0.,1.,0.)) ;
#35504 = DIRECTION('ref_axis',(1.,0.,0.)) ;
#35505 = DIRECTION('',(0.,-1.,0.)) ;
#35506 = DIRECTION('center_axis',(0.,0.,1.)) ;
#35507 = DIRECTION('ref_axis',(1.,0.,0.)) ;
#35508 = DIRECTION('center_axis',(0.,0.,1.)) ;
#35509 = DIRECTION('ref_axis',(1.,0.,0.)) ;
#35510 = DIRECTION('',(1.,0.,0.)) ;
#35511 = DIRECTION('',(0.,1.,0.)) ;
#35512 = DIRECTION('',(-1.,0.,0.)) ;
#35513 = DIRECTION('',(0.,-1.,0.)) ;
#35514 = DIRECTION('center_axis',(1.,0.,0.)) ;
#35515 = DIRECTION('ref_axis',(0.,0.,-1.)) ;
#35516 = DIRECTION('',(0.,0.,-1.)) ;
#35517 = DIRECTION('',(0.,1.,0.)) ;
#35518 = DIRECTION('',(0.,0.,1.)) ;
#35519 = DIRECTION('center_axis',(0.,1.,0.)) ;
#35520 = DIRECTION('ref_axis',(0.,0.,1.)) ;
#35521 = DIRECTION('center_axis',(0.,1.,0.)) ;
#35522 = DIRECTION('ref_axis',(1.,0.,0.)) ;
#35523 = DIRECTION('center_axis',(0.,-1.,0.)) ;
#35524 = DIRECTION('ref_axis',(0.,0.,-1.)) ;
#35525 = DIRECTION('center_axis',(0.,-1.,0.)) ;
#35526 = DIRECTION('ref_axis',(1.,0.,0.)) ;
#35527 = DIRECTION('center_axis',(0.,1.,0.)) ;
#35528 = DIRECTION('ref_axis',(1.,0.,0.)) ;
#35529 = DIRECTION('center_axis',(0.,-1.,0.)) ;
#35530 = DIRECTION('ref_axis',(0.,0.,-1.)) ;
#35531 = DIRECTION('',(1.,0.,0.)) ;
#35532 = DIRECTION('',(0.,0.,-1.)) ;
#35533 = DIRECTION('center_axis',(0.,1.,0.)) ;
#35534 = DIRECTION('ref_axis',(1.,0.,0.)) ;
#35535 = DIRECTION('center_axis',(0.,1.,0.)) ;
#35536 = DIRECTION('ref_axis',(0.,0.,1.)) ;
#35537 = DIRECTION('',(-1.,0.,0.)) ;
#35538 = DIRECTION('center_axis',(0.,-1.,0.)) ;
#35539 = DIRECTION('ref_axis',(1.,0.,0.)) ;
#35540 = DIRECTION('',(0.,0.,-1.)) ;
#35541 = DIRECTION('center_axis',(0.,1.,0.)) ;
#35542 = DIRECTION('ref_axis',(1.,0.,0.)) ;
#35543 = DIRECTION('',(0.,1.,0.)) ;
#35544 = DIRECTION('',(0.,1.,0.)) ;
#35545 = DIRECTION('center_axis',(-1.,0.,0.)) ;
#35546 = DIRECTION('ref_axis',(0.,0.,1.)) ;
#35547 = DIRECTION('',(0.,-1.,0.)) ;
#35548 = DIRECTION('center_axis',(0.,0.,1.)) ;
#35549 = DIRECTION('ref_axis',(1.,0.,0.)) ;
#35550 = DIRECTION('center_axis',(0.,0.,1.)) ;
#35551 = DIRECTION('ref_axis',(1.,0.,0.)) ;
#35552 = DIRECTION('',(-1.,0.,0.)) ;
#35553 = DIRECTION('',(0.,-1.,0.)) ;
#35554 = DIRECTION('',(1.,0.,0.)) ;
#35555 = DIRECTION('',(0.,1.,0.)) ;
#35556 = DIRECTION('center_axis',(0.,1.,0.)) ;
#35557 = DIRECTION('ref_axis',(1.,0.,0.)) ;
#35558 = DIRECTION('center_axis',(0.,-1.,0.)) ;
#35559 = DIRECTION('ref_axis',(1.,0.,0.)) ;
#35560 = DIRECTION('',(0.,-1.,0.)) ;
#35561 = DIRECTION('center_axis',(0.,1.,0.)) ;
#35562 = DIRECTION('ref_axis',(1.,0.,0.)) ;
#35563 = DIRECTION('center_axis',(0.,1.,0.)) ;
#35564 = DIRECTION('ref_axis',(0.,0.,1.)) ;
#35565 = DIRECTION('',(0.,0.,-1.)) ;
#35566 = DIRECTION('center_axis',(1.,0.,0.)) ;
#35567 = DIRECTION('ref_axis',(0.,0.,-1.)) ;
#35568 = DIRECTION('',(0.,0.,-1.)) ;
#35569 = DIRECTION('center_axis',(0.,-1.,0.)) ;
#35570 = DIRECTION('ref_axis',(0.,0.,-1.)) ;
#35571 = DIRECTION('center_axis',(0.,-1.,0.)) ;
#35572 = DIRECTION('ref_axis',(0.,0.,-1.)) ;
#35573 = DIRECTION('',(1.,0.,0.)) ;
#35574 = DIRECTION('',(0.,0.,-1.)) ;
#35575 = DIRECTION('center_axis',(0.,1.,0.)) ;
#35576 = DIRECTION('ref_axis',(1.,0.,0.)) ;
#35577 = DIRECTION('center_axis',(0.,1.,0.)) ;
#35578 = DIRECTION('ref_axis',(0.,0.,1.)) ;
#35579 = DIRECTION('',(-1.,0.,0.)) ;
#35580 = DIRECTION('center_axis',(0.,-1.,0.)) ;
#35581 = DIRECTION('ref_axis',(1.,0.,0.)) ;
#35582 = DIRECTION('',(0.,0.,-1.)) ;
#35583 = DIRECTION('center_axis',(0.,1.,0.)) ;
#35584 = DIRECTION('ref_axis',(1.,0.,0.)) ;
#35585 = DIRECTION('',(0.,1.,0.)) ;
#35586 = DIRECTION('',(0.,1.,0.)) ;
#35587 = DIRECTION('center_axis',(-1.,0.,0.)) ;
#35588 = DIRECTION('ref_axis',(0.,0.,1.)) ;
#35589 = DIRECTION('',(0.,-1.,0.)) ;
#35590 = DIRECTION('center_axis',(0.,0.,1.)) ;
#35591 = DIRECTION('ref_axis',(1.,0.,0.)) ;
#35592 = DIRECTION('center_axis',(0.,0.,1.)) ;
#35593 = DIRECTION('ref_axis',(1.,0.,0.)) ;
#35594 = DIRECTION('',(0.,-1.,0.)) ;
#35595 = DIRECTION('',(-1.,0.,0.)) ;
#35596 = DIRECTION('',(0.,1.,0.)) ;
#35597 = DIRECTION('',(1.,0.,0.)) ;
#35598 = DIRECTION('center_axis',(0.,1.,0.)) ;
#35599 = DIRECTION('ref_axis',(0.,0.,1.)) ;
#35600 = DIRECTION('center_axis',(0.,1.,0.)) ;
#35601 = DIRECTION('ref_axis',(1.,0.,0.)) ;
#35602 = DIRECTION('center_axis',(0.,-1.,0.)) ;
#35603 = DIRECTION('ref_axis',(0.,0.,-1.)) ;
#35604 = DIRECTION('center_axis',(0.,-1.,0.)) ;
#35605 = DIRECTION('ref_axis',(1.,0.,0.)) ;
#35606 = DIRECTION('center_axis',(0.,1.,0.)) ;
#35607 = DIRECTION('ref_axis',(6.12323399573677E-17,0.,-1.)) ;
#35608 = DIRECTION('center_axis',(0.,1.,0.)) ;
#35609 = DIRECTION('ref_axis',(6.12323399573677E-17,0.,-1.)) ;
#35610 = DIRECTION('',(0.,1.,0.)) ;
#35611 = DIRECTION('center_axis',(0.,-1.,0.)) ;
#35612 = DIRECTION('ref_axis',(1.,0.,0.)) ;
#35613 = DIRECTION('',(0.,-1.,0.)) ;
#35614 = DIRECTION('center_axis',(0.,1.,0.)) ;
#35615 = DIRECTION('ref_axis',(1.,0.,0.)) ;
#35616 = DIRECTION('center_axis',(0.,1.,0.)) ;
#35617 = DIRECTION('ref_axis',(0.,0.,1.)) ;
#35618 = DIRECTION('',(1.,0.,0.)) ;
#35619 = DIRECTION('center_axis',(0.,-1.,0.)) ;
#35620 = DIRECTION('ref_axis',(0.,0.,-1.)) ;
#35621 = DIRECTION('',(-1.,0.,0.)) ;
#35622 = DIRECTION('center_axis',(0.,0.,1.)) ;
#35623 = DIRECTION('ref_axis',(1.,0.,0.)) ;
#35624 = DIRECTION('center_axis',(0.,0.,1.)) ;
#35625 = DIRECTION('ref_axis',(1.,0.,0.)) ;
#35626 = DIRECTION('',(-1.,0.,0.)) ;
#35627 = DIRECTION('',(0.,-1.,0.)) ;
#35628 = DIRECTION('',(1.,0.,0.)) ;
#35629 = DIRECTION('',(0.,1.,0.)) ;
#35630 = DIRECTION('center_axis',(0.,-1.,0.)) ;
#35631 = DIRECTION('ref_axis',(0.,0.,-1.)) ;
#35632 = DIRECTION('center_axis',(0.,-1.,0.)) ;
#35633 = DIRECTION('ref_axis',(1.,0.,0.)) ;
#35634 = DIRECTION('center_axis',(0.,1.,0.)) ;
#35635 = DIRECTION('ref_axis',(0.,0.,1.)) ;
#35636 = DIRECTION('center_axis',(0.,1.,0.)) ;
#35637 = DIRECTION('ref_axis',(1.,0.,0.)) ;
#35638 = DIRECTION('center_axis',(0.,1.,0.)) ;
#35639 = DIRECTION('ref_axis',(1.,0.,0.)) ;
#35640 = DIRECTION('center_axis',(0.,1.,0.)) ;
#35641 = DIRECTION('ref_axis',(6.12323399573677E-17,0.,-1.)) ;
#35642 = DIRECTION('',(0.,1.,0.)) ;
#35643 = DIRECTION('center_axis',(0.,-1.,0.)) ;
#35644 = DIRECTION('ref_axis',(1.,0.,0.)) ;
#35645 = DIRECTION('',(0.,-1.,0.)) ;
#35646 = DIRECTION('center_axis',(0.,1.,0.)) ;
#35647 = DIRECTION('ref_axis',(1.,0.,0.)) ;
#35648 = DIRECTION('center_axis',(0.,1.,0.)) ;
#35649 = DIRECTION('ref_axis',(0.,0.,1.)) ;
#35650 = DIRECTION('',(-1.,0.,0.)) ;
#35651 = DIRECTION('center_axis',(0.,-1.,0.)) ;
#35652 = DIRECTION('ref_axis',(0.,0.,-1.)) ;
#35653 = DIRECTION('',(1.,0.,0.)) ;
#35654 = DIRECTION('center_axis',(0.,0.,1.)) ;
#35655 = DIRECTION('ref_axis',(1.,0.,0.)) ;
#35656 = DIRECTION('center_axis',(0.,0.,1.)) ;
#35657 = DIRECTION('ref_axis',(1.,0.,0.)) ;
#35658 = DIRECTION('',(0.,1.,0.)) ;
#35659 = DIRECTION('',(-1.,0.,0.)) ;
#35660 = DIRECTION('',(0.,-1.,0.)) ;
#35661 = DIRECTION('',(1.,0.,0.)) ;
#35662 = DIRECTION('center_axis',(0.,1.,0.)) ;
#35663 = DIRECTION('ref_axis',(0.,0.,1.)) ;
#35664 = DIRECTION('center_axis',(0.,1.,0.)) ;
#35665 = DIRECTION('ref_axis',(1.,0.,0.)) ;
#35666 = DIRECTION('center_axis',(0.,1.,0.)) ;
#35667 = DIRECTION('ref_axis',(1.,0.,0.)) ;
#35668 = DIRECTION('center_axis',(0.,-1.,0.)) ;
#35669 = DIRECTION('ref_axis',(1.,0.,0.)) ;
#35670 = DIRECTION('center_axis',(0.,-1.,0.)) ;
#35671 = DIRECTION('ref_axis',(0.,0.,-1.)) ;
#35672 = DIRECTION('center_axis',(0.,-1.,0.)) ;
#35673 = DIRECTION('ref_axis',(0.,0.,-1.)) ;
#35674 = DIRECTION('',(-1.,0.,0.)) ;
#35675 = DIRECTION('',(0.,0.,-1.)) ;
#35676 = DIRECTION('',(1.,0.,0.)) ;
#35677 = DIRECTION('',(0.,0.,-1.)) ;
#35678 = DIRECTION('center_axis',(1.,0.,0.)) ;
#35679 = DIRECTION('ref_axis',(0.,0.,-1.)) ;
#35680 = DIRECTION('',(0.,-1.,0.)) ;
#35681 = DIRECTION('',(0.,0.,-1.)) ;
#35682 = DIRECTION('',(0.,1.,0.)) ;
#35683 = DIRECTION('center_axis',(-1.,0.,0.)) ;
#35684 = DIRECTION('ref_axis',(0.,0.,1.)) ;
#35685 = DIRECTION('',(0.,1.,0.)) ;
#35686 = DIRECTION('',(0.,-1.,0.)) ;
#35687 = DIRECTION('',(0.,0.,-1.)) ;
#35688 = DIRECTION('center_axis',(0.,1.,0.)) ;
#35689 = DIRECTION('ref_axis',(0.,0.,1.)) ;
#35690 = DIRECTION('',(1.,0.,0.)) ;
#35691 = DIRECTION('',(-1.,0.,0.)) ;
#35692 = DIRECTION('center_axis',(0.,0.,1.)) ;
#35693 = DIRECTION('ref_axis',(1.,0.,0.)) ;
#35694 = DIRECTION('center_axis',(0.,0.,1.)) ;
#35695 = DIRECTION('ref_axis',(1.,0.,0.)) ;
#35696 = DIRECTION('center_axis',(0.,0.,1.)) ;
#35697 = DIRECTION('ref_axis',(1.,0.,0.)) ;
#35698 = DIRECTION('',(1.,0.,0.)) ;
#35699 = DIRECTION('',(0.,-1.,0.)) ;
#35700 = DIRECTION('',(-1.,0.,0.)) ;
#35701 = DIRECTION('',(0.,1.,0.)) ;
#35702 = DIRECTION('center_axis',(0.,0.,1.)) ;
#35703 = DIRECTION('ref_axis',(1.,0.,0.)) ;
#35704 = DIRECTION('',(-1.,0.,0.)) ;
#35705 = DIRECTION('',(0.,-1.,0.)) ;
#35706 = DIRECTION('',(1.,0.,0.)) ;
#35707 = DIRECTION('',(0.,1.,0.)) ;
#35708 = DIRECTION('center_axis',(0.,1.,0.)) ;
#35709 = DIRECTION('ref_axis',(0.,0.,1.)) ;
#35710 = DIRECTION('',(0.,0.,-1.)) ;
#35711 = DIRECTION('',(0.,0.,-1.)) ;
#35712 = DIRECTION('center_axis',(-1.,0.,0.)) ;
#35713 = DIRECTION('ref_axis',(0.,0.,1.)) ;
#35714 = DIRECTION('',(0.,0.,-1.)) ;
#35715 = DIRECTION('center_axis',(1.,0.,0.)) ;
#35716 = DIRECTION('ref_axis',(0.,0.,-1.)) ;
#35717 = DIRECTION('',(0.,0.,-1.)) ;
#35718 = DIRECTION('center_axis',(0.,-1.,0.)) ;
#35719 = DIRECTION('ref_axis',(0.,0.,-1.)) ;
#35720 = DIRECTION('center_axis',(0.,1.,0.)) ;
#35721 = DIRECTION('ref_axis',(0.,0.,1.)) ;
#35722 = DIRECTION('',(0.,0.,1.)) ;
#35723 = DIRECTION('',(-1.,0.,0.)) ;
#35724 = DIRECTION('',(0.,0.,-1.)) ;
#35725 = DIRECTION('',(1.,0.,0.)) ;
#35726 = DIRECTION('center_axis',(0.,0.,1.)) ;
#35727 = DIRECTION('ref_axis',(1.,0.,0.)) ;
#35728 = DIRECTION('',(0.,-1.,0.)) ;
#35729 = DIRECTION('',(1.,0.,0.)) ;
#35730 = DIRECTION('',(0.,1.,0.)) ;
#35731 = DIRECTION('center_axis',(0.,-1.,0.)) ;
#35732 = DIRECTION('ref_axis',(0.,0.,-1.)) ;
#35733 = DIRECTION('',(0.,0.,-1.)) ;
#35734 = DIRECTION('',(-1.,0.,0.)) ;
#35735 = DIRECTION('',(0.,0.,1.)) ;
#35736 = DIRECTION('center_axis',(-1.,0.,0.)) ;
#35737 = DIRECTION('ref_axis',(0.,0.,1.)) ;
#35738 = DIRECTION('',(0.,1.,0.)) ;
#35739 = DIRECTION('',(0.,0.,-1.)) ;
#35740 = DIRECTION('',(0.,1.,0.)) ;
#35741 = DIRECTION('',(0.,0.,1.)) ;
#35742 = DIRECTION('',(0.,1.,0.)) ;
#35743 = DIRECTION('',(0.,0.,1.)) ;
#35744 = DIRECTION('',(0.,-1.,0.)) ;
#35745 = DIRECTION('',(0.,0.,-1.)) ;
#35746 = DIRECTION('',(0.,1.,0.)) ;
#35747 = DIRECTION('center_axis',(0.,0.,1.)) ;
#35748 = DIRECTION('ref_axis',(1.,0.,0.)) ;
#35749 = DIRECTION('',(0.,-1.,0.)) ;
#35750 = DIRECTION('',(1.,0.,0.)) ;
#35751 = DIRECTION('center_axis',(0.,0.,1.)) ;
#35752 = DIRECTION('ref_axis',(1.,0.,0.)) ;
#35753 = DIRECTION('',(1.,0.,0.)) ;
#35754 = DIRECTION('',(0.,-1.,0.)) ;
#35755 = DIRECTION('center_axis',(1.,0.,0.)) ;
#35756 = DIRECTION('ref_axis',(0.,0.,-1.)) ;
#35757 = DIRECTION('',(0.,0.,1.)) ;
#35758 = DIRECTION('',(0.,1.,0.)) ;
#35759 = DIRECTION('',(0.,0.,-1.)) ;
#35760 = DIRECTION('',(0.,-1.,0.)) ;
#35761 = DIRECTION('',(0.,0.,-1.)) ;
#35762 = DIRECTION('',(0.,-1.,0.)) ;
#35763 = DIRECTION('',(0.,0.,1.)) ;
#35764 = DIRECTION('center_axis',(0.,0.,1.)) ;
#35765 = DIRECTION('ref_axis',(1.,0.,0.)) ;
#35766 = DIRECTION('',(1.,0.,0.)) ;
#35767 = DIRECTION('',(-1.,0.,0.)) ;
#35768 = DIRECTION('center_axis',(0.,-1.,0.)) ;
#35769 = DIRECTION('ref_axis',(0.,0.,-1.)) ;
#35770 = DIRECTION('center_axis',(0.,1.,0.)) ;
#35771 = DIRECTION('ref_axis',(0.,0.,1.)) ;
#35772 = DIRECTION('',(-1.,0.,0.)) ;
#35773 = DIRECTION('center_axis',(0.,0.,1.)) ;
#35774 = DIRECTION('ref_axis',(1.,0.,0.)) ;
#35775 = DIRECTION('',(-1.,0.,0.)) ;
#35776 = DIRECTION('center_axis',(0.,-1.,0.)) ;
#35777 = DIRECTION('ref_axis',(0.,0.,-1.)) ;
#35778 = DIRECTION('',(1.,0.,0.)) ;
#35779 = DIRECTION('center_axis',(0.,0.,1.)) ;
#35780 = DIRECTION('ref_axis',(1.,0.,0.)) ;
#35781 = DIRECTION('',(-1.,0.,0.)) ;
#35782 = DIRECTION('center_axis',(0.,1.,0.)) ;
#35783 = DIRECTION('ref_axis',(0.,0.,1.)) ;
#35784 = DIRECTION('center_axis',(0.,1.,0.)) ;
#35785 = DIRECTION('ref_axis',(1.,0.,0.)) ;
#35786 = DIRECTION('',(0.,1.,0.)) ;
#35787 = DIRECTION('center_axis',(0.,1.,0.)) ;
#35788 = DIRECTION('ref_axis',(1.,0.,0.)) ;
#35789 = DIRECTION('',(0.,-1.,0.)) ;
#35790 = DIRECTION('center_axis',(0.,-1.,0.)) ;
#35791 = DIRECTION('ref_axis',(1.,0.,0.)) ;
#35792 = DIRECTION('center_axis',(0.,0.,1.)) ;
#35793 = DIRECTION('ref_axis',(1.,0.,0.)) ;
#35794 = DIRECTION('',(1.,0.,0.)) ;
#35795 = DIRECTION('',(-1.,0.,0.)) ;
#35796 = DIRECTION('center_axis',(0.,1.,0.)) ;
#35797 = DIRECTION('ref_axis',(0.,0.,1.)) ;
#35798 = DIRECTION('center_axis',(0.,-1.,0.)) ;
#35799 = DIRECTION('ref_axis',(0.,0.,-1.)) ;
#35800 = DIRECTION('center_axis',(0.,-1.,0.)) ;
#35801 = DIRECTION('ref_axis',(0.,0.,-1.)) ;
#35802 = DIRECTION('center_axis',(0.,-1.,0.)) ;
#35803 = DIRECTION('ref_axis',(1.,0.,0.)) ;
#35804 = DIRECTION('',(1.,0.,0.)) ;
#35805 = DIRECTION('center_axis',(0.,0.,1.)) ;
#35806 = DIRECTION('ref_axis',(1.,0.,0.)) ;
#35807 = DIRECTION('',(0.,1.,0.)) ;
#35808 = DIRECTION('',(1.,0.,0.)) ;
#35809 = DIRECTION('',(0.,-1.,0.)) ;
#35810 = DIRECTION('center_axis',(0.,1.,0.)) ;
#35811 = DIRECTION('ref_axis',(1.,0.,0.)) ;
#35812 = DIRECTION('center_axis',(0.,1.,0.)) ;
#35813 = DIRECTION('ref_axis',(1.,0.,0.)) ;
#35814 = DIRECTION('',(0.,1.,0.)) ;
#35815 = DIRECTION('center_axis',(0.,-1.,0.)) ;
#35816 = DIRECTION('ref_axis',(1.,0.,0.)) ;
#35817 = DIRECTION('',(0.,-1.,0.)) ;
#35818 = DIRECTION('center_axis',(0.,1.,0.)) ;
#35819 = DIRECTION('ref_axis',(1.,0.,0.)) ;
#35820 = DIRECTION('',(0.,1.,0.)) ;
#35821 = DIRECTION('center_axis',(0.,-1.,0.)) ;
#35822 = DIRECTION('ref_axis',(1.,0.,0.)) ;
#35823 = DIRECTION('',(0.,-1.,0.)) ;
#35824 = DIRECTION('center_axis',(0.,1.,0.)) ;
#35825 = DIRECTION('ref_axis',(1.,0.,0.)) ;
#35826 = DIRECTION('center_axis',(0.,1.,0.)) ;
#35827 = DIRECTION('ref_axis',(0.,0.,1.)) ;
#35828 = DIRECTION('',(-1.,0.,0.)) ;
#35829 = DIRECTION('center_axis',(0.,0.,1.)) ;
#35830 = DIRECTION('ref_axis',(1.,0.,0.)) ;
#35831 = DIRECTION('',(-1.,0.,0.)) ;
#35832 = DIRECTION('center_axis',(0.,1.,0.)) ;
#35833 = DIRECTION('ref_axis',(0.,0.,1.)) ;
#35834 = DIRECTION('',(1.,0.,0.)) ;
#35835 = DIRECTION('center_axis',(0.,-1.,0.)) ;
#35836 = DIRECTION('ref_axis',(0.,0.,-1.)) ;
#35837 = DIRECTION('',(-1.,0.,0.)) ;
#35838 = DIRECTION('center_axis',(0.,0.,1.)) ;
#35839 = DIRECTION('ref_axis',(1.,0.,0.)) ;
#35840 = DIRECTION('axis',(0.,0.,1.)) ;
#35841 = DIRECTION('refdir',(1.,0.,0.)) ;
#35842 = DIRECTION('center_axis',(0.,0.,1.)) ;
#35843 = DIRECTION('ref_axis',(1.,0.,0.)) ;
#35844 = DIRECTION('',(0.,1.,0.)) ;
#35845 = DIRECTION('',(-1.,0.,0.)) ;
#35846 = DIRECTION('',(0.,-1.,0.)) ;
#35847 = DIRECTION('',(1.,0.,0.)) ;
#35848 = DIRECTION('center_axis',(0.,0.,1.)) ;
#35849 = DIRECTION('ref_axis',(1.,0.,0.)) ;
#35850 = DIRECTION('',(0.,-1.,0.)) ;
#35851 = DIRECTION('',(-1.,0.,0.)) ;
#35852 = DIRECTION('',(0.,1.,0.)) ;
#35853 = DIRECTION('',(1.,0.,0.)) ;
#35854 = DIRECTION('center_axis',(0.,1.,0.)) ;
#35855 = DIRECTION('ref_axis',(0.,0.,1.)) ;
#35856 = DIRECTION('',(0.,0.,-1.)) ;
#35857 = DIRECTION('',(0.,0.,-1.)) ;
#35858 = DIRECTION('center_axis',(1.,0.,0.)) ;
#35859 = DIRECTION('ref_axis',(0.,0.,-1.)) ;
#35860 = DIRECTION('',(0.,0.,-1.)) ;
#35861 = DIRECTION('center_axis',(0.,-1.,0.)) ;
#35862 = DIRECTION('ref_axis',(0.,0.,-1.)) ;
#35863 = DIRECTION('',(0.,0.,-1.)) ;
#35864 = DIRECTION('center_axis',(-1.,0.,0.)) ;
#35865 = DIRECTION('ref_axis',(0.,0.,1.)) ;
#35866 = DIRECTION('axis',(0.,0.,1.)) ;
#35867 = DIRECTION('refdir',(1.,0.,0.)) ;
#35868 = DIRECTION('center_axis',(0.,0.,1.)) ;
#35869 = DIRECTION('ref_axis',(1.,0.,0.)) ;
#35870 = DIRECTION('',(0.,0.,1.)) ;
#35871 = DIRECTION('center_axis',(0.,1.,0.)) ;
#35872 = DIRECTION('ref_axis',(1.,0.,0.)) ;
#35873 = DIRECTION('center_axis',(0.,1.,0.)) ;
#35874 = DIRECTION('ref_axis',(1.,0.,0.)) ;
#35875 = DIRECTION('center_axis',(0.,-1.,0.)) ;
#35876 = DIRECTION('ref_axis',(1.,0.,0.)) ;
#35877 = DIRECTION('center_axis',(0.,1.,0.)) ;
#35878 = DIRECTION('ref_axis',(1.,0.,0.)) ;
#35879 = DIRECTION('',(0.,-1.,0.)) ;
#35880 = DIRECTION('center_axis',(0.,-1.,0.)) ;
#35881 = DIRECTION('ref_axis',(1.,0.,0.)) ;
#35882 = DIRECTION('center_axis',(0.,-1.,0.)) ;
#35883 = DIRECTION('ref_axis',(-1.,0.,0.)) ;
#35884 = DIRECTION('center_axis',(0.,1.,0.)) ;
#35885 = DIRECTION('ref_axis',(1.,0.,0.)) ;
#35886 = DIRECTION('center_axis',(0.,1.,0.)) ;
#35887 = DIRECTION('ref_axis',(1.,0.,0.)) ;
#35888 = DIRECTION('',(0.,-1.,0.)) ;
#35889 = DIRECTION('center_axis',(0.,1.,0.)) ;
#35890 = DIRECTION('ref_axis',(1.,0.,0.)) ;
#35891 = DIRECTION('axis',(0.,0.,1.)) ;
#35892 = DIRECTION('refdir',(1.,0.,0.)) ;
#35893 = DIRECTION('center_axis',(0.,0.,1.)) ;
#35894 = DIRECTION('ref_axis',(1.,0.,0.)) ;
#35895 = DIRECTION('',(0.,0.,1.)) ;
#35896 = DIRECTION('center_axis',(0.,1.,0.)) ;
#35897 = DIRECTION('ref_axis',(1.,0.,0.)) ;
#35898 = DIRECTION('center_axis',(0.,1.,0.)) ;
#35899 = DIRECTION('ref_axis',(1.,0.,0.)) ;
#35900 = DIRECTION('center_axis',(0.,-1.,0.)) ;
#35901 = DIRECTION('ref_axis',(1.,0.,0.)) ;
#35902 = DIRECTION('center_axis',(0.,1.,0.)) ;
#35903 = DIRECTION('ref_axis',(1.,0.,0.)) ;
#35904 = DIRECTION('',(0.,-1.,0.)) ;
#35905 = DIRECTION('center_axis',(0.,-1.,0.)) ;
#35906 = DIRECTION('ref_axis',(1.,0.,0.)) ;
#35907 = DIRECTION('center_axis',(0.,-1.,0.)) ;
#35908 = DIRECTION('ref_axis',(-1.,0.,0.)) ;
#35909 = DIRECTION('center_axis',(0.,1.,0.)) ;
#35910 = DIRECTION('ref_axis',(1.,0.,0.)) ;
#35911 = DIRECTION('center_axis',(0.,1.,0.)) ;
#35912 = DIRECTION('ref_axis',(1.,0.,0.)) ;
#35913 = DIRECTION('',(0.,-1.,0.)) ;
#35914 = DIRECTION('center_axis',(0.,1.,0.)) ;
#35915 = DIRECTION('ref_axis',(1.,0.,0.)) ;
#35916 = DIRECTION('',(0.,0.,1.)) ;
#35917 = DIRECTION('',(1.,0.,0.)) ;
#35918 = DIRECTION('',(0.,0.,1.)) ;
#35919 = DIRECTION('',(1.,0.,0.)) ;
#35920 = DIRECTION('',(0.,0.,1.)) ;
#35921 = DIRECTION('',(1.,0.,0.)) ;
#35922 = DIRECTION('',(0.,0.,1.)) ;
#35923 = DIRECTION('',(1.,0.,0.)) ;
#35924 = DIRECTION('',(0.,0.,1.)) ;
#35925 = DIRECTION('',(1.,0.,0.)) ;
#35926 = DIRECTION('',(0.,0.,1.)) ;
#35927 = DIRECTION('',(1.,0.,0.)) ;
#35928 = DIRECTION('',(0.,0.,1.)) ;
#35929 = DIRECTION('',(-1.,1.22464679914735E-16,0.)) ;
#35930 = DIRECTION('',(0.,0.,1.)) ;
#35931 = DIRECTION('',(1.,0.,0.)) ;
#35932 = DIRECTION('axis',(0.,0.,1.)) ;
#35933 = DIRECTION('refdir',(1.,0.,0.)) ;
#35934 = DIRECTION('axis',(0.,0.,1.)) ;
#35935 = DIRECTION('refdir',(1.,0.,0.)) ;
#35936 = DIRECTION('center_axis',(0.,0.,1.)) ;
#35937 = DIRECTION('ref_axis',(1.,0.,0.)) ;
#35938 = DIRECTION('center_axis',(0.,0.,1.)) ;
#35939 = DIRECTION('ref_axis',(1.,0.,0.)) ;
#35940 = DIRECTION('',(0.,0.,1.)) ;
#35941 = DIRECTION('center_axis',(0.,0.,-1.)) ;
#35942 = DIRECTION('ref_axis',(1.,0.,0.)) ;
#35943 = DIRECTION('center_axis',(0.,0.,1.)) ;
#35944 = DIRECTION('ref_axis',(1.,0.,0.)) ;
#35945 = DIRECTION('center_axis',(0.,0.,1.)) ;
#35946 = DIRECTION('ref_axis',(1.,0.,0.)) ;
#35947 = DIRECTION('',(0.,0.,1.)) ;
#35948 = DIRECTION('center_axis',(0.,0.,-1.)) ;
#35949 = DIRECTION('ref_axis',(1.,0.,0.)) ;
#35950 = DIRECTION('center_axis',(0.,0.,1.)) ;
#35951 = DIRECTION('ref_axis',(1.,0.,0.)) ;
#35952 = DIRECTION('center_axis',(0.,0.,1.)) ;
#35953 = DIRECTION('ref_axis',(1.,0.,0.)) ;
#35954 = DIRECTION('',(0.,0.,1.)) ;
#35955 = DIRECTION('center_axis',(0.,0.,-1.)) ;
#35956 = DIRECTION('ref_axis',(1.,0.,0.)) ;
#35957 = DIRECTION('center_axis',(0.,0.,1.)) ;
#35958 = DIRECTION('ref_axis',(1.,0.,0.)) ;
#35959 = DIRECTION('center_axis',(0.,0.,1.)) ;
#35960 = DIRECTION('ref_axis',(1.,0.,0.)) ;
#35961 = DIRECTION('',(0.,0.,1.)) ;
#35962 = DIRECTION('center_axis',(0.,0.,-1.)) ;
#35963 = DIRECTION('ref_axis',(1.,0.,0.)) ;
#35964 = DIRECTION('center_axis',(0.,0.,1.)) ;
#35965 = DIRECTION('ref_axis',(1.,0.,0.)) ;
#35966 = DIRECTION('',(0.,0.,1.)) ;
#35967 = DIRECTION('center_axis',(0.,0.,-1.)) ;
#35968 = DIRECTION('ref_axis',(1.,0.,0.)) ;
#35969 = DIRECTION('',(0.,0.,-1.)) ;
#35970 = DIRECTION('center_axis',(0.,0.,-1.)) ;
#35971 = DIRECTION('ref_axis',(1.,0.,0.)) ;
#35972 = DIRECTION('center_axis',(0.,0.,-1.)) ;
#35973 = DIRECTION('ref_axis',(-1.,0.,0.)) ;
#35974 = DIRECTION('',(0.,1.,0.)) ;
#35975 = DIRECTION('center_axis',(0.,0.,1.)) ;
#35976 = DIRECTION('ref_axis',(1.,0.,0.)) ;
#35977 = DIRECTION('',(0.,-1.,0.)) ;
#35978 = DIRECTION('',(1.,0.,0.)) ;
#35979 = DIRECTION('center_axis',(0.,0.,-1.)) ;
#35980 = DIRECTION('ref_axis',(1.,0.,0.)) ;
#35981 = DIRECTION('center_axis',(0.,0.,-1.)) ;
#35982 = DIRECTION('ref_axis',(1.,0.,0.)) ;
#35983 = DIRECTION('center_axis',(0.,0.,-1.)) ;
#35984 = DIRECTION('ref_axis',(1.,0.,0.)) ;
#35985 = DIRECTION('center_axis',(0.,0.,-1.)) ;
#35986 = DIRECTION('ref_axis',(1.,0.,0.)) ;
#35987 = DIRECTION('center_axis',(0.,0.,-1.)) ;
#35988 = DIRECTION('ref_axis',(1.,0.,0.)) ;
#35989 = DIRECTION('',(1.,0.,0.)) ;
#35990 = DIRECTION('',(0.,1.,0.)) ;
#35991 = DIRECTION('center_axis',(0.,0.,-1.)) ;
#35992 = DIRECTION('ref_axis',(1.,0.,0.)) ;
#35993 = DIRECTION('',(0.,1.,0.)) ;
#35994 = DIRECTION('center_axis',(0.,0.,-1.)) ;
#35995 = DIRECTION('ref_axis',(1.,0.,0.)) ;
#35996 = DIRECTION('',(0.,1.,0.)) ;
#35997 = DIRECTION('',(-1.,0.,0.)) ;
#35998 = DIRECTION('',(0.,-1.,0.)) ;
#35999 = DIRECTION('center_axis',(0.,0.,-1.)) ;
#36000 = DIRECTION('ref_axis',(1.,0.,0.)) ;
#36001 = DIRECTION('',(0.,-1.,0.)) ;
#36002 = DIRECTION('center_axis',(0.,0.,-1.)) ;
#36003 = DIRECTION('ref_axis',(-1.,0.,0.)) ;
#36004 = DIRECTION('',(0.,1.,0.)) ;
#36005 = DIRECTION('center_axis',(0.,0.,-1.)) ;
#36006 = DIRECTION('ref_axis',(1.,0.,0.)) ;
#36007 = DIRECTION('center_axis',(0.,0.,1.)) ;
#36008 = DIRECTION('ref_axis',(1.,0.,0.)) ;
#36009 = DIRECTION('',(0.,0.,-1.)) ;
#36010 = DIRECTION('',(0.,0.,1.)) ;
#36011 = DIRECTION('center_axis',(1.,0.,0.)) ;
#36012 = DIRECTION('ref_axis',(0.,0.,-1.)) ;
#36013 = DIRECTION('',(0.,0.,-1.)) ;
#36014 = DIRECTION('',(0.,-1.,0.)) ;
#36015 = DIRECTION('',(0.,0.,-1.)) ;
#36016 = DIRECTION('',(0.,1.,0.)) ;
#36017 = DIRECTION('',(0.,0.,-1.)) ;
#36018 = DIRECTION('',(0.,1.,0.)) ;
#36019 = DIRECTION('',(0.,0.,-1.)) ;
#36020 = DIRECTION('',(0.,1.,0.)) ;
#36021 = DIRECTION('',(0.,0.,-1.)) ;
#36022 = DIRECTION('',(0.,-1.,0.)) ;
#36023 = DIRECTION('',(0.,0.,-1.)) ;
#36024 = DIRECTION('center_axis',(1.,0.,0.)) ;
#36025 = DIRECTION('ref_axis',(0.,0.,-1.)) ;
#36026 = DIRECTION('center_axis',(0.,0.,-1.)) ;
#36027 = DIRECTION('ref_axis',(-1.,0.,0.)) ;
#36028 = DIRECTION('',(0.,-1.,0.)) ;
#36029 = DIRECTION('center_axis',(0.,0.,-1.)) ;
#36030 = DIRECTION('ref_axis',(1.,0.,0.)) ;
#36031 = DIRECTION('center_axis',(0.,0.,1.)) ;
#36032 = DIRECTION('ref_axis',(-1.,1.22464679914735E-16,0.)) ;
#36033 = DIRECTION('',(0.,0.,-1.)) ;
#36034 = DIRECTION('',(0.,0.,1.)) ;
#36035 = DIRECTION('center_axis',(-1.,0.,0.)) ;
#36036 = DIRECTION('ref_axis',(0.,0.,1.)) ;
#36037 = DIRECTION('',(0.,0.,-1.)) ;
#36038 = DIRECTION('',(0.,1.,0.)) ;
#36039 = DIRECTION('',(0.,0.,-1.)) ;
#36040 = DIRECTION('',(0.,-1.,0.)) ;
#36041 = DIRECTION('',(0.,0.,-1.)) ;
#36042 = DIRECTION('',(0.,-1.,0.)) ;
#36043 = DIRECTION('',(0.,0.,-1.)) ;
#36044 = DIRECTION('',(0.,-1.,0.)) ;
#36045 = DIRECTION('',(0.,0.,-1.)) ;
#36046 = DIRECTION('',(0.,1.,0.)) ;
#36047 = DIRECTION('',(0.,0.,-1.)) ;
#36048 = DIRECTION('',(0.,0.,-1.)) ;
#36049 = DIRECTION('',(0.,-1.,0.)) ;
#36050 = DIRECTION('',(0.,0.,1.)) ;
#36051 = DIRECTION('center_axis',(-1.,0.,0.)) ;
#36052 = DIRECTION('ref_axis',(0.,0.,-1.)) ;
#36053 = DIRECTION('center_axis',(0.,0.,-1.)) ;
#36054 = DIRECTION('ref_axis',(-1.,0.,0.)) ;
#36055 = DIRECTION('center_axis',(0.,0.,-1.)) ;
#36056 = DIRECTION('ref_axis',(1.,0.,0.)) ;
#36057 = DIRECTION('center_axis',(0.,0.,1.)) ;
#36058 = DIRECTION('ref_axis',(-1.,1.22464679914735E-16,0.)) ;
#36059 = DIRECTION('center_axis',(1.,0.,0.)) ;
#36060 = DIRECTION('ref_axis',(0.,0.,-1.)) ;
#36061 = DIRECTION('center_axis',(-1.,0.,0.)) ;
#36062 = DIRECTION('ref_axis',(0.,0.,-1.)) ;
#36063 = DIRECTION('',(1.,0.,0.)) ;
#36064 = DIRECTION('center_axis',(-1.,0.,0.)) ;
#36065 = DIRECTION('ref_axis',(0.,0.,-1.)) ;
#36066 = DIRECTION('center_axis',(-1.,0.,0.)) ;
#36067 = DIRECTION('ref_axis',(0.,0.,1.)) ;
#36068 = DIRECTION('center_axis',(1.,0.,0.)) ;
#36069 = DIRECTION('ref_axis',(0.,0.,-1.)) ;
#36070 = DIRECTION('center_axis',(1.,0.,0.)) ;
#36071 = DIRECTION('ref_axis',(0.,0.,-1.)) ;
#36072 = DIRECTION('',(-1.,0.,0.)) ;
#36073 = DIRECTION('center_axis',(1.,0.,0.)) ;
#36074 = DIRECTION('ref_axis',(0.,0.,-1.)) ;
#36075 = DIRECTION('center_axis',(1.,0.,0.)) ;
#36076 = DIRECTION('ref_axis',(0.,-1.22464679914735E-16,1.)) ;
#36077 = DIRECTION('',(1.,0.,0.)) ;
#36078 = DIRECTION('center_axis',(1.,0.,0.)) ;
#36079 = DIRECTION('ref_axis',(0.,0.,-1.)) ;
#36080 = DIRECTION('',(-1.,0.,0.)) ;
#36081 = DIRECTION('center_axis',(-1.,0.,0.)) ;
#36082 = DIRECTION('ref_axis',(0.,0.,-1.)) ;
#36083 = DIRECTION('center_axis',(1.,0.,0.)) ;
#36084 = DIRECTION('ref_axis',(0.,-1.22464679914735E-16,1.)) ;
#36085 = DIRECTION('',(1.,0.,0.)) ;
#36086 = DIRECTION('center_axis',(1.,0.,0.)) ;
#36087 = DIRECTION('ref_axis',(0.,0.,-1.)) ;
#36088 = DIRECTION('',(-1.,0.,0.)) ;
#36089 = DIRECTION('center_axis',(-1.,0.,0.)) ;
#36090 = DIRECTION('ref_axis',(0.,0.,-1.)) ;
#36091 = DIRECTION('center_axis',(1.,0.,0.)) ;
#36092 = DIRECTION('ref_axis',(0.,0.,-1.)) ;
#36093 = DIRECTION('',(0.,1.,0.)) ;
#36094 = DIRECTION('',(0.,0.,-1.)) ;
#36095 = DIRECTION('',(0.,-1.,0.)) ;
#36096 = DIRECTION('',(0.,0.,-1.)) ;
#36097 = DIRECTION('',(0.,1.,0.)) ;
#36098 = DIRECTION('center_axis',(0.,0.,1.)) ;
#36099 = DIRECTION('ref_axis',(1.,0.,0.)) ;
#36100 = DIRECTION('',(0.,-1.,0.)) ;
#36101 = DIRECTION('',(-1.,0.,0.)) ;
#36102 = DIRECTION('center_axis',(0.,0.,1.)) ;
#36103 = DIRECTION('ref_axis',(1.,0.,0.)) ;
#36104 = DIRECTION('',(1.,0.,0.)) ;
#36105 = DIRECTION('',(0.,-1.,0.)) ;
#36106 = DIRECTION('center_axis',(1.,0.,0.)) ;
#36107 = DIRECTION('ref_axis',(0.,0.,-1.)) ;
#36108 = DIRECTION('',(0.,1.,0.)) ;
#36109 = DIRECTION('',(0.,0.,-1.)) ;
#36110 = DIRECTION('',(0.,-1.,0.)) ;
#36111 = DIRECTION('',(0.,0.,-1.)) ;
#36112 = DIRECTION('',(0.,1.,0.)) ;
#36113 = DIRECTION('center_axis',(0.,0.,1.)) ;
#36114 = DIRECTION('ref_axis',(1.,0.,0.)) ;
#36115 = DIRECTION('',(0.,-1.,0.)) ;
#36116 = DIRECTION('',(-1.,0.,0.)) ;
#36117 = DIRECTION('center_axis',(0.,0.,1.)) ;
#36118 = DIRECTION('ref_axis',(1.,0.,0.)) ;
#36119 = DIRECTION('',(1.,0.,0.)) ;
#36120 = DIRECTION('',(0.,-1.,0.)) ;
#36121 = DIRECTION('center_axis',(0.,1.,0.)) ;
#36122 = DIRECTION('ref_axis',(0.,0.,1.)) ;
#36123 = DIRECTION('',(0.,0.,-1.)) ;
#36124 = DIRECTION('',(1.,0.,0.)) ;
#36125 = DIRECTION('center_axis',(0.,-1.,0.)) ;
#36126 = DIRECTION('ref_axis',(0.,0.,-1.)) ;
#36127 = DIRECTION('',(0.,0.,-1.)) ;
#36128 = DIRECTION('',(-1.,0.,0.)) ;
#36129 = DIRECTION('center_axis',(-1.,0.,0.)) ;
#36130 = DIRECTION('ref_axis',(0.,0.,1.)) ;
#36131 = DIRECTION('',(0.,1.,0.)) ;
#36132 = DIRECTION('center_axis',(0.,1.,0.)) ;
#36133 = DIRECTION('ref_axis',(0.,0.,1.)) ;
#36134 = DIRECTION('',(0.,0.,-1.)) ;
#36135 = DIRECTION('',(1.,0.,0.)) ;
#36136 = DIRECTION('center_axis',(0.,-1.,0.)) ;
#36137 = DIRECTION('ref_axis',(0.,0.,-1.)) ;
#36138 = DIRECTION('',(0.,0.,-1.)) ;
#36139 = DIRECTION('',(-1.,0.,0.)) ;
#36140 = DIRECTION('center_axis',(-1.,0.,0.)) ;
#36141 = DIRECTION('ref_axis',(0.,0.,1.)) ;
#36142 = DIRECTION('',(0.,1.,0.)) ;
#36143 = DIRECTION('center_axis',(0.,0.,1.)) ;
#36144 = DIRECTION('ref_axis',(1.,0.,0.)) ;
#36145 = DIRECTION('center_axis',(0.,0.,1.)) ;
#36146 = DIRECTION('ref_axis',(1.,0.,0.)) ;
#36147 = DIRECTION('center_axis',(0.,0.,1.)) ;
#36148 = DIRECTION('ref_axis',(1.,0.,0.)) ;
#36149 = DIRECTION('center_axis',(0.,0.,1.)) ;
#36150 = DIRECTION('ref_axis',(1.,0.,0.)) ;
#36151 = DIRECTION('center_axis',(0.,0.,1.)) ;
#36152 = DIRECTION('ref_axis',(1.,0.,0.)) ;
#36153 = DIRECTION('',(0.,0.,1.)) ;
#36154 = DIRECTION('',(0.,0.,-1.)) ;
#36155 = DIRECTION('',(0.,0.,1.)) ;
#36156 = DIRECTION('center_axis',(0.,0.,1.)) ;
#36157 = DIRECTION('ref_axis',(1.,0.,0.)) ;
#36158 = DIRECTION('center_axis',(0.,0.,1.)) ;
#36159 = DIRECTION('ref_axis',(1.,0.,0.)) ;
#36160 = DIRECTION('',(0.,0.,-1.)) ;
#36161 = DIRECTION('center_axis',(0.,0.,1.)) ;
#36162 = DIRECTION('ref_axis',(1.,0.,0.)) ;
#36163 = DIRECTION('center_axis',(0.,0.,-1.)) ;
#36164 = DIRECTION('ref_axis',(1.,0.,0.)) ;
#36165 = DIRECTION('',(0.,0.,1.)) ;
#36166 = DIRECTION('center_axis',(0.,0.,-1.)) ;
#36167 = DIRECTION('ref_axis',(1.,0.,0.)) ;
#36168 = DIRECTION('center_axis',(0.,0.,-1.)) ;
#36169 = DIRECTION('ref_axis',(-1.,0.,0.)) ;
#36170 = DIRECTION('center_axis',(0.,0.,1.)) ;
#36171 = DIRECTION('ref_axis',(1.,0.,0.)) ;
#36172 = DIRECTION('center_axis',(0.,1.,0.)) ;
#36173 = DIRECTION('ref_axis',(1.,0.,0.)) ;
#36174 = DIRECTION('center_axis',(0.,1.,0.)) ;
#36175 = DIRECTION('ref_axis',(1.,0.,0.)) ;
#36176 = DIRECTION('',(0.,1.,0.)) ;
#36177 = DIRECTION('center_axis',(0.,1.,0.)) ;
#36178 = DIRECTION('ref_axis',(1.,0.,0.)) ;
#36179 = DIRECTION('center_axis',(0.,1.,0.)) ;
#36180 = DIRECTION('ref_axis',(1.,0.,0.)) ;
#36181 = DIRECTION('center_axis',(0.,1.,0.)) ;
#36182 = DIRECTION('ref_axis',(1.,0.,0.)) ;
#36183 = DIRECTION('center_axis',(0.,1.,0.)) ;
#36184 = DIRECTION('ref_axis',(1.,0.,0.)) ;
#36185 = DIRECTION('',(0.,-1.,0.)) ;
#36186 = DIRECTION('center_axis',(0.,-1.,0.)) ;
#36187 = DIRECTION('ref_axis',(1.,0.,0.)) ;
#36188 = DIRECTION('center_axis',(0.,-1.,0.)) ;
#36189 = DIRECTION('ref_axis',(-1.,0.,0.)) ;
#36190 = DIRECTION('center_axis',(1.,0.,0.)) ;
#36191 = DIRECTION('ref_axis',(0.,0.,-1.)) ;
#36192 = DIRECTION('center_axis',(1.,0.,0.)) ;
#36193 = DIRECTION('ref_axis',(0.,0.,-1.)) ;
#36194 = DIRECTION('',(1.,0.,0.)) ;
#36195 = DIRECTION('center_axis',(1.,0.,0.)) ;
#36196 = DIRECTION('ref_axis',(0.,0.,-1.)) ;
#36197 = DIRECTION('center_axis',(1.,0.,0.)) ;
#36198 = DIRECTION('ref_axis',(0.,0.,-1.)) ;
#36199 = DIRECTION('center_axis',(1.,0.,0.)) ;
#36200 = DIRECTION('ref_axis',(0.,0.,-1.)) ;
#36201 = DIRECTION('',(-1.,0.,0.)) ;
#36202 = DIRECTION('center_axis',(-1.,0.,0.)) ;
#36203 = DIRECTION('ref_axis',(0.,0.,-1.)) ;
#36204 = DIRECTION('center_axis',(-1.,0.,0.)) ;
#36205 = DIRECTION('ref_axis',(0.,0.,1.)) ;
#36206 = DIRECTION('center_axis',(0.,0.,1.)) ;
#36207 = DIRECTION('ref_axis',(1.,0.,0.)) ;
#36208 = DIRECTION('',(0.,1.,0.)) ;
#36209 = DIRECTION('',(1.,0.,0.)) ;
#36210 = DIRECTION('',(1.,0.,0.)) ;
#36211 = DIRECTION('center_axis',(0.,0.,1.)) ;
#36212 = DIRECTION('ref_axis',(1.,0.,0.)) ;
#36213 = DIRECTION('',(0.,-1.,0.)) ;
#36214 = DIRECTION('',(-1.,0.,0.)) ;
#36215 = DIRECTION('',(-1.,0.,0.)) ;
#36216 = DIRECTION('center_axis',(0.,1.,0.)) ;
#36217 = DIRECTION('ref_axis',(0.,0.,1.)) ;
#36218 = DIRECTION('',(0.,0.,-1.)) ;
#36219 = DIRECTION('center_axis',(-1.,0.,0.)) ;
#36220 = DIRECTION('ref_axis',(0.,0.,1.)) ;
#36221 = DIRECTION('',(0.,0.,-1.)) ;
#36222 = DIRECTION('center_axis',(0.,1.,0.)) ;
#36223 = DIRECTION('ref_axis',(0.,0.,1.)) ;
#36224 = DIRECTION('',(-1.,0.,0.)) ;
#36225 = DIRECTION('',(-1.,0.,0.)) ;
#36226 = DIRECTION('',(0.,0.,1.)) ;
#36227 = DIRECTION('',(1.,0.,0.)) ;
#36228 = DIRECTION('center_axis',(0.,0.,1.)) ;
#36229 = DIRECTION('ref_axis',(1.,0.,0.)) ;
#36230 = DIRECTION('',(0.,1.,0.)) ;
#36231 = DIRECTION('',(-1.,0.,0.)) ;
#36232 = DIRECTION('',(-1.,0.,0.)) ;
#36233 = DIRECTION('center_axis',(0.,0.,1.)) ;
#36234 = DIRECTION('ref_axis',(1.,0.,0.)) ;
#36235 = DIRECTION('',(0.,-1.,0.)) ;
#36236 = DIRECTION('',(1.,0.,0.)) ;
#36237 = DIRECTION('',(1.,0.,0.)) ;
#36238 = DIRECTION('center_axis',(0.,-1.,0.)) ;
#36239 = DIRECTION('ref_axis',(0.,0.,-1.)) ;
#36240 = DIRECTION('',(0.,0.,-1.)) ;
#36241 = DIRECTION('center_axis',(-1.,0.,0.)) ;
#36242 = DIRECTION('ref_axis',(0.,0.,1.)) ;
#36243 = DIRECTION('',(0.,0.,1.)) ;
#36244 = DIRECTION('center_axis',(0.,0.,1.)) ;
#36245 = DIRECTION('ref_axis',(1.,0.,0.)) ;
#36246 = DIRECTION('',(0.,-1.,0.)) ;
#36247 = DIRECTION('',(1.,0.,0.)) ;
#36248 = DIRECTION('center_axis',(0.,0.,1.)) ;
#36249 = DIRECTION('ref_axis',(1.,0.,0.)) ;
#36250 = DIRECTION('',(-1.,0.,0.)) ;
#36251 = DIRECTION('',(0.,1.,0.)) ;
#36252 = DIRECTION('center_axis',(0.,1.,0.)) ;
#36253 = DIRECTION('ref_axis',(0.,0.,1.)) ;
#36254 = DIRECTION('',(0.,0.,-1.)) ;
#36255 = DIRECTION('center_axis',(1.,0.,0.)) ;
#36256 = DIRECTION('ref_axis',(0.,0.,-1.)) ;
#36257 = DIRECTION('center_axis',(0.,0.,1.)) ;
#36258 = DIRECTION('ref_axis',(1.,0.,0.)) ;
#36259 = DIRECTION('',(-1.,0.,0.)) ;
#36260 = DIRECTION('',(0.,-1.,0.)) ;
#36261 = DIRECTION('',(-1.,0.,0.)) ;
#36262 = DIRECTION('center_axis',(0.,0.,1.)) ;
#36263 = DIRECTION('ref_axis',(1.,0.,0.)) ;
#36264 = DIRECTION('',(1.,0.,0.)) ;
#36265 = DIRECTION('',(0.,1.,0.)) ;
#36266 = DIRECTION('',(1.,0.,0.)) ;
#36267 = DIRECTION('center_axis',(1.,0.,0.)) ;
#36268 = DIRECTION('ref_axis',(0.,0.,-1.)) ;
#36269 = DIRECTION('',(0.,0.,-1.)) ;
#36270 = DIRECTION('',(0.,0.,-1.)) ;
#36271 = DIRECTION('center_axis',(0.,-1.,0.)) ;
#36272 = DIRECTION('ref_axis',(0.,0.,-1.)) ;
#36273 = DIRECTION('center_axis',(0.,-1.,0.)) ;
#36274 = DIRECTION('ref_axis',(0.,0.,-1.)) ;
#36275 = DIRECTION('',(1.,0.,0.)) ;
#36276 = DIRECTION('center_axis',(0.,0.,1.)) ;
#36277 = DIRECTION('ref_axis',(1.,0.,0.)) ;
#36278 = DIRECTION('axis',(0.,0.,1.)) ;
#36279 = DIRECTION('refdir',(1.,0.,0.)) ;
#36280 = DIRECTION('center_axis',(1.,0.,0.)) ;
#36281 = DIRECTION('ref_axis',(0.,0.,-1.)) ;
#36282 = DIRECTION('center_axis',(1.,0.,0.)) ;
#36283 = DIRECTION('ref_axis',(0.,0.,-1.)) ;
#36284 = DIRECTION('',(-1.,0.,0.)) ;
#36285 = DIRECTION('center_axis',(-1.,0.,0.)) ;
#36286 = DIRECTION('ref_axis',(0.,0.,-1.)) ;
#36287 = DIRECTION('center_axis',(-1.,0.,0.)) ;
#36288 = DIRECTION('ref_axis',(0.,0.,1.)) ;
#36289 = DIRECTION('center_axis',(0.,-0.866025403784439,-0.5)) ;
#36290 = DIRECTION('ref_axis',(0.,0.5,-0.866025403784439)) ;
#36291 = DIRECTION('',(1.,0.,0.)) ;
#36292 = DIRECTION('',(0.,-0.5,0.866025403784439)) ;
#36293 = DIRECTION('',(-1.,0.,0.)) ;
#36294 = DIRECTION('',(0.,0.5,-0.866025403784439)) ;
#36295 = DIRECTION('center_axis',(0.,0.866025403784439,0.5)) ;
#36296 = DIRECTION('ref_axis',(0.,-0.5,0.866025403784439)) ;
#36297 = DIRECTION('',(1.,0.,0.)) ;
#36298 = DIRECTION('',(0.,0.5,-0.866025403784439)) ;
#36299 = DIRECTION('',(-1.,0.,0.)) ;
#36300 = DIRECTION('',(0.,-0.5,0.866025403784439)) ;
#36301 = DIRECTION('center_axis',(-1.,0.,0.)) ;
#36302 = DIRECTION('ref_axis',(0.,0.,1.)) ;
#36303 = DIRECTION('',(0.,0.5,0.866025403784439)) ;
#36304 = DIRECTION('',(0.,1.,0.)) ;
#36305 = DIRECTION('',(0.,-0.5,-0.866025403784439)) ;
#36306 = DIRECTION('',(0.,-1.,0.)) ;
#36307 = DIRECTION('center_axis',(0.,-0.866025403784439,0.5)) ;
#36308 = DIRECTION('ref_axis',(0.,-0.5,-0.866025403784439)) ;
#36309 = DIRECTION('',(1.,0.,0.)) ;
#36310 = DIRECTION('',(0.,-0.5,-0.866025403784439)) ;
#36311 = DIRECTION('center_axis',(0.,0.866025403784439,-0.5)) ;
#36312 = DIRECTION('ref_axis',(0.,0.5,0.866025403784439)) ;
#36313 = DIRECTION('',(1.,0.,0.)) ;
#36314 = DIRECTION('',(0.,0.5,0.866025403784439)) ;
#36315 = DIRECTION('center_axis',(0.,0.,1.)) ;
#36316 = DIRECTION('ref_axis',(0.,-1.,0.)) ;
#36317 = DIRECTION('',(0.,-1.,0.)) ;
#36318 = DIRECTION('center_axis',(0.,0.,-1.)) ;
#36319 = DIRECTION('ref_axis',(0.,1.,0.)) ;
#36320 = DIRECTION('',(0.,1.,0.)) ;
#36321 = DIRECTION('center_axis',(1.,0.,0.)) ;
#36322 = DIRECTION('ref_axis',(0.,0.,-1.)) ;
#36323 = DIRECTION('axis',(0.,0.,1.)) ;
#36324 = DIRECTION('refdir',(1.,0.,0.)) ;
#36325 = DIRECTION('center_axis',(-1.,0.,0.)) ;
#36326 = DIRECTION('ref_axis',(0.,0.,1.)) ;
#36327 = DIRECTION('',(0.,1.,0.)) ;
#36328 = DIRECTION('center_axis',(-1.,0.,0.)) ;
#36329 = DIRECTION('ref_axis',(0.,0.,-1.)) ;
#36330 = DIRECTION('',(0.,0.,-1.)) ;
#36331 = DIRECTION('',(0.,-1.,0.)) ;
#36332 = DIRECTION('center_axis',(1.,0.,0.)) ;
#36333 = DIRECTION('ref_axis',(0.,0.,-1.)) ;
#36334 = DIRECTION('center_axis',(-1.,0.,0.)) ;
#36335 = DIRECTION('ref_axis',(0.,0.,1.)) ;
#36336 = DIRECTION('',(0.,-1.,0.)) ;
#36337 = DIRECTION('center_axis',(1.,0.,0.)) ;
#36338 = DIRECTION('ref_axis',(0.,0.,-1.)) ;
#36339 = DIRECTION('',(0.,1.,0.)) ;
#36340 = DIRECTION('',(0.,0.,-1.)) ;
#36341 = DIRECTION('center_axis',(-1.,0.,0.)) ;
#36342 = DIRECTION('ref_axis',(0.,0.,-1.)) ;
#36343 = DIRECTION('center_axis',(-1.,0.,0.)) ;
#36344 = DIRECTION('ref_axis',(0.,0.,1.)) ;
#36345 = DIRECTION('',(0.,0.,1.)) ;
#36346 = DIRECTION('center_axis',(1.,0.,0.)) ;
#36347 = DIRECTION('ref_axis',(0.,0.,-1.)) ;
#36348 = DIRECTION('',(0.,0.,-1.)) ;
#36349 = DIRECTION('center_axis',(-1.,0.,0.)) ;
#36350 = DIRECTION('ref_axis',(0.,0.,-1.)) ;
#36351 = DIRECTION('center_axis',(-1.,0.,0.)) ;
#36352 = DIRECTION('ref_axis',(0.,0.,1.)) ;
#36353 = DIRECTION('',(0.,1.,0.)) ;
#36354 = DIRECTION('center_axis',(1.,0.,0.)) ;
#36355 = DIRECTION('ref_axis',(0.,0.,-1.)) ;
#36356 = DIRECTION('',(0.,-1.,0.)) ;
#36357 = DIRECTION('center_axis',(-1.,0.,0.)) ;
#36358 = DIRECTION('ref_axis',(0.,0.,-1.)) ;
#36359 = DIRECTION('',(0.,0.,1.)) ;
#36360 = DIRECTION('center_axis',(-1.,0.,0.)) ;
#36361 = DIRECTION('ref_axis',(0.,0.,1.)) ;
#36362 = DIRECTION('',(0.,1.,0.)) ;
#36363 = DIRECTION('center_axis',(1.,0.,0.)) ;
#36364 = DIRECTION('ref_axis',(0.,0.,-1.)) ;
#36365 = DIRECTION('',(0.,-1.,0.)) ;
#36366 = DIRECTION('',(0.,0.,1.)) ;
#36367 = DIRECTION('center_axis',(-1.,0.,0.)) ;
#36368 = DIRECTION('ref_axis',(0.,0.,-1.)) ;
#36369 = DIRECTION('center_axis',(-1.,0.,0.)) ;
#36370 = DIRECTION('ref_axis',(0.,0.,1.)) ;
#36371 = DIRECTION('',(0.,0.,-1.)) ;
#36372 = DIRECTION('center_axis',(1.,0.,0.)) ;
#36373 = DIRECTION('ref_axis',(0.,0.,-1.)) ;
#36374 = DIRECTION('',(0.,0.,1.)) ;
#36375 = DIRECTION('center_axis',(-1.,0.,0.)) ;
#36376 = DIRECTION('ref_axis',(0.,0.,-1.)) ;
#36377 = DIRECTION('center_axis',(1.,0.,0.)) ;
#36378 = DIRECTION('ref_axis',(0.,0.,-1.)) ;
#36379 = DIRECTION('',(-1.,0.,0.)) ;
#36380 = DIRECTION('center_axis',(-1.,0.,0.)) ;
#36381 = DIRECTION('ref_axis',(0.,0.,-1.)) ;
#36382 = DIRECTION('',(1.,0.,0.)) ;
#36383 = DIRECTION('center_axis',(1.,0.,0.)) ;
#36384 = DIRECTION('ref_axis',(0.,-1.22464679914735E-16,1.)) ;
#36385 = DIRECTION('',(-1.,0.,0.)) ;
#36386 = DIRECTION('center_axis',(-1.,0.,0.)) ;
#36387 = DIRECTION('ref_axis',(0.,0.,-1.)) ;
#36388 = DIRECTION('',(1.,0.,0.)) ;
#36389 = DIRECTION('center_axis',(1.,0.,0.)) ;
#36390 = DIRECTION('ref_axis',(0.,0.,-1.)) ;
#36391 = DIRECTION('',(1.,0.,0.)) ;
#36392 = DIRECTION('',(-1.,0.,0.)) ;
#36393 = DIRECTION('center_axis',(-1.,0.,0.)) ;
#36394 = DIRECTION('ref_axis',(0.,0.,-1.)) ;
#36395 = DIRECTION('center_axis',(1.,0.,0.)) ;
#36396 = DIRECTION('ref_axis',(0.,0.,-1.)) ;
#36397 = DIRECTION('',(-1.,0.,0.)) ;
#36398 = DIRECTION('center_axis',(-1.,0.,0.)) ;
#36399 = DIRECTION('ref_axis',(0.,0.,-1.)) ;
#36400 = DIRECTION('',(1.,0.,0.)) ;
#36401 = DIRECTION('center_axis',(1.,0.,0.)) ;
#36402 = DIRECTION('ref_axis',(0.,0.,-1.)) ;
#36403 = DIRECTION('',(-1.,0.,0.)) ;
#36404 = DIRECTION('center_axis',(-1.,0.,0.)) ;
#36405 = DIRECTION('ref_axis',(0.,0.,-1.)) ;
#36406 = DIRECTION('',(1.,0.,0.)) ;
#36407 = DIRECTION('center_axis',(1.,0.,0.)) ;
#36408 = DIRECTION('ref_axis',(0.,0.,-1.)) ;
#36409 = DIRECTION('',(-1.,0.,0.)) ;
#36410 = DIRECTION('center_axis',(-1.,0.,0.)) ;
#36411 = DIRECTION('ref_axis',(0.,0.,-1.)) ;
#36412 = DIRECTION('',(1.,0.,0.)) ;
#36413 = DIRECTION('center_axis',(1.,0.,0.)) ;
#36414 = DIRECTION('ref_axis',(0.,0.,-1.)) ;
#36415 = DIRECTION('',(0.,-1.,0.)) ;
#36416 = DIRECTION('',(0.,1.,0.)) ;
#36417 = DIRECTION('',(0.,0.,1.)) ;
#36418 = DIRECTION('center_axis',(1.,0.,0.)) ;
#36419 = DIRECTION('ref_axis',(0.,0.,-1.)) ;
#36420 = DIRECTION('center_axis',(1.,0.,0.)) ;
#36421 = DIRECTION('ref_axis',(0.,0.,-1.)) ;
#36422 = DIRECTION('',(0.,0.,-1.)) ;
#36423 = DIRECTION('center_axis',(1.,0.,0.)) ;
#36424 = DIRECTION('ref_axis',(0.,0.,-1.)) ;
#36425 = DIRECTION('center_axis',(1.,0.,0.)) ;
#36426 = DIRECTION('ref_axis',(0.,0.,-1.)) ;
#36427 = DIRECTION('',(0.,0.,1.)) ;
#36428 = DIRECTION('center_axis',(1.,0.,0.)) ;
#36429 = DIRECTION('ref_axis',(0.,0.,-1.)) ;
#36430 = DIRECTION('',(0.,-1.,0.)) ;
#36431 = DIRECTION('',(0.,0.,-1.)) ;
#36432 = DIRECTION('center_axis',(1.,0.,0.)) ;
#36433 = DIRECTION('ref_axis',(0.,0.,-1.)) ;
#36434 = DIRECTION('',(0.,1.,0.)) ;
#36435 = DIRECTION('center_axis',(1.,0.,0.)) ;
#36436 = DIRECTION('ref_axis',(0.,0.,-1.)) ;
#36437 = DIRECTION('',(0.,-1.,0.)) ;
#36438 = DIRECTION('center_axis',(1.,0.,0.)) ;
#36439 = DIRECTION('ref_axis',(0.,0.,-1.)) ;
#36440 = DIRECTION('',(0.,0.,-1.)) ;
#36441 = DIRECTION('',(0.,1.,0.)) ;
#36442 = DIRECTION('center_axis',(1.,0.,0.)) ;
#36443 = DIRECTION('ref_axis',(0.,0.,-1.)) ;
#36444 = DIRECTION('',(0.,1.,0.)) ;
#36445 = DIRECTION('center_axis',(1.,0.,0.)) ;
#36446 = DIRECTION('ref_axis',(0.,0.,-1.)) ;
#36447 = DIRECTION('',(0.,0.,1.)) ;
#36448 = DIRECTION('',(0.,-1.,0.)) ;
#36449 = DIRECTION('center_axis',(1.,0.,0.)) ;
#36450 = DIRECTION('ref_axis',(0.,0.,-1.)) ;
#36451 = DIRECTION('',(0.,0.,1.)) ;
#36452 = DIRECTION('center_axis',(1.,0.,0.)) ;
#36453 = DIRECTION('ref_axis',(0.,0.,-1.)) ;
#36454 = DIRECTION('',(0.,0.,-1.)) ;
#36455 = DIRECTION('center_axis',(0.,1.,0.)) ;
#36456 = DIRECTION('ref_axis',(1.,0.,0.)) ;
#36457 = DIRECTION('',(1.,0.,0.)) ;
#36458 = DIRECTION('',(0.,0.,-1.)) ;
#36459 = DIRECTION('',(-1.,0.,0.)) ;
#36460 = DIRECTION('',(0.,0.,1.)) ;
#36461 = DIRECTION('',(1.,0.,0.)) ;
#36462 = DIRECTION('center_axis',(0.,0.,1.)) ;
#36463 = DIRECTION('ref_axis',(1.,0.,0.)) ;
#36464 = DIRECTION('',(1.,0.,0.)) ;
#36465 = DIRECTION('',(0.,-1.,0.)) ;
#36466 = DIRECTION('',(-1.,0.,0.)) ;
#36467 = DIRECTION('',(0.,1.,0.)) ;
#36468 = DIRECTION('',(1.,0.,0.)) ;
#36469 = DIRECTION('center_axis',(0.,-1.,0.)) ;
#36470 = DIRECTION('ref_axis',(1.,0.,0.)) ;
#36471 = DIRECTION('',(1.,0.,0.)) ;
#36472 = DIRECTION('',(0.,0.,-1.)) ;
#36473 = DIRECTION('',(-1.,0.,0.)) ;
#36474 = DIRECTION('center_axis',(0.,0.,-1.)) ;
#36475 = DIRECTION('ref_axis',(0.,1.,0.)) ;
#36476 = DIRECTION('',(1.,0.,0.)) ;
#36477 = DIRECTION('',(0.,-1.,0.)) ;
#36478 = DIRECTION('',(0.,-1.,0.)) ;
#36479 = DIRECTION('',(1.,0.,0.)) ;
#36480 = DIRECTION('center_axis',(0.,1.,0.)) ;
#36481 = DIRECTION('ref_axis',(1.,0.,0.)) ;
#36482 = DIRECTION('',(-1.,0.,0.)) ;
#36483 = DIRECTION('',(0.,0.,-1.)) ;
#36484 = DIRECTION('center_axis',(0.,1.,0.)) ;
#36485 = DIRECTION('ref_axis',(1.,0.,0.)) ;
#36486 = DIRECTION('',(0.,0.,1.)) ;
#36487 = DIRECTION('',(-1.,0.,0.)) ;
#36488 = DIRECTION('center_axis',(0.,0.,1.)) ;
#36489 = DIRECTION('ref_axis',(1.,0.,0.)) ;
#36490 = DIRECTION('',(-1.,0.,0.)) ;
#36491 = DIRECTION('',(0.,-1.,0.)) ;
#36492 = DIRECTION('',(1.,0.,0.)) ;
#36493 = DIRECTION('',(0.,1.,0.)) ;
#36494 = DIRECTION('',(-1.,0.,0.)) ;
#36495 = DIRECTION('center_axis',(0.,1.,0.)) ;
#36496 = DIRECTION('ref_axis',(1.,0.,0.)) ;
#36497 = DIRECTION('',(-1.,0.,0.)) ;
#36498 = DIRECTION('',(0.,0.,1.)) ;
#36499 = DIRECTION('',(1.,0.,0.)) ;
#36500 = DIRECTION('center_axis',(0.,0.,1.)) ;
#36501 = DIRECTION('ref_axis',(1.,0.,0.)) ;
#36502 = DIRECTION('',(-1.,0.,0.)) ;
#36503 = DIRECTION('',(0.,1.,0.)) ;
#36504 = DIRECTION('',(1.,0.,0.)) ;
#36505 = DIRECTION('',(0.,-1.,0.)) ;
#36506 = DIRECTION('',(-1.,0.,0.)) ;
#36507 = DIRECTION('center_axis',(0.,-1.,0.)) ;
#36508 = DIRECTION('ref_axis',(1.,0.,0.)) ;
#36509 = DIRECTION('',(-1.,0.,0.)) ;
#36510 = DIRECTION('',(0.,0.,-1.)) ;
#36511 = DIRECTION('',(1.,0.,0.)) ;
#36512 = DIRECTION('center_axis',(0.,-1.,0.)) ;
#36513 = DIRECTION('ref_axis',(1.,0.,0.)) ;
#36514 = DIRECTION('',(1.,0.,0.)) ;
#36515 = DIRECTION('',(0.,0.,1.)) ;
#36516 = DIRECTION('',(-1.,0.,0.)) ;
#36517 = DIRECTION('center_axis',(0.,-1.,0.)) ;
#36518 = DIRECTION('ref_axis',(1.,0.,0.)) ;
#36519 = DIRECTION('',(-1.,0.,0.)) ;
#36520 = DIRECTION('',(0.,0.,1.)) ;
#36521 = DIRECTION('',(1.,0.,0.)) ;
#36522 = DIRECTION('',(0.,0.,-1.)) ;
#36523 = DIRECTION('',(-1.,0.,0.)) ;
#36524 = DIRECTION('center_axis',(1.,0.,0.)) ;
#36525 = DIRECTION('ref_axis',(0.,1.22464679914735E-16,1.)) ;
#36526 = DIRECTION('center_axis',(-1.,0.,0.)) ;
#36527 = DIRECTION('ref_axis',(0.,0.,-1.)) ;
#36528 = DIRECTION('',(1.,0.,0.)) ;
#36529 = DIRECTION('center_axis',(1.,0.,0.)) ;
#36530 = DIRECTION('ref_axis',(0.,0.,-1.)) ;
#36531 = DIRECTION('center_axis',(-1.,0.,0.)) ;
#36532 = DIRECTION('ref_axis',(0.,0.,-1.)) ;
#36533 = DIRECTION('center_axis',(1.,0.,0.)) ;
#36534 = DIRECTION('ref_axis',(0.,0.,-1.)) ;
#36535 = DIRECTION('center_axis',(-1.,0.,0.)) ;
#36536 = DIRECTION('ref_axis',(0.,0.,-1.)) ;
#36537 = DIRECTION('',(1.,0.,0.)) ;
#36538 = DIRECTION('center_axis',(1.,0.,0.)) ;
#36539 = DIRECTION('ref_axis',(0.,0.,-1.)) ;
#36540 = DIRECTION('center_axis',(-1.,0.,0.)) ;
#36541 = DIRECTION('ref_axis',(0.,0.,-1.)) ;
#36542 = DIRECTION('',(1.,0.,0.)) ;
#36543 = DIRECTION('center_axis',(1.,0.,0.)) ;
#36544 = DIRECTION('ref_axis',(0.,0.,-1.)) ;
#36545 = DIRECTION('center_axis',(-1.,0.,0.)) ;
#36546 = DIRECTION('ref_axis',(0.,0.,-1.)) ;
#36547 = DIRECTION('center_axis',(1.,0.,0.)) ;
#36548 = DIRECTION('ref_axis',(0.,0.,-1.)) ;
#36549 = DIRECTION('',(-1.,0.,0.)) ;
#36550 = DIRECTION('center_axis',(-1.,0.,0.)) ;
#36551 = DIRECTION('ref_axis',(0.,0.,-1.)) ;
#36552 = DIRECTION('center_axis',(-1.,0.,0.)) ;
#36553 = DIRECTION('ref_axis',(0.,1.,0.)) ;
#36554 = DIRECTION('center_axis',(1.,0.,0.)) ;
#36555 = DIRECTION('ref_axis',(0.,0.,-1.)) ;
#36556 = DIRECTION('center_axis',(-1.,0.,0.)) ;
#36557 = DIRECTION('ref_axis',(0.,0.,1.)) ;
#36558 = DIRECTION('',(0.,0.,1.)) ;
#36559 = DIRECTION('',(0.,-1.,0.)) ;
#36560 = DIRECTION('',(0.,0.,-1.)) ;
#36561 = DIRECTION('',(0.,0.,1.)) ;
#36562 = DIRECTION('',(0.,1.,0.)) ;
#36563 = DIRECTION('',(0.,0.,1.)) ;
#36564 = DIRECTION('',(0.,1.,0.)) ;
#36565 = DIRECTION('',(0.,0.,-1.)) ;
#36566 = DIRECTION('',(0.,1.,0.)) ;
#36567 = DIRECTION('center_axis',(0.,1.,0.)) ;
#36568 = DIRECTION('ref_axis',(1.,0.,0.)) ;
#36569 = DIRECTION('',(-1.,0.,0.)) ;
#36570 = DIRECTION('',(0.,0.,-1.)) ;
#36571 = DIRECTION('',(1.,0.,0.)) ;
#36572 = DIRECTION('center_axis',(0.,1.,0.)) ;
#36573 = DIRECTION('ref_axis',(1.,0.,0.)) ;
#36574 = DIRECTION('',(-1.,0.,0.)) ;
#36575 = DIRECTION('center_axis',(0.,0.,-1.)) ;
#36576 = DIRECTION('ref_axis',(0.,1.,0.)) ;
#36577 = DIRECTION('',(0.,-1.,0.)) ;
#36578 = DIRECTION('center_axis',(-1.,0.,0.)) ;
#36579 = DIRECTION('ref_axis',(0.,1.,0.)) ;
#36580 = DIRECTION('center_axis',(1.,0.,0.)) ;
#36581 = DIRECTION('ref_axis',(0.,0.,-1.)) ;
#36582 = DIRECTION('center_axis',(-1.,0.,0.)) ;
#36583 = DIRECTION('ref_axis',(0.,0.,1.)) ;
#36584 = DIRECTION('center_axis',(1.,0.,0.)) ;
#36585 = DIRECTION('ref_axis',(0.,0.,-1.)) ;
#36586 = DIRECTION('',(0.,0.,-1.)) ;
#36587 = DIRECTION('center_axis',(0.,-1.,0.)) ;
#36588 = DIRECTION('ref_axis',(0.,0.,-1.)) ;
#36589 = DIRECTION('center_axis',(1.,0.,0.)) ;
#36590 = DIRECTION('ref_axis',(0.,0.,-1.)) ;
#36591 = DIRECTION('center_axis',(1.,0.,0.)) ;
#36592 = DIRECTION('ref_axis',(0.,0.,-1.)) ;
#36593 = DIRECTION('',(-1.,0.,0.)) ;
#36594 = DIRECTION('',(1.,0.,0.)) ;
#36595 = DIRECTION('center_axis',(1.,0.,0.)) ;
#36596 = DIRECTION('ref_axis',(0.,0.,-1.)) ;
#36597 = DIRECTION('',(-1.,0.,0.)) ;
#36598 = DIRECTION('',(1.,0.,0.)) ;
#36599 = DIRECTION('center_axis',(1.,0.,0.)) ;
#36600 = DIRECTION('ref_axis',(0.,0.,-1.)) ;
#36601 = DIRECTION('center_axis',(1.,0.,0.)) ;
#36602 = DIRECTION('ref_axis',(0.,0.,-1.)) ;
#36603 = DIRECTION('center_axis',(0.,-1.,0.)) ;
#36604 = DIRECTION('ref_axis',(1.,0.,0.)) ;
#36605 = DIRECTION('',(0.,0.,1.)) ;
#36606 = DIRECTION('',(1.,0.,0.)) ;
#36607 = DIRECTION('center_axis',(0.,-1.,0.)) ;
#36608 = DIRECTION('ref_axis',(1.,0.,0.)) ;
#36609 = DIRECTION('',(-1.,0.,0.)) ;
#36610 = DIRECTION('',(0.,0.,-1.)) ;
#36611 = DIRECTION('center_axis',(0.,0.,1.)) ;
#36612 = DIRECTION('ref_axis',(0.,-1.,0.)) ;
#36613 = DIRECTION('',(0.,1.,0.)) ;
#36614 = DIRECTION('center_axis',(-1.,0.,0.)) ;
#36615 = DIRECTION('ref_axis',(0.,-1.,0.)) ;
#36616 = DIRECTION('center_axis',(0.,0.,1.)) ;
#36617 = DIRECTION('ref_axis',(0.,-1.,0.)) ;
#36618 = DIRECTION('',(0.,1.,0.)) ;
#36619 = DIRECTION('center_axis',(-1.,0.,0.)) ;
#36620 = DIRECTION('ref_axis',(0.,-1.,0.)) ;
#36621 = DIRECTION('center_axis',(0.,0.,1.)) ;
#36622 = DIRECTION('ref_axis',(1.,0.,0.)) ;
#36623 = DIRECTION('',(-1.,0.,0.)) ;
#36624 = DIRECTION('',(0.,-1.,0.)) ;
#36625 = DIRECTION('center_axis',(0.,1.,0.)) ;
#36626 = DIRECTION('ref_axis',(0.,0.,1.)) ;
#36627 = DIRECTION('',(0.,0.,-1.)) ;
#36628 = DIRECTION('center_axis',(-1.,0.,0.)) ;
#36629 = DIRECTION('ref_axis',(0.,0.,1.)) ;
#36630 = DIRECTION('center_axis',(1.,0.,0.)) ;
#36631 = DIRECTION('ref_axis',(0.,0.,-1.)) ;
#36632 = DIRECTION('center_axis',(1.,0.,0.)) ;
#36633 = DIRECTION('ref_axis',(0.,0.,-1.)) ;
#36634 = DIRECTION('',(-1.,0.,0.)) ;
#36635 = DIRECTION('center_axis',(-1.,0.,0.)) ;
#36636 = DIRECTION('ref_axis',(0.,0.,-1.)) ;
#36637 = DIRECTION('center_axis',(1.,0.,0.)) ;
#36638 = DIRECTION('ref_axis',(0.,0.,-1.)) ;
#36639 = DIRECTION('center_axis',(-1.,0.,0.)) ;
#36640 = DIRECTION('ref_axis',(0.,0.,1.)) ;
#36641 = DIRECTION('center_axis',(-1.,0.,0.)) ;
#36642 = DIRECTION('ref_axis',(0.,0.,-1.)) ;
#36643 = DIRECTION('center_axis',(1.,0.,0.)) ;
#36644 = DIRECTION('ref_axis',(0.,0.,-1.)) ;
#36645 = DIRECTION('center_axis',(1.,0.,0.)) ;
#36646 = DIRECTION('ref_axis',(0.,0.,-1.)) ;
#36647 = DIRECTION('',(-1.,0.,0.)) ;
#36648 = DIRECTION('center_axis',(1.,0.,0.)) ;
#36649 = DIRECTION('ref_axis',(0.,0.,-1.)) ;
#36650 = DIRECTION('axis',(0.,0.,1.)) ;
#36651 = DIRECTION('refdir',(1.,0.,0.)) ;
#36652 = DIRECTION('center_axis',(1.,0.,0.)) ;
#36653 = DIRECTION('ref_axis',(0.,0.,-1.)) ;
#36654 = DIRECTION('center_axis',(1.,0.,0.)) ;
#36655 = DIRECTION('ref_axis',(0.,0.,-1.)) ;
#36656 = DIRECTION('',(1.,0.,0.)) ;
#36657 = DIRECTION('center_axis',(-1.,0.,0.)) ;
#36658 = DIRECTION('ref_axis',(0.,0.,-1.)) ;
#36659 = DIRECTION('center_axis',(1.,0.,0.)) ;
#36660 = DIRECTION('ref_axis',(0.,0.,-1.)) ;
#36661 = DIRECTION('center_axis',(1.,0.,0.)) ;
#36662 = DIRECTION('ref_axis',(0.,0.,-1.)) ;
#36663 = DIRECTION('',(-1.,0.,0.)) ;
#36664 = DIRECTION('center_axis',(-1.,0.,0.)) ;
#36665 = DIRECTION('ref_axis',(0.,0.,-1.)) ;
#36666 = DIRECTION('center_axis',(-1.,0.,0.)) ;
#36667 = DIRECTION('ref_axis',(0.,0.,1.)) ;
#36668 = DIRECTION('center_axis',(1.,0.,0.)) ;
#36669 = DIRECTION('ref_axis',(0.,0.,-1.)) ;
#36670 = DIRECTION('axis',(0.,0.,1.)) ;
#36671 = DIRECTION('refdir',(1.,0.,0.)) ;
#36672 = DIRECTION('center_axis',(1.,0.,0.)) ;
#36673 = DIRECTION('ref_axis',(0.,0.,-1.)) ;
#36674 = DIRECTION('center_axis',(-1.,0.,0.)) ;
#36675 = DIRECTION('ref_axis',(0.,0.,-1.)) ;
#36676 = DIRECTION('',(0.,0.,-1.)) ;
#36677 = DIRECTION('center_axis',(1.,0.,0.)) ;
#36678 = DIRECTION('ref_axis',(0.,0.,-1.)) ;
#36679 = DIRECTION('',(0.,0.,-1.)) ;
#36680 = DIRECTION('center_axis',(0.,-1.,0.)) ;
#36681 = DIRECTION('ref_axis',(0.,0.,-1.)) ;
#36682 = DIRECTION('',(1.,0.,0.)) ;
#36683 = DIRECTION('',(1.,0.,0.)) ;
#36684 = DIRECTION('',(0.,0.,-1.)) ;
#36685 = DIRECTION('',(-1.,0.,0.)) ;
#36686 = DIRECTION('',(0.,0.,1.)) ;
#36687 = DIRECTION('center_axis',(0.,0.,1.)) ;
#36688 = DIRECTION('ref_axis',(1.,0.,0.)) ;
#36689 = DIRECTION('',(0.,-1.,0.)) ;
#36690 = DIRECTION('',(0.,1.,0.)) ;
#36691 = DIRECTION('',(1.,0.,0.)) ;
#36692 = DIRECTION('center_axis',(0.,1.,0.)) ;
#36693 = DIRECTION('ref_axis',(0.,0.,1.)) ;
#36694 = DIRECTION('',(-1.,0.,0.)) ;
#36695 = DIRECTION('',(0.,0.,-1.)) ;
#36696 = DIRECTION('',(0.,0.,1.)) ;
#36697 = DIRECTION('',(-1.,0.,0.)) ;
#36698 = DIRECTION('center_axis',(1.,0.,0.)) ;
#36699 = DIRECTION('ref_axis',(0.,-1.22464679914735E-16,1.)) ;
#36700 = DIRECTION('center_axis',(-1.,0.,0.)) ;
#36701 = DIRECTION('ref_axis',(0.,0.,-1.)) ;
#36702 = DIRECTION('',(-1.,0.,0.)) ;
#36703 = DIRECTION('center_axis',(-1.,0.,0.)) ;
#36704 = DIRECTION('ref_axis',(0.,0.,-1.)) ;
#36705 = DIRECTION('',(1.,0.,0.)) ;
#36706 = DIRECTION('center_axis',(-1.,0.,0.)) ;
#36707 = DIRECTION('ref_axis',(0.,0.,-1.)) ;
#36708 = DIRECTION('center_axis',(1.,0.,0.)) ;
#36709 = DIRECTION('ref_axis',(0.,1.22464679914735E-16,1.)) ;
#36710 = DIRECTION('',(-1.,0.,0.)) ;
#36711 = DIRECTION('center_axis',(1.,0.,0.)) ;
#36712 = DIRECTION('ref_axis',(0.,0.,-1.)) ;
#36713 = DIRECTION('',(1.,0.,0.)) ;
#36714 = DIRECTION('center_axis',(0.,0.,1.)) ;
#36715 = DIRECTION('ref_axis',(1.,0.,0.)) ;
#36716 = DIRECTION('',(0.,1.,0.)) ;
#36717 = DIRECTION('',(1.,0.,0.)) ;
#36718 = DIRECTION('',(0.,-1.,0.)) ;
#36719 = DIRECTION('center_axis',(1.,0.,0.)) ;
#36720 = DIRECTION('ref_axis',(0.,0.,-1.)) ;
#36721 = DIRECTION('',(0.,1.,0.)) ;
#36722 = DIRECTION('',(0.,0.,-1.)) ;
#36723 = DIRECTION('',(0.,1.,0.)) ;
#36724 = DIRECTION('',(0.,0.,-1.)) ;
#36725 = DIRECTION('center_axis',(1.,0.,0.)) ;
#36726 = DIRECTION('ref_axis',(0.,0.,-1.)) ;
#36727 = DIRECTION('',(0.,0.,-1.)) ;
#36728 = DIRECTION('',(0.,-1.,0.)) ;
#36729 = DIRECTION('',(0.,0.,-1.)) ;
#36730 = DIRECTION('center_axis',(0.,0.,1.)) ;
#36731 = DIRECTION('ref_axis',(1.,0.,0.)) ;
#36732 = DIRECTION('',(-1.,0.,0.)) ;
#36733 = DIRECTION('',(1.,0.,0.)) ;
#36734 = DIRECTION('center_axis',(0.,1.,0.)) ;
#36735 = DIRECTION('ref_axis',(0.,0.,1.)) ;
#36736 = DIRECTION('center_axis',(0.,-1.,0.)) ;
#36737 = DIRECTION('ref_axis',(0.,0.,-1.)) ;
#36738 = DIRECTION('',(-1.,0.,0.)) ;
#36739 = DIRECTION('center_axis',(0.,0.,1.)) ;
#36740 = DIRECTION('ref_axis',(1.,0.,0.)) ;
#36741 = DIRECTION('',(0.,-1.,0.)) ;
#36742 = DIRECTION('center_axis',(-1.,0.,0.)) ;
#36743 = DIRECTION('ref_axis',(0.,0.,1.)) ;
#36744 = DIRECTION('axis',(0.,0.,1.)) ;
#36745 = DIRECTION('refdir',(1.,0.,0.)) ;
#36746 = DIRECTION('center_axis',(0.,1.,0.)) ;
#36747 = DIRECTION('ref_axis',(1.,0.,0.)) ;
#36748 = DIRECTION('center_axis',(0.,1.,0.)) ;
#36749 = DIRECTION('ref_axis',(1.,0.,0.)) ;
#36750 = DIRECTION('',(0.,-1.,0.)) ;
#36751 = DIRECTION('center_axis',(0.,-1.,0.)) ;
#36752 = DIRECTION('ref_axis',(1.,0.,0.)) ;
#36753 = DIRECTION('center_axis',(0.,-1.,0.)) ;
#36754 = DIRECTION('ref_axis',(-1.,0.,0.)) ;
#36755 = DIRECTION('center_axis',(0.,1.,0.)) ;
#36756 = DIRECTION('ref_axis',(1.,0.,0.)) ;
#36757 = DIRECTION('axis',(0.,0.,1.)) ;
#36758 = DIRECTION('refdir',(1.,0.,0.)) ;
#36759 = DIRECTION('center_axis',(0.,1.,0.)) ;
#36760 = DIRECTION('ref_axis',(1.,0.,0.)) ;
#36761 = DIRECTION('center_axis',(0.,1.,0.)) ;
#36762 = DIRECTION('ref_axis',(1.,0.,0.)) ;
#36763 = DIRECTION('',(0.,-1.,0.)) ;
#36764 = DIRECTION('center_axis',(0.,-1.,0.)) ;
#36765 = DIRECTION('ref_axis',(1.,0.,0.)) ;
#36766 = DIRECTION('center_axis',(0.,-1.,0.)) ;
#36767 = DIRECTION('ref_axis',(-1.,0.,0.)) ;
#36768 = DIRECTION('center_axis',(0.,1.,0.)) ;
#36769 = DIRECTION('ref_axis',(1.,0.,0.)) ;
#36770 = DIRECTION('center_axis',(0.,1.,0.)) ;
#36771 = DIRECTION('ref_axis',(1.,0.,0.)) ;
#36772 = DIRECTION('',(0.,1.,0.)) ;
#36773 = DIRECTION('center_axis',(0.,-1.,0.)) ;
#36774 = DIRECTION('ref_axis',(1.,0.,0.)) ;
#36775 = DIRECTION('center_axis',(0.,1.,0.)) ;
#36776 = DIRECTION('ref_axis',(1.,0.,0.)) ;
#36777 = DIRECTION('center_axis',(0.,1.,0.)) ;
#36778 = DIRECTION('ref_axis',(1.,0.,0.)) ;
#36779 = DIRECTION('',(0.,-1.,0.)) ;
#36780 = DIRECTION('center_axis',(0.,-1.,0.)) ;
#36781 = DIRECTION('ref_axis',(1.,0.,0.)) ;
#36782 = DIRECTION('center_axis',(0.,-1.,0.)) ;
#36783 = DIRECTION('ref_axis',(-1.,0.,0.)) ;
#36784 = DIRECTION('center_axis',(0.,1.,0.)) ;
#36785 = DIRECTION('ref_axis',(1.,0.,0.)) ;
#36786 = DIRECTION('axis',(0.,0.,1.)) ;
#36787 = DIRECTION('refdir',(1.,0.,0.)) ;
#36788 = DIRECTION('center_axis',(0.,1.,0.)) ;
#36789 = DIRECTION('ref_axis',(1.,0.,0.)) ;
#36790 = DIRECTION('center_axis',(0.,1.,0.)) ;
#36791 = DIRECTION('ref_axis',(1.,0.,0.)) ;
#36792 = DIRECTION('',(0.,1.,0.)) ;
#36793 = DIRECTION('center_axis',(0.,-1.,0.)) ;
#36794 = DIRECTION('ref_axis',(1.,0.,0.)) ;
#36795 = DIRECTION('center_axis',(0.,1.,0.)) ;
#36796 = DIRECTION('ref_axis',(1.,0.,0.)) ;
#36797 = DIRECTION('center_axis',(0.,1.,0.)) ;
#36798 = DIRECTION('ref_axis',(1.,0.,0.)) ;
#36799 = DIRECTION('',(0.,-1.,0.)) ;
#36800 = DIRECTION('center_axis',(0.,-1.,0.)) ;
#36801 = DIRECTION('ref_axis',(1.,0.,0.)) ;
#36802 = DIRECTION('center_axis',(0.,-1.,0.)) ;
#36803 = DIRECTION('ref_axis',(-1.,0.,0.)) ;
#36804 = DIRECTION('center_axis',(0.,1.,0.)) ;
#36805 = DIRECTION('ref_axis',(1.,0.,0.)) ;
#36806 = DIRECTION('center_axis',(0.,1.,0.)) ;
#36807 = DIRECTION('ref_axis',(1.,0.,0.)) ;
#36808 = DIRECTION('center_axis',(0.,1.,0.)) ;
#36809 = DIRECTION('ref_axis',(1.,0.,0.)) ;
#36810 = DIRECTION('',(0.,1.,0.)) ;
#36811 = DIRECTION('center_axis',(0.,-1.,0.)) ;
#36812 = DIRECTION('ref_axis',(1.,0.,0.)) ;
#36813 = DIRECTION('center_axis',(0.,1.,0.)) ;
#36814 = DIRECTION('ref_axis',(1.,0.,0.)) ;
#36815 = DIRECTION('center_axis',(0.,1.,0.)) ;
#36816 = DIRECTION('ref_axis',(1.,0.,0.)) ;
#36817 = DIRECTION('',(0.,-1.,0.)) ;
#36818 = DIRECTION('center_axis',(0.,-1.,0.)) ;
#36819 = DIRECTION('ref_axis',(1.,0.,0.)) ;
#36820 = DIRECTION('center_axis',(0.,-1.,0.)) ;
#36821 = DIRECTION('ref_axis',(-1.,0.,0.)) ;
#36822 = DIRECTION('center_axis',(0.,1.,0.)) ;
#36823 = DIRECTION('ref_axis',(1.,0.,0.)) ;
#36824 = DIRECTION('center_axis',(-0.224859506698758,0.,-0.97439119569462)) ;
#36825 = DIRECTION('ref_axis',(0.97439119569462,0.,-0.224859506698758)) ;
#36826 = DIRECTION('center_axis',(-0.224859506698758,0.,-0.97439119569462)) ;
#36827 = DIRECTION('ref_axis',(0.97439119569462,0.,-0.224859506698758)) ;
#36828 = DIRECTION('',(0.224859506698758,0.,0.97439119569462)) ;
#36829 = DIRECTION('center_axis',(0.224859506698758,0.,0.97439119569462)) ;
#36830 = DIRECTION('ref_axis',(0.97439119569462,0.,-0.224859506698758)) ;
#36831 = DIRECTION('center_axis',(0.224859506698758,0.,0.97439119569462)) ;
#36832 = DIRECTION('ref_axis',(-0.97439119569462,0.,0.224859506698758)) ;
#36833 = DIRECTION('center_axis',(-0.224859506698758,0.,-0.97439119569462)) ;
#36834 = DIRECTION('ref_axis',(0.97439119569462,0.,-0.224859506698758)) ;
#36835 = DIRECTION('axis',(0.,0.,1.)) ;
#36836 = DIRECTION('refdir',(1.,0.,0.)) ;
#36837 = DIRECTION('center_axis',(0.,0.,-1.)) ;
#36838 = DIRECTION('ref_axis',(-1.,0.,0.)) ;
#36839 = DIRECTION('center_axis',(0.,0.,-1.)) ;
#36840 = DIRECTION('ref_axis',(1.,0.,0.)) ;
#36841 = DIRECTION('center_axis',(0.,0.,-1.)) ;
#36842 = DIRECTION('ref_axis',(1.,0.,0.)) ;
#36843 = DIRECTION('center_axis',(0.,0.,1.)) ;
#36844 = DIRECTION('ref_axis',(1.,0.,0.)) ;
#36845 = DIRECTION('center_axis',(0.,0.,1.)) ;
#36846 = DIRECTION('ref_axis',(1.,0.,0.)) ;
#36847 = DIRECTION('center_axis',(0.,0.,1.)) ;
#36848 = DIRECTION('ref_axis',(1.,0.,0.)) ;
#36849 = DIRECTION('center_axis',(0.,0.,1.)) ;
#36850 = DIRECTION('ref_axis',(1.,0.,0.)) ;
#36851 = DIRECTION('',(0.,0.,-1.)) ;
#36852 = DIRECTION('center_axis',(0.,0.,1.)) ;
#36853 = DIRECTION('ref_axis',(1.,0.,0.)) ;
#36854 = DIRECTION('center_axis',(0.,0.,1.)) ;
#36855 = DIRECTION('ref_axis',(1.,0.,0.)) ;
#36856 = DIRECTION('',(0.,0.,-1.)) ;
#36857 = DIRECTION('center_axis',(0.,0.,1.)) ;
#36858 = DIRECTION('ref_axis',(1.,0.,0.)) ;
#36859 = DIRECTION('',(0.,0.,-1.)) ;
#36860 = DIRECTION('center_axis',(0.,0.,-1.)) ;
#36861 = DIRECTION('ref_axis',(1.,0.,0.)) ;
#36862 = DIRECTION('',(0.,0.,-1.)) ;
#36863 = DIRECTION('center_axis',(0.,0.,1.)) ;
#36864 = DIRECTION('ref_axis',(1.,0.,0.)) ;
#36865 = DIRECTION('',(0.,0.,-1.)) ;
#36866 = DIRECTION('center_axis',(0.,0.,-1.)) ;
#36867 = DIRECTION('ref_axis',(1.,0.,0.)) ;
#36868 = DIRECTION('',(0.,0.,-1.)) ;
#36869 = DIRECTION('center_axis',(0.,0.,-1.)) ;
#36870 = DIRECTION('ref_axis',(1.,0.,0.)) ;
#36871 = DIRECTION('',(0.,0.,1.)) ;
#36872 = DIRECTION('center_axis',(0.,0.,1.)) ;
#36873 = DIRECTION('ref_axis',(1.,0.,0.)) ;
#36874 = DIRECTION('center_axis',(0.,0.,-1.)) ;
#36875 = DIRECTION('ref_axis',(1.,0.,0.)) ;
#36876 = DIRECTION('',(0.,0.,1.)) ;
#36877 = DIRECTION('center_axis',(0.,0.,1.)) ;
#36878 = DIRECTION('ref_axis',(1.,0.,0.)) ;
#36879 = DIRECTION('',(0.,0.,-1.)) ;
#36880 = DIRECTION('center_axis',(0.,0.,-1.)) ;
#36881 = DIRECTION('ref_axis',(1.,0.,0.)) ;
#36882 = DIRECTION('',(0.,0.,1.)) ;
#36883 = DIRECTION('center_axis',(0.,0.,1.)) ;
#36884 = DIRECTION('ref_axis',(1.,0.,0.)) ;
#36885 = DIRECTION('',(0.,0.,1.)) ;
#36886 = DIRECTION('center_axis',(0.,0.,1.)) ;
#36887 = DIRECTION('ref_axis',(1.,0.,0.)) ;
#36888 = DIRECTION('',(0.,0.,-1.)) ;
#36889 = DIRECTION('center_axis',(0.,0.,-1.)) ;
#36890 = DIRECTION('ref_axis',(1.,0.,0.)) ;
#36891 = DIRECTION('',(0.,0.,-1.)) ;
#36892 = DIRECTION('center_axis',(0.,0.,-1.)) ;
#36893 = DIRECTION('ref_axis',(1.,0.,0.)) ;
#36894 = DIRECTION('',(0.,0.,1.)) ;
#36895 = DIRECTION('center_axis',(0.,0.,1.)) ;
#36896 = DIRECTION('ref_axis',(1.,0.,0.)) ;
#36897 = DIRECTION('',(0.,0.,-1.)) ;
#36898 = DIRECTION('center_axis',(0.,0.,-1.)) ;
#36899 = DIRECTION('ref_axis',(1.,0.,0.)) ;
#36900 = DIRECTION('',(0.,0.,1.)) ;
#36901 = DIRECTION('center_axis',(0.,0.,1.)) ;
#36902 = DIRECTION('ref_axis',(1.,0.,0.)) ;
#36903 = DIRECTION('',(0.,0.,1.)) ;
#36904 = DIRECTION('center_axis',(0.,0.,1.)) ;
#36905 = DIRECTION('ref_axis',(1.,0.,0.)) ;
#36906 = DIRECTION('',(0.,0.,-1.)) ;
#36907 = DIRECTION('center_axis',(0.,0.,-1.)) ;
#36908 = DIRECTION('ref_axis',(1.,0.,0.)) ;
#36909 = DIRECTION('',(0.,0.,-1.)) ;
#36910 = DIRECTION('center_axis',(0.,0.,-1.)) ;
#36911 = DIRECTION('ref_axis',(1.,0.,0.)) ;
#36912 = DIRECTION('',(0.,0.,1.)) ;
#36913 = DIRECTION('center_axis',(0.,0.,1.)) ;
#36914 = DIRECTION('ref_axis',(1.,0.,0.)) ;
#36915 = DIRECTION('center_axis',(1.,-6.12323399573677E-17,0.)) ;
#36916 = DIRECTION('ref_axis',(6.12323399573677E-17,1.,0.)) ;
#36917 = DIRECTION('',(-6.12323399573677E-17,-1.,0.)) ;
#36918 = DIRECTION('',(0.,0.,-1.)) ;
#36919 = DIRECTION('',(6.12323399573677E-17,1.,0.)) ;
#36920 = DIRECTION('center_axis',(0.,0.,-1.)) ;
#36921 = DIRECTION('ref_axis',(-1.,6.12323399573677E-17,0.)) ;
#36922 = DIRECTION('',(6.12323399573677E-17,1.,0.)) ;
#36923 = DIRECTION('',(-1.,6.12323399573677E-17,0.)) ;
#36924 = DIRECTION('center_axis',(0.,0.,1.)) ;
#36925 = DIRECTION('ref_axis',(1.,-6.12323399573677E-17,0.)) ;
#36926 = DIRECTION('',(-1.,6.12323399573677E-17,0.)) ;
#36927 = DIRECTION('',(-6.12323399573677E-17,-1.,0.)) ;
#36928 = DIRECTION('center_axis',(0.,0.,1.)) ;
#36929 = DIRECTION('ref_axis',(1.,-6.12323399573677E-17,0.)) ;
#36930 = DIRECTION('',(-6.12323399573677E-17,-1.,0.)) ;
#36931 = DIRECTION('',(-1.,6.12323399573677E-17,0.)) ;
#36932 = DIRECTION('',(6.12323399573677E-17,1.,0.)) ;
#36933 = DIRECTION('center_axis',(1.,-6.12323399573677E-17,0.)) ;
#36934 = DIRECTION('ref_axis',(6.12323399573677E-17,1.,0.)) ;
#36935 = DIRECTION('',(0.,0.,1.)) ;
#36936 = DIRECTION('center_axis',(1.,-6.12323399573677E-17,0.)) ;
#36937 = DIRECTION('ref_axis',(6.12323399573677E-17,1.,0.)) ;
#36938 = DIRECTION('',(6.12323399573677E-17,1.,0.)) ;
#36939 = DIRECTION('',(0.,0.,-1.)) ;
#36940 = DIRECTION('center_axis',(1.,-6.12323399573677E-17,0.)) ;
#36941 = DIRECTION('ref_axis',(6.12323399573677E-17,1.,0.)) ;
#36942 = DIRECTION('',(0.,0.,1.)) ;
#36943 = DIRECTION('',(-6.12323399573677E-17,-1.,0.)) ;
#36944 = DIRECTION('center_axis',(6.12323399573677E-17,1.,0.)) ;
#36945 = DIRECTION('ref_axis',(-1.,6.12323399573677E-17,0.)) ;
#36946 = DIRECTION('center_axis',(0.,0.,-1.)) ;
#36947 = DIRECTION('ref_axis',(-1.,6.12323399573677E-17,0.)) ;
#36948 = DIRECTION('',(-1.,6.12323399573677E-17,0.)) ;
#36949 = DIRECTION('center_axis',(-6.12323399573677E-17,-1.,0.)) ;
#36950 = DIRECTION('ref_axis',(1.,-6.12323399573677E-17,0.)) ;
#36951 = DIRECTION('center_axis',(0.,-1.,0.)) ;
#36952 = DIRECTION('ref_axis',(1.,0.,0.)) ;
#36953 = DIRECTION('',(1.,0.,0.)) ;
#36954 = DIRECTION('',(0.,0.,1.)) ;
#36955 = DIRECTION('',(-1.,0.,0.)) ;
#36956 = DIRECTION('center_axis',(0.,0.,1.)) ;
#36957 = DIRECTION('ref_axis',(0.,-1.,0.)) ;
#36958 = DIRECTION('',(-1.,0.,0.)) ;
#36959 = DIRECTION('',(0.,1.,0.)) ;
#36960 = DIRECTION('center_axis',(0.,0.,-1.)) ;
#36961 = DIRECTION('ref_axis',(0.,1.,0.)) ;
#36962 = DIRECTION('',(0.,1.,0.)) ;
#36963 = DIRECTION('',(1.,0.,0.)) ;
#36964 = DIRECTION('center_axis',(0.,0.,-1.)) ;
#36965 = DIRECTION('ref_axis',(0.,1.,0.)) ;
#36966 = DIRECTION('',(1.,0.,0.)) ;
#36967 = DIRECTION('',(0.,1.,0.)) ;
#36968 = DIRECTION('',(-1.,0.,0.)) ;
#36969 = DIRECTION('center_axis',(0.,-1.,0.)) ;
#36970 = DIRECTION('ref_axis',(1.,0.,0.)) ;
#36971 = DIRECTION('',(0.,0.,-1.)) ;
#36972 = DIRECTION('center_axis',(0.,-1.,0.)) ;
#36973 = DIRECTION('ref_axis',(1.,0.,0.)) ;
#36974 = DIRECTION('',(-1.,0.,0.)) ;
#36975 = DIRECTION('',(0.,0.,1.)) ;
#36976 = DIRECTION('center_axis',(0.,-1.,0.)) ;
#36977 = DIRECTION('ref_axis',(1.,0.,0.)) ;
#36978 = DIRECTION('',(0.,0.,-1.)) ;
#36979 = DIRECTION('',(1.,0.,0.)) ;
#36980 = DIRECTION('center_axis',(0.,0.,1.)) ;
#36981 = DIRECTION('ref_axis',(0.,-1.,0.)) ;
#36982 = DIRECTION('',(0.,1.,0.)) ;
#36983 = DIRECTION('center_axis',(1.,0.,0.)) ;
#36984 = DIRECTION('ref_axis',(0.,1.,0.)) ;
#36985 = DIRECTION('center_axis',(-1.,0.,0.)) ;
#36986 = DIRECTION('ref_axis',(0.,-1.,0.)) ;
#36987 = DIRECTION('center_axis',(1.,-6.12323399573677E-17,0.)) ;
#36988 = DIRECTION('ref_axis',(6.12323399573677E-17,1.,0.)) ;
#36989 = DIRECTION('',(-6.12323399573677E-17,-1.,0.)) ;
#36990 = DIRECTION('',(0.,0.,-1.)) ;
#36991 = DIRECTION('',(6.12323399573677E-17,1.,0.)) ;
#36992 = DIRECTION('center_axis',(0.,0.,-1.)) ;
#36993 = DIRECTION('ref_axis',(-1.,6.12323399573677E-17,0.)) ;
#36994 = DIRECTION('',(6.12323399573677E-17,1.,0.)) ;
#36995 = DIRECTION('',(-1.,6.12323399573677E-17,0.)) ;
#36996 = DIRECTION('center_axis',(0.,0.,1.)) ;
#36997 = DIRECTION('ref_axis',(1.,-6.12323399573677E-17,0.)) ;
#36998 = DIRECTION('',(-1.,6.12323399573677E-17,0.)) ;
#36999 = DIRECTION('',(-6.12323399573677E-17,-1.,0.)) ;
#37000 = DIRECTION('center_axis',(0.,0.,1.)) ;
#37001 = DIRECTION('ref_axis',(1.,-6.12323399573677E-17,0.)) ;
#37002 = DIRECTION('',(-6.12323399573677E-17,-1.,0.)) ;
#37003 = DIRECTION('',(-1.,6.12323399573677E-17,0.)) ;
#37004 = DIRECTION('',(6.12323399573677E-17,1.,0.)) ;
#37005 = DIRECTION('center_axis',(1.,-6.12323399573677E-17,0.)) ;
#37006 = DIRECTION('ref_axis',(6.12323399573677E-17,1.,0.)) ;
#37007 = DIRECTION('',(0.,0.,1.)) ;
#37008 = DIRECTION('center_axis',(1.,-6.12323399573677E-17,0.)) ;
#37009 = DIRECTION('ref_axis',(6.12323399573677E-17,1.,0.)) ;
#37010 = DIRECTION('',(6.12323399573677E-17,1.,0.)) ;
#37011 = DIRECTION('',(0.,0.,-1.)) ;
#37012 = DIRECTION('center_axis',(1.,-6.12323399573677E-17,0.)) ;
#37013 = DIRECTION('ref_axis',(6.12323399573677E-17,1.,0.)) ;
#37014 = DIRECTION('',(0.,0.,1.)) ;
#37015 = DIRECTION('',(-6.12323399573677E-17,-1.,0.)) ;
#37016 = DIRECTION('center_axis',(6.12323399573677E-17,1.,0.)) ;
#37017 = DIRECTION('ref_axis',(-1.,6.12323399573677E-17,0.)) ;
#37018 = DIRECTION('center_axis',(0.,0.,-1.)) ;
#37019 = DIRECTION('ref_axis',(-1.,6.12323399573677E-17,0.)) ;
#37020 = DIRECTION('',(-1.,6.12323399573677E-17,0.)) ;
#37021 = DIRECTION('center_axis',(-6.12323399573677E-17,-1.,0.)) ;
#37022 = DIRECTION('ref_axis',(1.,-6.12323399573677E-17,0.)) ;
#37023 = DIRECTION('center_axis',(0.,-1.,0.)) ;
#37024 = DIRECTION('ref_axis',(1.,0.,0.)) ;
#37025 = DIRECTION('',(1.,0.,0.)) ;
#37026 = DIRECTION('',(0.,0.,1.)) ;
#37027 = DIRECTION('',(-1.,0.,0.)) ;
#37028 = DIRECTION('center_axis',(0.,0.,1.)) ;
#37029 = DIRECTION('ref_axis',(0.,-1.,0.)) ;
#37030 = DIRECTION('',(-1.,0.,0.)) ;
#37031 = DIRECTION('',(0.,1.,0.)) ;
#37032 = DIRECTION('center_axis',(0.,0.,-1.)) ;
#37033 = DIRECTION('ref_axis',(0.,1.,0.)) ;
#37034 = DIRECTION('',(0.,1.,0.)) ;
#37035 = DIRECTION('',(1.,0.,0.)) ;
#37036 = DIRECTION('center_axis',(0.,0.,-1.)) ;
#37037 = DIRECTION('ref_axis',(0.,1.,0.)) ;
#37038 = DIRECTION('',(1.,0.,0.)) ;
#37039 = DIRECTION('',(0.,1.,0.)) ;
#37040 = DIRECTION('',(-1.,0.,0.)) ;
#37041 = DIRECTION('center_axis',(0.,-1.,0.)) ;
#37042 = DIRECTION('ref_axis',(1.,0.,0.)) ;
#37043 = DIRECTION('',(0.,0.,-1.)) ;
#37044 = DIRECTION('center_axis',(0.,-1.,0.)) ;
#37045 = DIRECTION('ref_axis',(1.,0.,0.)) ;
#37046 = DIRECTION('',(-1.,0.,0.)) ;
#37047 = DIRECTION('',(0.,0.,1.)) ;
#37048 = DIRECTION('center_axis',(0.,-1.,0.)) ;
#37049 = DIRECTION('ref_axis',(1.,0.,0.)) ;
#37050 = DIRECTION('',(0.,0.,-1.)) ;
#37051 = DIRECTION('',(1.,0.,0.)) ;
#37052 = DIRECTION('center_axis',(0.,0.,1.)) ;
#37053 = DIRECTION('ref_axis',(0.,-1.,0.)) ;
#37054 = DIRECTION('',(0.,1.,0.)) ;
#37055 = DIRECTION('center_axis',(1.,0.,0.)) ;
#37056 = DIRECTION('ref_axis',(0.,1.,0.)) ;
#37057 = DIRECTION('center_axis',(-1.,0.,0.)) ;
#37058 = DIRECTION('ref_axis',(0.,-1.,0.)) ;
#37059 = DIRECTION('center_axis',(0.,0.,1.)) ;
#37060 = DIRECTION('ref_axis',(1.,0.,0.)) ;
#37061 = DIRECTION('',(0.,0.,-1.)) ;
#37062 = DIRECTION('center_axis',(0.,0.,-1.)) ;
#37063 = DIRECTION('ref_axis',(1.,0.,0.)) ;
#37064 = DIRECTION('center_axis',(0.,0.,-1.)) ;
#37065 = DIRECTION('ref_axis',(-1.,0.,0.)) ;
#37066 = DIRECTION('center_axis',(0.,0.,1.)) ;
#37067 = DIRECTION('ref_axis',(1.,0.,0.)) ;
#37068 = DIRECTION('axis',(0.,0.,1.)) ;
#37069 = DIRECTION('refdir',(1.,0.,0.)) ;
#37070 = DIRECTION('center_axis',(0.,0.,1.)) ;
#37071 = DIRECTION('ref_axis',(1.,0.,0.)) ;
#37072 = DIRECTION('center_axis',(0.,0.,1.)) ;
#37073 = DIRECTION('ref_axis',(1.,0.,0.)) ;
#37074 = DIRECTION('',(0.,0.,1.)) ;
#37075 = DIRECTION('center_axis',(0.,0.,-1.)) ;
#37076 = DIRECTION('ref_axis',(1.,0.,0.)) ;
#37077 = DIRECTION('center_axis',(0.,0.,1.)) ;
#37078 = DIRECTION('ref_axis',(1.,0.,0.)) ;
#37079 = DIRECTION('center_axis',(0.,0.,1.)) ;
#37080 = DIRECTION('ref_axis',(1.,0.,0.)) ;
#37081 = DIRECTION('',(0.,0.,-1.)) ;
#37082 = DIRECTION('center_axis',(0.,0.,-1.)) ;
#37083 = DIRECTION('ref_axis',(1.,0.,0.)) ;
#37084 = DIRECTION('center_axis',(0.,0.,-1.)) ;
#37085 = DIRECTION('ref_axis',(-1.,0.,0.)) ;
#37086 = DIRECTION('center_axis',(0.,0.,1.)) ;
#37087 = DIRECTION('ref_axis',(1.,0.,0.)) ;
#37088 = DIRECTION('',(0.,0.,1.)) ;
#37089 = DIRECTION('',(1.,0.,0.)) ;
#37090 = DIRECTION('',(0.,0.,1.)) ;
#37091 = DIRECTION('',(1.,0.,0.)) ;
#37092 = DIRECTION('',(0.,0.,1.)) ;
#37093 = DIRECTION('',(1.,0.,0.)) ;
#37094 = DIRECTION('',(0.,0.,1.)) ;
#37095 = DIRECTION('',(1.,0.,0.)) ;
#37096 = DIRECTION('',(0.,0.,1.)) ;
#37097 = DIRECTION('',(1.,0.,0.)) ;
#37098 = DIRECTION('',(0.,0.,1.)) ;
#37099 = DIRECTION('',(1.,0.,0.)) ;
#37100 = DIRECTION('',(0.,0.,1.)) ;
#37101 = DIRECTION('',(1.,0.,0.)) ;
#37102 = DIRECTION('',(0.,0.,1.)) ;
#37103 = DIRECTION('',(1.,0.,0.)) ;
#37104 = DIRECTION('',(0.,0.,1.)) ;
#37105 = DIRECTION('',(1.,0.,0.)) ;
#37106 = DIRECTION('',(0.,0.,1.)) ;
#37107 = DIRECTION('',(1.,0.,0.)) ;
#37108 = DIRECTION('axis',(0.,0.,1.)) ;
#37109 = DIRECTION('refdir',(1.,0.,0.)) ;
#37110 = DIRECTION('axis',(0.,0.,1.)) ;
#37111 = DIRECTION('refdir',(1.,0.,0.)) ;
#37112 = DIRECTION('center_axis',(0.,0.,1.)) ;
#37113 = DIRECTION('ref_axis',(1.,0.,0.)) ;
#37114 = DIRECTION('center_axis',(0.,0.,1.)) ;
#37115 = DIRECTION('ref_axis',(1.,0.,0.)) ;
#37116 = DIRECTION('',(0.,0.,1.)) ;
#37117 = DIRECTION('center_axis',(0.,0.,-1.)) ;
#37118 = DIRECTION('ref_axis',(1.,0.,0.)) ;
#37119 = DIRECTION('center_axis',(0.,0.,1.)) ;
#37120 = DIRECTION('ref_axis',(1.,0.,0.)) ;
#37121 = DIRECTION('',(0.,1.,0.)) ;
#37122 = DIRECTION('',(-1.,0.,0.)) ;
#37123 = DIRECTION('',(0.,1.,0.)) ;
#37124 = DIRECTION('',(1.,0.,0.)) ;
#37125 = DIRECTION('center_axis',(1.,0.,0.)) ;
#37126 = DIRECTION('ref_axis',(0.,0.,-1.)) ;
#37127 = DIRECTION('',(0.,0.,-1.)) ;
#37128 = DIRECTION('',(0.,0.,-1.)) ;
#37129 = DIRECTION('',(0.,-1.,0.)) ;
#37130 = DIRECTION('center_axis',(0.,-1.,0.)) ;
#37131 = DIRECTION('ref_axis',(0.,0.,-1.)) ;
#37132 = DIRECTION('',(0.,0.,-1.)) ;
#37133 = DIRECTION('',(1.,0.,0.)) ;
#37134 = DIRECTION('',(0.,0.,-1.)) ;
#37135 = DIRECTION('',(-1.,0.,0.)) ;
#37136 = DIRECTION('center_axis',(-1.,0.,0.)) ;
#37137 = DIRECTION('ref_axis',(0.,0.,1.)) ;
#37138 = DIRECTION('',(0.,0.,-1.)) ;
#37139 = DIRECTION('',(0.,-1.,0.)) ;
#37140 = DIRECTION('',(0.,1.,0.)) ;
#37141 = DIRECTION('center_axis',(0.,0.,1.)) ;
#37142 = DIRECTION('ref_axis',(1.,0.,0.)) ;
#37143 = DIRECTION('',(1.,0.,0.)) ;
#37144 = DIRECTION('center_axis',(0.,1.,0.)) ;
#37145 = DIRECTION('ref_axis',(0.,0.,1.)) ;
#37146 = DIRECTION('',(0.,0.,-1.)) ;
#37147 = DIRECTION('',(-1.,0.,0.)) ;
#37148 = DIRECTION('center_axis',(1.,0.,0.)) ;
#37149 = DIRECTION('ref_axis',(0.,0.,-1.)) ;
#37150 = DIRECTION('',(0.,1.,0.)) ;
#37151 = DIRECTION('center_axis',(1.,0.,0.)) ;
#37152 = DIRECTION('ref_axis',(0.,0.,-1.)) ;
#37153 = DIRECTION('center_axis',(1.,0.,0.)) ;
#37154 = DIRECTION('ref_axis',(0.,0.,-1.)) ;
#37155 = DIRECTION('',(1.,0.,0.)) ;
#37156 = DIRECTION('center_axis',(-1.,0.,0.)) ;
#37157 = DIRECTION('ref_axis',(0.,0.,-1.)) ;
#37158 = DIRECTION('center_axis',(0.,0.,1.)) ;
#37159 = DIRECTION('ref_axis',(1.,0.,0.)) ;
#37160 = DIRECTION('',(0.,1.,0.)) ;
#37161 = DIRECTION('',(-1.,0.,0.)) ;
#37162 = DIRECTION('',(0.,-1.,0.)) ;
#37163 = DIRECTION('',(1.,0.,0.)) ;
#37164 = DIRECTION('center_axis',(0.,1.,0.)) ;
#37165 = DIRECTION('ref_axis',(0.,0.,1.)) ;
#37166 = DIRECTION('',(0.,0.,-1.)) ;
#37167 = DIRECTION('',(-1.,0.,0.)) ;
#37168 = DIRECTION('',(0.,0.,-1.)) ;
#37169 = DIRECTION('center_axis',(1.,0.,0.)) ;
#37170 = DIRECTION('ref_axis',(0.,0.,-1.)) ;
#37171 = DIRECTION('',(0.,0.,-1.)) ;
#37172 = DIRECTION('',(0.,1.,0.)) ;
#37173 = DIRECTION('center_axis',(0.,-1.,0.)) ;
#37174 = DIRECTION('ref_axis',(0.,0.,-1.)) ;
#37175 = DIRECTION('',(0.,0.,-1.)) ;
#37176 = DIRECTION('',(1.,0.,0.)) ;
#37177 = DIRECTION('center_axis',(-1.,0.,0.)) ;
#37178 = DIRECTION('ref_axis',(0.,0.,1.)) ;
#37179 = DIRECTION('',(0.,-1.,0.)) ;
#37180 = DIRECTION('center_axis',(0.,0.,1.)) ;
#37181 = DIRECTION('ref_axis',(1.,0.,0.)) ;
#37182 = DIRECTION('center_axis',(0.,0.,1.)) ;
#37183 = DIRECTION('ref_axis',(1.,0.,0.)) ;
#37184 = DIRECTION('',(0.,0.,1.)) ;
#37185 = DIRECTION('center_axis',(0.,0.,-1.)) ;
#37186 = DIRECTION('ref_axis',(1.,0.,0.)) ;
#37187 = DIRECTION('center_axis',(0.,0.,1.)) ;
#37188 = DIRECTION('ref_axis',(1.,0.,0.)) ;
#37189 = DIRECTION('center_axis',(0.,0.,1.)) ;
#37190 = DIRECTION('ref_axis',(1.,0.,0.)) ;
#37191 = DIRECTION('',(0.,0.,1.)) ;
#37192 = DIRECTION('center_axis',(0.,0.,-1.)) ;
#37193 = DIRECTION('ref_axis',(1.,0.,0.)) ;
#37194 = DIRECTION('center_axis',(0.,0.,1.)) ;
#37195 = DIRECTION('ref_axis',(1.,0.,0.)) ;
#37196 = DIRECTION('center_axis',(0.,0.,1.)) ;
#37197 = DIRECTION('ref_axis',(1.,0.,0.)) ;
#37198 = DIRECTION('',(0.,0.,1.)) ;
#37199 = DIRECTION('center_axis',(0.,0.,-1.)) ;
#37200 = DIRECTION('ref_axis',(1.,0.,0.)) ;
#37201 = DIRECTION('center_axis',(0.,0.,1.)) ;
#37202 = DIRECTION('ref_axis',(1.,0.,0.)) ;
#37203 = DIRECTION('center_axis',(0.,0.,1.)) ;
#37204 = DIRECTION('ref_axis',(1.,0.,0.)) ;
#37205 = DIRECTION('',(0.,0.,1.)) ;
#37206 = DIRECTION('center_axis',(0.,0.,-1.)) ;
#37207 = DIRECTION('ref_axis',(1.,0.,0.)) ;
#37208 = DIRECTION('center_axis',(0.,0.,1.)) ;
#37209 = DIRECTION('ref_axis',(1.,0.,0.)) ;
#37210 = DIRECTION('center_axis',(0.,0.,1.)) ;
#37211 = DIRECTION('ref_axis',(1.,0.,0.)) ;
#37212 = DIRECTION('',(0.,0.,1.)) ;
#37213 = DIRECTION('center_axis',(0.,0.,-1.)) ;
#37214 = DIRECTION('ref_axis',(1.,0.,0.)) ;
#37215 = DIRECTION('',(0.,0.,-1.)) ;
#37216 = DIRECTION('center_axis',(0.,0.,-1.)) ;
#37217 = DIRECTION('ref_axis',(1.,0.,0.)) ;
#37218 = DIRECTION('',(0.,0.,1.)) ;
#37219 = DIRECTION('center_axis',(0.,0.,-1.)) ;
#37220 = DIRECTION('ref_axis',(1.,0.,0.)) ;
#37221 = DIRECTION('center_axis',(0.,0.,1.)) ;
#37222 = DIRECTION('ref_axis',(1.,0.,0.)) ;
#37223 = DIRECTION('',(-1.,0.,0.)) ;
#37224 = DIRECTION('',(0.,1.,0.)) ;
#37225 = DIRECTION('',(-1.,0.,0.)) ;
#37226 = DIRECTION('',(0.,-1.,0.)) ;
#37227 = DIRECTION('',(1.,0.,0.)) ;
#37228 = DIRECTION('',(0.,1.,0.)) ;
#37229 = DIRECTION('',(1.,0.,0.)) ;
#37230 = DIRECTION('center_axis',(0.,0.,-1.)) ;
#37231 = DIRECTION('ref_axis',(1.,0.,0.)) ;
#37232 = DIRECTION('center_axis',(0.,0.,-1.)) ;
#37233 = DIRECTION('ref_axis',(1.,0.,0.)) ;
#37234 = DIRECTION('center_axis',(0.,0.,-1.)) ;
#37235 = DIRECTION('ref_axis',(1.,0.,0.)) ;
#37236 = DIRECTION('',(1.,0.,0.)) ;
#37237 = DIRECTION('',(0.,-1.,0.)) ;
#37238 = DIRECTION('',(1.,0.,0.)) ;
#37239 = DIRECTION('',(0.,1.,0.)) ;
#37240 = DIRECTION('',(-1.,0.,0.)) ;
#37241 = DIRECTION('',(0.,-1.,0.)) ;
#37242 = DIRECTION('',(-1.,0.,0.)) ;
#37243 = DIRECTION('center_axis',(0.,1.,0.)) ;
#37244 = DIRECTION('ref_axis',(0.,0.,1.)) ;
#37245 = DIRECTION('',(1.,0.,0.)) ;
#37246 = DIRECTION('',(0.,0.,-1.)) ;
#37247 = DIRECTION('center_axis',(0.,0.,1.)) ;
#37248 = DIRECTION('ref_axis',(1.,0.,0.)) ;
#37249 = DIRECTION('center_axis',(0.,0.,-1.)) ;
#37250 = DIRECTION('ref_axis',(1.,0.,0.)) ;
#37251 = DIRECTION('',(-1.,0.,0.)) ;
#37252 = DIRECTION('',(0.,-1.,0.)) ;
#37253 = DIRECTION('',(1.,0.,0.)) ;
#37254 = DIRECTION('',(0.,1.,0.)) ;
#37255 = DIRECTION('',(-1.,0.,0.)) ;
#37256 = DIRECTION('center_axis',(0.,-1.,0.)) ;
#37257 = DIRECTION('ref_axis',(0.,0.,-1.)) ;
#37258 = DIRECTION('',(0.,0.,-1.)) ;
#37259 = DIRECTION('',(0.,0.,-1.)) ;
#37260 = DIRECTION('center_axis',(1.,0.,0.)) ;
#37261 = DIRECTION('ref_axis',(0.,0.,-1.)) ;
#37262 = DIRECTION('',(0.,0.,-1.)) ;
#37263 = DIRECTION('center_axis',(0.,-1.,0.)) ;
#37264 = DIRECTION('ref_axis',(0.,0.,-1.)) ;
#37265 = DIRECTION('',(0.,0.,1.)) ;
#37266 = DIRECTION('',(0.,0.,-1.)) ;
#37267 = DIRECTION('center_axis',(-1.,0.,0.)) ;
#37268 = DIRECTION('ref_axis',(0.,0.,1.)) ;
#37269 = DIRECTION('',(0.,0.,-1.)) ;
#37270 = DIRECTION('center_axis',(0.,0.,1.)) ;
#37271 = DIRECTION('ref_axis',(1.,0.,0.)) ;
#37272 = DIRECTION('',(1.,0.,0.)) ;
#37273 = DIRECTION('',(0.,1.,0.)) ;
#37274 = DIRECTION('',(-1.,0.,0.)) ;
#37275 = DIRECTION('',(0.,-1.,0.)) ;
#37276 = DIRECTION('center_axis',(0.,1.,0.)) ;
#37277 = DIRECTION('ref_axis',(0.,0.,1.)) ;
#37278 = DIRECTION('',(0.,0.,-1.)) ;
#37279 = DIRECTION('center_axis',(1.,0.,0.)) ;
#37280 = DIRECTION('ref_axis',(0.,0.,-1.)) ;
#37281 = DIRECTION('',(0.,0.,-1.)) ;
#37282 = DIRECTION('center_axis',(-1.,0.,0.)) ;
#37283 = DIRECTION('ref_axis',(0.,0.,1.)) ;
#37284 = DIRECTION('',(0.,0.,-1.)) ;
#37285 = DIRECTION('center_axis',(0.,0.,1.)) ;
#37286 = DIRECTION('ref_axis',(6.12323399573677E-17,-1.,0.)) ;
#37287 = DIRECTION('',(0.,0.,1.)) ;
#37288 = DIRECTION('center_axis',(0.,0.,1.)) ;
#37289 = DIRECTION('ref_axis',(1.,0.,0.)) ;
#37290 = DIRECTION('',(0.,0.,-1.)) ;
#37291 = DIRECTION('center_axis',(0.,0.,1.)) ;
#37292 = DIRECTION('ref_axis',(1.,0.,0.)) ;
#37293 = DIRECTION('',(0.,-1.,0.)) ;
#37294 = DIRECTION('',(-1.,0.,0.)) ;
#37295 = DIRECTION('',(0.,1.,0.)) ;
#37296 = DIRECTION('',(1.,0.,0.)) ;
#37297 = DIRECTION('center_axis',(0.,0.,1.)) ;
#37298 = DIRECTION('ref_axis',(1.,0.,0.)) ;
#37299 = DIRECTION('center_axis',(0.,0.,1.)) ;
#37300 = DIRECTION('ref_axis',(-1.83697019872103E-16,1.,0.)) ;
#37301 = DIRECTION('center_axis',(0.,1.,0.)) ;
#37302 = DIRECTION('ref_axis',(0.,0.,1.)) ;
#37303 = DIRECTION('',(0.,0.,-1.)) ;
#37304 = DIRECTION('',(0.,0.,-1.)) ;
#37305 = DIRECTION('center_axis',(1.,0.,0.)) ;
#37306 = DIRECTION('ref_axis',(0.,0.,-1.)) ;
#37307 = DIRECTION('',(0.,0.,-1.)) ;
#37308 = DIRECTION('center_axis',(0.,-1.,0.)) ;
#37309 = DIRECTION('ref_axis',(0.,0.,-1.)) ;
#37310 = DIRECTION('',(0.,0.,-1.)) ;
#37311 = DIRECTION('center_axis',(-1.,0.,0.)) ;
#37312 = DIRECTION('ref_axis',(0.,0.,1.)) ;
#37313 = DIRECTION('axis',(0.,0.,1.)) ;
#37314 = DIRECTION('refdir',(1.,0.,0.)) ;
#37315 = DIRECTION('center_axis',(0.,1.,0.)) ;
#37316 = DIRECTION('ref_axis',(0.,0.,1.)) ;
#37317 = DIRECTION('',(0.,0.,1.)) ;
#37318 = DIRECTION('',(-1.,0.,0.)) ;
#37319 = DIRECTION('',(0.,0.,-1.)) ;
#37320 = DIRECTION('',(1.,0.,0.)) ;
#37321 = DIRECTION('center_axis',(-1.,0.,0.)) ;
#37322 = DIRECTION('ref_axis',(0.,0.,1.)) ;
#37323 = DIRECTION('',(0.,-1.,0.)) ;
#37324 = DIRECTION('',(0.,0.,-1.)) ;
#37325 = DIRECTION('',(0.,1.,0.)) ;
#37326 = DIRECTION('center_axis',(0.,0.,1.)) ;
#37327 = DIRECTION('ref_axis',(1.,0.,0.)) ;
#37328 = DIRECTION('',(0.,-1.,0.)) ;
#37329 = DIRECTION('',(1.,0.,0.)) ;
#37330 = DIRECTION('',(0.,1.,0.)) ;
#37331 = DIRECTION('',(-1.,0.,0.)) ;
#37332 = DIRECTION('center_axis',(1.,0.,0.)) ;
#37333 = DIRECTION('ref_axis',(0.,0.,-1.)) ;
#37334 = DIRECTION('',(0.,1.,0.)) ;
#37335 = DIRECTION('',(0.,0.,-1.)) ;
#37336 = DIRECTION('',(0.,0.,-1.)) ;
#37337 = DIRECTION('',(0.,1.,0.)) ;
#37338 = DIRECTION('center_axis',(0.,0.,1.)) ;
#37339 = DIRECTION('ref_axis',(1.,0.,0.)) ;
#37340 = DIRECTION('',(-1.,0.,0.)) ;
#37341 = DIRECTION('',(1.,0.,0.)) ;
#37342 = DIRECTION('',(0.,-1.,0.)) ;
#37343 = DIRECTION('center_axis',(0.,1.,0.)) ;
#37344 = DIRECTION('ref_axis',(0.,0.,1.)) ;
#37345 = DIRECTION('',(-1.,0.,0.)) ;
#37346 = DIRECTION('',(0.,0.,-1.)) ;
#37347 = DIRECTION('center_axis',(0.,-1.,0.)) ;
#37348 = DIRECTION('ref_axis',(0.,0.,-1.)) ;
#37349 = DIRECTION('center_axis',(0.,0.,1.)) ;
#37350 = DIRECTION('ref_axis',(1.,0.,0.)) ;
#37351 = DIRECTION('center_axis',(0.,0.,1.)) ;
#37352 = DIRECTION('ref_axis',(1.,0.,0.)) ;
#37353 = DIRECTION('',(0.,0.,1.)) ;
#37354 = DIRECTION('center_axis',(0.,0.,-1.)) ;
#37355 = DIRECTION('ref_axis',(1.,0.,0.)) ;
#37356 = DIRECTION('center_axis',(0.,1.,0.)) ;
#37357 = DIRECTION('ref_axis',(0.,0.,1.)) ;
#37358 = DIRECTION('',(0.,0.,1.)) ;
#37359 = DIRECTION('',(-1.,0.,0.)) ;
#37360 = DIRECTION('',(0.,0.,-1.)) ;
#37361 = DIRECTION('',(1.,0.,0.)) ;
#37362 = DIRECTION('center_axis',(0.,-1.,0.)) ;
#37363 = DIRECTION('ref_axis',(0.,0.,-1.)) ;
#37364 = DIRECTION('',(0.,0.,-1.)) ;
#37365 = DIRECTION('',(1.,0.,0.)) ;
#37366 = DIRECTION('',(0.,0.,-1.)) ;
#37367 = DIRECTION('',(-1.,0.,0.)) ;
#37368 = DIRECTION('center_axis',(-1.,0.,0.)) ;
#37369 = DIRECTION('ref_axis',(0.,0.,1.)) ;
#37370 = DIRECTION('',(0.,-1.,0.)) ;
#37371 = DIRECTION('',(0.,1.,0.)) ;
#37372 = DIRECTION('center_axis',(-1.,0.,0.)) ;
#37373 = DIRECTION('ref_axis',(0.,0.,1.)) ;
#37374 = DIRECTION('',(0.,1.,0.)) ;
#37375 = DIRECTION('',(0.,0.,-1.)) ;
#37376 = DIRECTION('',(0.,-1.,0.)) ;
#37377 = DIRECTION('center_axis',(-1.,0.,0.)) ;
#37378 = DIRECTION('ref_axis',(0.,0.,1.)) ;
#37379 = DIRECTION('',(0.,-1.,0.)) ;
#37380 = DIRECTION('',(0.,0.,-1.)) ;
#37381 = DIRECTION('',(0.,1.,0.)) ;
#37382 = DIRECTION('center_axis',(0.,0.,1.)) ;
#37383 = DIRECTION('ref_axis',(1.,0.,0.)) ;
#37384 = DIRECTION('center_axis',(0.,0.,1.)) ;
#37385 = DIRECTION('ref_axis',(1.,0.,0.)) ;
#37386 = DIRECTION('',(0.,0.,1.)) ;
#37387 = DIRECTION('center_axis',(0.,0.,-1.)) ;
#37388 = DIRECTION('ref_axis',(1.,0.,0.)) ;
#37389 = DIRECTION('center_axis',(0.,1.,0.)) ;
#37390 = DIRECTION('ref_axis',(0.,0.,1.)) ;
#37391 = DIRECTION('',(0.,0.,-1.)) ;
#37392 = DIRECTION('',(-1.,0.,0.)) ;
#37393 = DIRECTION('',(0.,0.,-1.)) ;
#37394 = DIRECTION('',(1.,0.,0.)) ;
#37395 = DIRECTION('center_axis',(1.,0.,0.)) ;
#37396 = DIRECTION('ref_axis',(0.,0.,-1.)) ;
#37397 = DIRECTION('',(0.,0.,-1.)) ;
#37398 = DIRECTION('',(0.,1.,0.)) ;
#37399 = DIRECTION('',(0.,-1.,0.)) ;
#37400 = DIRECTION('center_axis',(0.,-1.,0.)) ;
#37401 = DIRECTION('ref_axis',(0.,0.,-1.)) ;
#37402 = DIRECTION('',(0.,0.,1.)) ;
#37403 = DIRECTION('',(1.,0.,0.)) ;
#37404 = DIRECTION('',(-1.,0.,0.)) ;
#37405 = DIRECTION('center_axis',(1.,0.,0.)) ;
#37406 = DIRECTION('ref_axis',(0.,0.,-1.)) ;
#37407 = DIRECTION('',(0.,-1.,0.)) ;
#37408 = DIRECTION('',(0.,0.,-1.)) ;
#37409 = DIRECTION('',(0.,1.,0.)) ;
#37410 = DIRECTION('center_axis',(1.,0.,0.)) ;
#37411 = DIRECTION('ref_axis',(0.,0.,-1.)) ;
#37412 = DIRECTION('',(0.,1.,0.)) ;
#37413 = DIRECTION('',(0.,0.,-1.)) ;
#37414 = DIRECTION('',(0.,-1.,0.)) ;
#37415 = DIRECTION('center_axis',(0.,0.,1.)) ;
#37416 = DIRECTION('ref_axis',(1.,0.,0.)) ;
#37417 = DIRECTION('center_axis',(0.,0.,1.)) ;
#37418 = DIRECTION('ref_axis',(1.,0.,0.)) ;
#37419 = DIRECTION('',(0.,0.,1.)) ;
#37420 = DIRECTION('center_axis',(0.,0.,-1.)) ;
#37421 = DIRECTION('ref_axis',(1.,0.,0.)) ;
#37422 = DIRECTION('center_axis',(0.,0.,1.)) ;
#37423 = DIRECTION('ref_axis',(1.,0.,0.)) ;
#37424 = DIRECTION('',(-1.,0.,0.)) ;
#37425 = DIRECTION('',(1.,0.,0.)) ;
#37426 = DIRECTION('center_axis',(0.,0.,1.)) ;
#37427 = DIRECTION('ref_axis',(1.,0.,0.)) ;
#37428 = DIRECTION('',(-1.,0.,0.)) ;
#37429 = DIRECTION('',(1.,0.,0.)) ;
#37430 = DIRECTION('center_axis',(0.,1.,0.)) ;
#37431 = DIRECTION('ref_axis',(0.,0.,1.)) ;
#37432 = DIRECTION('center_axis',(0.,-1.,0.)) ;
#37433 = DIRECTION('ref_axis',(0.,0.,-1.)) ;
#37434 = DIRECTION('axis',(0.,0.,1.)) ;
#37435 = DIRECTION('refdir',(1.,0.,0.)) ;
#37436 = DIRECTION('center_axis',(0.,0.,1.)) ;
#37437 = DIRECTION('ref_axis',(1.,0.,0.)) ;
#37438 = DIRECTION('',(-1.,0.,0.)) ;
#37439 = DIRECTION('',(0.,-1.,0.)) ;
#37440 = DIRECTION('',(1.,0.,0.)) ;
#37441 = DIRECTION('',(0.,1.,0.)) ;
#37442 = DIRECTION('center_axis',(1.,0.,0.)) ;
#37443 = DIRECTION('ref_axis',(0.,0.,-1.)) ;
#37444 = DIRECTION('',(0.,0.,1.)) ;
#37445 = DIRECTION('',(0.,0.,-1.)) ;
#37446 = DIRECTION('',(0.,1.,0.)) ;
#37447 = DIRECTION('center_axis',(0.,-1.,0.)) ;
#37448 = DIRECTION('ref_axis',(0.,0.,-1.)) ;
#37449 = DIRECTION('',(1.,0.,0.)) ;
#37450 = DIRECTION('',(0.,0.,-1.)) ;
#37451 = DIRECTION('center_axis',(-1.,0.,0.)) ;
#37452 = DIRECTION('ref_axis',(0.,0.,1.)) ;
#37453 = DIRECTION('',(0.,0.,-1.)) ;
#37454 = DIRECTION('',(0.,-1.,0.)) ;
#37455 = DIRECTION('center_axis',(0.,1.,0.)) ;
#37456 = DIRECTION('ref_axis',(0.,0.,1.)) ;
#37457 = DIRECTION('',(1.,0.,0.)) ;
#37458 = DIRECTION('',(0.,0.,-1.)) ;
#37459 = DIRECTION('',(-1.,0.,0.)) ;
#37460 = DIRECTION('',(0.,0.,1.)) ;
#37461 = DIRECTION('',(1.,0.,0.)) ;
#37462 = DIRECTION('',(0.,0.,-1.)) ;
#37463 = DIRECTION('',(-1.,0.,0.)) ;
#37464 = DIRECTION('',(0.,0.,1.)) ;
#37465 = DIRECTION('',(1.,0.,0.)) ;
#37466 = DIRECTION('',(0.,0.,-1.)) ;
#37467 = DIRECTION('',(-1.,0.,0.)) ;
#37468 = DIRECTION('',(0.,0.,1.)) ;
#37469 = DIRECTION('',(1.,0.,0.)) ;
#37470 = DIRECTION('',(0.,0.,-1.)) ;
#37471 = DIRECTION('',(-1.,0.,0.)) ;
#37472 = DIRECTION('',(0.,0.,1.)) ;
#37473 = DIRECTION('',(1.,0.,0.)) ;
#37474 = DIRECTION('',(0.,0.,-1.)) ;
#37475 = DIRECTION('',(-1.,0.,0.)) ;
#37476 = DIRECTION('',(0.,0.,1.)) ;
#37477 = DIRECTION('',(1.,0.,0.)) ;
#37478 = DIRECTION('',(0.,0.,-1.)) ;
#37479 = DIRECTION('',(-1.,0.,0.)) ;
#37480 = DIRECTION('',(0.,0.,1.)) ;
#37481 = DIRECTION('',(1.,0.,0.)) ;
#37482 = DIRECTION('',(0.,0.,-1.)) ;
#37483 = DIRECTION('',(-1.,0.,0.)) ;
#37484 = DIRECTION('',(0.,0.,1.)) ;
#37485 = DIRECTION('',(1.,0.,0.)) ;
#37486 = DIRECTION('',(0.,0.,-1.)) ;
#37487 = DIRECTION('',(-1.,0.,0.)) ;
#37488 = DIRECTION('',(0.,0.,1.)) ;
#37489 = DIRECTION('',(1.,0.,0.)) ;
#37490 = DIRECTION('',(0.,0.,-1.)) ;
#37491 = DIRECTION('',(-1.,0.,0.)) ;
#37492 = DIRECTION('',(0.,0.,-1.)) ;
#37493 = DIRECTION('',(1.,0.,0.)) ;
#37494 = DIRECTION('center_axis',(0.,-1.,0.)) ;
#37495 = DIRECTION('ref_axis',(0.,0.,-1.)) ;
#37496 = DIRECTION('',(1.,0.,0.)) ;
#37497 = DIRECTION('',(0.,0.,-1.)) ;
#37498 = DIRECTION('',(1.,0.,0.)) ;
#37499 = DIRECTION('',(0.,0.,-1.)) ;
#37500 = DIRECTION('center_axis',(-1.,0.,0.)) ;
#37501 = DIRECTION('ref_axis',(0.,0.,1.)) ;
#37502 = DIRECTION('',(0.,-1.,0.)) ;
#37503 = DIRECTION('',(0.,-1.,0.)) ;
#37504 = DIRECTION('center_axis',(0.,0.,1.)) ;
#37505 = DIRECTION('ref_axis',(1.,0.,0.)) ;
#37506 = DIRECTION('',(0.,1.,0.)) ;
#37507 = DIRECTION('center_axis',(1.,0.,0.)) ;
#37508 = DIRECTION('ref_axis',(0.,0.,-1.)) ;
#37509 = DIRECTION('',(0.,1.,0.)) ;
#37510 = DIRECTION('center_axis',(0.,0.,1.)) ;
#37511 = DIRECTION('ref_axis',(1.,0.,0.)) ;
#37512 = DIRECTION('',(0.,1.,0.)) ;
#37513 = DIRECTION('',(-1.,0.,0.)) ;
#37514 = DIRECTION('',(0.,-1.,0.)) ;
#37515 = DIRECTION('',(0.,1.,0.)) ;
#37516 = DIRECTION('',(1.,0.,0.)) ;
#37517 = DIRECTION('',(0.,-1.,0.)) ;
#37518 = DIRECTION('',(0.,1.,0.)) ;
#37519 = DIRECTION('',(1.,0.,0.)) ;
#37520 = DIRECTION('',(0.,-1.,0.)) ;
#37521 = DIRECTION('',(0.,1.,0.)) ;
#37522 = DIRECTION('',(1.,0.,0.)) ;
#37523 = DIRECTION('',(0.,-1.,0.)) ;
#37524 = DIRECTION('',(0.,1.,0.)) ;
#37525 = DIRECTION('',(1.,0.,0.)) ;
#37526 = DIRECTION('',(0.,-1.,0.)) ;
#37527 = DIRECTION('',(0.,1.,0.)) ;
#37528 = DIRECTION('',(1.,0.,0.)) ;
#37529 = DIRECTION('',(0.,-1.,0.)) ;
#37530 = DIRECTION('',(0.,1.,0.)) ;
#37531 = DIRECTION('',(1.,0.,0.)) ;
#37532 = DIRECTION('',(0.,-1.,0.)) ;
#37533 = DIRECTION('',(0.,1.,0.)) ;
#37534 = DIRECTION('',(1.,0.,0.)) ;
#37535 = DIRECTION('',(0.,-1.,0.)) ;
#37536 = DIRECTION('center_axis',(0.,0.,1.)) ;
#37537 = DIRECTION('ref_axis',(1.,0.,0.)) ;
#37538 = DIRECTION('',(0.,-1.,0.)) ;
#37539 = DIRECTION('',(1.,0.,0.)) ;
#37540 = DIRECTION('',(0.,1.,0.)) ;
#37541 = DIRECTION('center_axis',(1.,0.,0.)) ;
#37542 = DIRECTION('ref_axis',(0.,0.,-1.)) ;
#37543 = DIRECTION('',(0.,0.,-1.)) ;
#37544 = DIRECTION('center_axis',(0.,-1.,0.)) ;
#37545 = DIRECTION('ref_axis',(0.,0.,-1.)) ;
#37546 = DIRECTION('',(0.,0.,-1.)) ;
#37547 = DIRECTION('center_axis',(-1.,0.,0.)) ;
#37548 = DIRECTION('ref_axis',(0.,0.,1.)) ;
#37549 = DIRECTION('center_axis',(0.,-1.,0.)) ;
#37550 = DIRECTION('ref_axis',(0.,0.,-1.)) ;
#37551 = DIRECTION('',(0.,0.,-1.)) ;
#37552 = DIRECTION('',(1.,0.,0.)) ;
#37553 = DIRECTION('',(0.,0.,-1.)) ;
#37554 = DIRECTION('center_axis',(-1.,0.,0.)) ;
#37555 = DIRECTION('ref_axis',(0.,0.,1.)) ;
#37556 = DIRECTION('',(0.,-1.,0.)) ;
#37557 = DIRECTION('center_axis',(0.,0.,1.)) ;
#37558 = DIRECTION('ref_axis',(1.,0.,0.)) ;
#37559 = DIRECTION('',(0.,1.,0.)) ;
#37560 = DIRECTION('center_axis',(1.,0.,0.)) ;
#37561 = DIRECTION('ref_axis',(0.,0.,-1.)) ;
#37562 = DIRECTION('center_axis',(0.,0.,1.)) ;
#37563 = DIRECTION('ref_axis',(1.,0.,0.)) ;
#37564 = DIRECTION('',(0.,-1.,0.)) ;
#37565 = DIRECTION('',(1.,0.,0.)) ;
#37566 = DIRECTION('',(0.,1.,0.)) ;
#37567 = DIRECTION('center_axis',(1.,0.,0.)) ;
#37568 = DIRECTION('ref_axis',(0.,0.,-1.)) ;
#37569 = DIRECTION('',(0.,0.,-1.)) ;
#37570 = DIRECTION('center_axis',(0.,-1.,0.)) ;
#37571 = DIRECTION('ref_axis',(0.,0.,-1.)) ;
#37572 = DIRECTION('',(0.,0.,-1.)) ;
#37573 = DIRECTION('center_axis',(-1.,0.,0.)) ;
#37574 = DIRECTION('ref_axis',(0.,0.,1.)) ;
#37575 = DIRECTION('center_axis',(0.,-1.,0.)) ;
#37576 = DIRECTION('ref_axis',(0.,0.,-1.)) ;
#37577 = DIRECTION('',(0.,0.,-1.)) ;
#37578 = DIRECTION('',(1.,0.,0.)) ;
#37579 = DIRECTION('',(0.,0.,-1.)) ;
#37580 = DIRECTION('center_axis',(-1.,0.,0.)) ;
#37581 = DIRECTION('ref_axis',(0.,0.,1.)) ;
#37582 = DIRECTION('',(0.,-1.,0.)) ;
#37583 = DIRECTION('center_axis',(0.,0.,1.)) ;
#37584 = DIRECTION('ref_axis',(1.,0.,0.)) ;
#37585 = DIRECTION('',(0.,1.,0.)) ;
#37586 = DIRECTION('center_axis',(1.,0.,0.)) ;
#37587 = DIRECTION('ref_axis',(0.,0.,-1.)) ;
#37588 = DIRECTION('center_axis',(0.,0.,1.)) ;
#37589 = DIRECTION('ref_axis',(1.,0.,0.)) ;
#37590 = DIRECTION('',(0.,-1.,0.)) ;
#37591 = DIRECTION('',(1.,0.,0.)) ;
#37592 = DIRECTION('',(0.,1.,0.)) ;
#37593 = DIRECTION('center_axis',(1.,0.,0.)) ;
#37594 = DIRECTION('ref_axis',(0.,0.,-1.)) ;
#37595 = DIRECTION('',(0.,0.,-1.)) ;
#37596 = DIRECTION('center_axis',(0.,-1.,0.)) ;
#37597 = DIRECTION('ref_axis',(0.,0.,-1.)) ;
#37598 = DIRECTION('',(0.,0.,-1.)) ;
#37599 = DIRECTION('center_axis',(-1.,0.,0.)) ;
#37600 = DIRECTION('ref_axis',(0.,0.,1.)) ;
#37601 = DIRECTION('center_axis',(0.,-1.,0.)) ;
#37602 = DIRECTION('ref_axis',(0.,0.,-1.)) ;
#37603 = DIRECTION('',(0.,0.,-1.)) ;
#37604 = DIRECTION('',(1.,0.,0.)) ;
#37605 = DIRECTION('',(0.,0.,-1.)) ;
#37606 = DIRECTION('center_axis',(-1.,0.,0.)) ;
#37607 = DIRECTION('ref_axis',(0.,0.,1.)) ;
#37608 = DIRECTION('',(0.,-1.,0.)) ;
#37609 = DIRECTION('center_axis',(0.,0.,1.)) ;
#37610 = DIRECTION('ref_axis',(1.,0.,0.)) ;
#37611 = DIRECTION('',(0.,1.,0.)) ;
#37612 = DIRECTION('center_axis',(1.,0.,0.)) ;
#37613 = DIRECTION('ref_axis',(0.,0.,-1.)) ;
#37614 = DIRECTION('center_axis',(0.,0.,1.)) ;
#37615 = DIRECTION('ref_axis',(1.,0.,0.)) ;
#37616 = DIRECTION('',(0.,-1.,0.)) ;
#37617 = DIRECTION('',(1.,0.,0.)) ;
#37618 = DIRECTION('',(0.,1.,0.)) ;
#37619 = DIRECTION('center_axis',(1.,0.,0.)) ;
#37620 = DIRECTION('ref_axis',(0.,0.,-1.)) ;
#37621 = DIRECTION('',(0.,0.,-1.)) ;
#37622 = DIRECTION('center_axis',(0.,-1.,0.)) ;
#37623 = DIRECTION('ref_axis',(0.,0.,-1.)) ;
#37624 = DIRECTION('',(0.,0.,-1.)) ;
#37625 = DIRECTION('center_axis',(-1.,0.,0.)) ;
#37626 = DIRECTION('ref_axis',(0.,0.,1.)) ;
#37627 = DIRECTION('center_axis',(0.,0.,1.)) ;
#37628 = DIRECTION('ref_axis',(1.,0.,0.)) ;
#37629 = DIRECTION('',(0.,-1.,0.)) ;
#37630 = DIRECTION('',(0.,1.,0.)) ;
#37631 = DIRECTION('',(1.,0.,0.)) ;
#37632 = DIRECTION('center_axis',(1.,0.,0.)) ;
#37633 = DIRECTION('ref_axis',(0.,0.,-1.)) ;
#37634 = DIRECTION('',(0.,0.,-1.)) ;
#37635 = DIRECTION('center_axis',(0.,-1.,0.)) ;
#37636 = DIRECTION('ref_axis',(0.,0.,-1.)) ;
#37637 = DIRECTION('',(0.,0.,-1.)) ;
#37638 = DIRECTION('center_axis',(-1.,0.,0.)) ;
#37639 = DIRECTION('ref_axis',(0.,0.,1.)) ;
#37640 = DIRECTION('axis',(0.,0.,1.)) ;
#37641 = DIRECTION('refdir',(1.,0.,0.)) ;
#37642 = DIRECTION('center_axis',(0.,0.,1.)) ;
#37643 = DIRECTION('ref_axis',(1.,0.,0.)) ;
#37644 = DIRECTION('center_axis',(0.,0.,1.)) ;
#37645 = DIRECTION('ref_axis',(1.,0.,0.)) ;
#37646 = DIRECTION('',(0.,0.,1.)) ;
#37647 = DIRECTION('center_axis',(0.,0.,-1.)) ;
#37648 = DIRECTION('ref_axis',(1.,0.,0.)) ;
#37649 = DIRECTION('center_axis',(0.,0.,1.)) ;
#37650 = DIRECTION('ref_axis',(1.,0.,0.)) ;
#37651 = DIRECTION('center_axis',(0.,0.,1.)) ;
#37652 = DIRECTION('ref_axis',(1.,0.,0.)) ;
#37653 = DIRECTION('',(0.,0.,1.)) ;
#37654 = DIRECTION('center_axis',(0.,0.,-1.)) ;
#37655 = DIRECTION('ref_axis',(1.,0.,0.)) ;
#37656 = DIRECTION('center_axis',(0.,0.,1.)) ;
#37657 = DIRECTION('ref_axis',(1.,0.,0.)) ;
#37658 = DIRECTION('center_axis',(0.,0.,1.)) ;
#37659 = DIRECTION('ref_axis',(1.,0.,0.)) ;
#37660 = DIRECTION('',(0.,0.,1.)) ;
#37661 = DIRECTION('center_axis',(0.,0.,-1.)) ;
#37662 = DIRECTION('ref_axis',(1.,0.,0.)) ;
#37663 = DIRECTION('center_axis',(0.,0.,1.)) ;
#37664 = DIRECTION('ref_axis',(1.,0.,0.)) ;
#37665 = DIRECTION('center_axis',(0.,0.,1.)) ;
#37666 = DIRECTION('ref_axis',(1.,0.,0.)) ;
#37667 = DIRECTION('',(0.,0.,1.)) ;
#37668 = DIRECTION('center_axis',(0.,0.,-1.)) ;
#37669 = DIRECTION('ref_axis',(1.,0.,0.)) ;
#37670 = DIRECTION('center_axis',(0.,0.,1.)) ;
#37671 = DIRECTION('ref_axis',(6.12323399573677E-17,-1.,0.)) ;
#37672 = DIRECTION('',(0.,0.,1.)) ;
#37673 = DIRECTION('center_axis',(0.,0.,1.)) ;
#37674 = DIRECTION('ref_axis',(1.,0.,0.)) ;
#37675 = DIRECTION('',(0.,0.,-1.)) ;
#37676 = DIRECTION('center_axis',(0.,0.,-1.)) ;
#37677 = DIRECTION('ref_axis',(1.,0.,0.)) ;
#37678 = DIRECTION('center_axis',(0.,0.,1.)) ;
#37679 = DIRECTION('ref_axis',(1.,0.,0.)) ;
#37680 = DIRECTION('',(0.,-1.,0.)) ;
#37681 = DIRECTION('',(-1.,0.,0.)) ;
#37682 = DIRECTION('',(0.,1.,0.)) ;
#37683 = DIRECTION('',(1.,0.,0.)) ;
#37684 = DIRECTION('center_axis',(0.,0.,1.)) ;
#37685 = DIRECTION('ref_axis',(1.,0.,0.)) ;
#37686 = DIRECTION('center_axis',(0.,0.,1.)) ;
#37687 = DIRECTION('ref_axis',(-1.83697019872103E-16,1.,0.)) ;
#37688 = DIRECTION('center_axis',(0.,0.,1.)) ;
#37689 = DIRECTION('ref_axis',(1.,0.,0.)) ;
#37690 = DIRECTION('center_axis',(0.,0.,1.)) ;
#37691 = DIRECTION('ref_axis',(1.,0.,0.)) ;
#37692 = DIRECTION('center_axis',(0.,0.,1.)) ;
#37693 = DIRECTION('ref_axis',(1.,0.,0.)) ;
#37694 = DIRECTION('center_axis',(0.,0.,1.)) ;
#37695 = DIRECTION('ref_axis',(1.,0.,0.)) ;
#37696 = DIRECTION('',(0.721387321030952,8.83444673646039E-17,-0.692531828189713)) ;
#37697 = DIRECTION('center_axis',(0.,0.,-1.)) ;
#37698 = DIRECTION('ref_axis',(1.,0.,0.)) ;
#37699 = DIRECTION('center_axis',(0.,0.,-1.)) ;
#37700 = DIRECTION('ref_axis',(1.,0.,0.)) ;
#37701 = DIRECTION('center_axis',(0.,0.,1.)) ;
#37702 = DIRECTION('ref_axis',(1.,0.,0.)) ;
#37703 = DIRECTION('',(0.,1.,0.)) ;
#37704 = DIRECTION('',(-1.,0.,0.)) ;
#37705 = DIRECTION('',(0.,-1.,0.)) ;
#37706 = DIRECTION('',(1.,0.,0.)) ;
#37707 = DIRECTION('center_axis',(0.,1.,0.)) ;
#37708 = DIRECTION('ref_axis',(0.,0.,1.)) ;
#37709 = DIRECTION('',(0.,0.,-1.)) ;
#37710 = DIRECTION('',(0.,0.,-1.)) ;
#37711 = DIRECTION('center_axis',(1.,0.,0.)) ;
#37712 = DIRECTION('ref_axis',(0.,0.,-1.)) ;
#37713 = DIRECTION('',(0.,0.,-1.)) ;
#37714 = DIRECTION('center_axis',(0.,-1.,0.)) ;
#37715 = DIRECTION('ref_axis',(0.,0.,-1.)) ;
#37716 = DIRECTION('',(0.,0.,-1.)) ;
#37717 = DIRECTION('center_axis',(-1.,0.,0.)) ;
#37718 = DIRECTION('ref_axis',(0.,0.,1.)) ;
#37719 = DIRECTION('center_axis',(0.,0.,1.)) ;
#37720 = DIRECTION('ref_axis',(1.,0.,0.)) ;
#37721 = DIRECTION('',(-0.721387321030951,-8.83444673646039E-17,0.692531828189713)) ;
#37722 = DIRECTION('center_axis',(0.,0.,-1.)) ;
#37723 = DIRECTION('ref_axis',(1.,0.,0.)) ;
#37724 = DIRECTION('center_axis',(0.,0.,1.)) ;
#37725 = DIRECTION('ref_axis',(1.,0.,0.)) ;
#37726 = DIRECTION('axis',(0.,0.,1.)) ;
#37727 = DIRECTION('refdir',(1.,0.,0.)) ;
#37728 = DIRECTION('center_axis',(0.,0.,1.)) ;
#37729 = DIRECTION('ref_axis',(1.,0.,0.)) ;
#37730 = DIRECTION('center_axis',(0.,0.,1.)) ;
#37731 = DIRECTION('ref_axis',(1.,0.,0.)) ;
#37732 = DIRECTION('',(0.,0.,1.)) ;
#37733 = DIRECTION('center_axis',(0.,0.,1.)) ;
#37734 = DIRECTION('ref_axis',(1.,0.,0.)) ;
#37735 = DIRECTION('center_axis',(0.,0.,1.)) ;
#37736 = DIRECTION('ref_axis',(1.,0.,0.)) ;
#37737 = DIRECTION('',(0.,0.,1.)) ;
#37738 = DIRECTION('center_axis',(0.,0.,-1.)) ;
#37739 = DIRECTION('ref_axis',(1.,0.,0.)) ;
#37740 = DIRECTION('center_axis',(0.,0.,1.)) ;
#37741 = DIRECTION('ref_axis',(1.,0.,0.)) ;
#37742 = DIRECTION('center_axis',(0.,0.,1.)) ;
#37743 = DIRECTION('ref_axis',(1.,0.,0.)) ;
#37744 = DIRECTION('',(0.,0.,-1.)) ;
#37745 = DIRECTION('center_axis',(0.,0.,-1.)) ;
#37746 = DIRECTION('ref_axis',(1.,0.,0.)) ;
#37747 = DIRECTION('center_axis',(0.,0.,-1.)) ;
#37748 = DIRECTION('ref_axis',(-1.,0.,0.)) ;
#37749 = DIRECTION('center_axis',(0.,0.,1.)) ;
#37750 = DIRECTION('ref_axis',(1.,0.,0.)) ;
#37751 = DIRECTION('center_axis',(0.,0.,-1.)) ;
#37752 = DIRECTION('ref_axis',(1.,0.,0.)) ;
#37753 = DIRECTION('center_axis',(0.,0.,-1.)) ;
#37754 = DIRECTION('ref_axis',(1.,0.,0.)) ;
#37755 = DIRECTION('center_axis',(0.,0.,1.)) ;
#37756 = DIRECTION('ref_axis',(1.,0.,0.)) ;
#37757 = DIRECTION('center_axis',(0.,0.,1.)) ;
#37758 = DIRECTION('ref_axis',(-1.,0.,0.)) ;
#37759 = DIRECTION('center_axis',(0.,0.,1.)) ;
#37760 = DIRECTION('ref_axis',(1.,0.,0.)) ;
#37761 = DIRECTION('center_axis',(0.,0.,-1.)) ;
#37762 = DIRECTION('ref_axis',(1.,0.,0.)) ;
#37763 = DIRECTION('center_axis',(0.,0.,1.)) ;
#37764 = DIRECTION('ref_axis',(1.,0.,0.)) ;
#37765 = DIRECTION('',(-0.192745304030928,2.36044919632159E-17,0.981248820521087)) ;
#37766 = DIRECTION('center_axis',(0.,0.,1.)) ;
#37767 = DIRECTION('ref_axis',(1.,0.,0.)) ;
#37768 = DIRECTION('',(0.192745304030928,-2.36044919632159E-17,-0.981248820521087)) ;
#37769 = DIRECTION('axis',(0.,0.,1.)) ;
#37770 = DIRECTION('refdir',(1.,0.,0.)) ;
#37771 = DIRECTION('center_axis',(0.,1.,0.)) ;
#37772 = DIRECTION('ref_axis',(1.,0.,0.)) ;
#37773 = DIRECTION('center_axis',(0.,1.,0.)) ;
#37774 = DIRECTION('ref_axis',(1.,0.,0.)) ;
#37775 = DIRECTION('',(0.,1.,0.)) ;
#37776 = DIRECTION('center_axis',(0.,-1.,0.)) ;
#37777 = DIRECTION('ref_axis',(1.,0.,0.)) ;
#37778 = DIRECTION('center_axis',(0.,1.,0.)) ;
#37779 = DIRECTION('ref_axis',(1.,0.,0.)) ;
#37780 = DIRECTION('center_axis',(0.,1.,0.)) ;
#37781 = DIRECTION('ref_axis',(1.,0.,0.)) ;
#37782 = DIRECTION('',(0.,1.,0.)) ;
#37783 = DIRECTION('center_axis',(0.,-1.,0.)) ;
#37784 = DIRECTION('ref_axis',(1.,0.,0.)) ;
#37785 = DIRECTION('center_axis',(0.,1.,0.)) ;
#37786 = DIRECTION('ref_axis',(1.,0.,0.)) ;
#37787 = DIRECTION('center_axis',(0.,1.,0.)) ;
#37788 = DIRECTION('ref_axis',(1.,0.,0.)) ;
#37789 = DIRECTION('',(0.,1.,0.)) ;
#37790 = DIRECTION('center_axis',(0.,-1.,0.)) ;
#37791 = DIRECTION('ref_axis',(1.,0.,0.)) ;
#37792 = DIRECTION('center_axis',(0.,1.,0.)) ;
#37793 = DIRECTION('ref_axis',(1.,0.,0.)) ;
#37794 = DIRECTION('center_axis',(0.,1.,0.)) ;
#37795 = DIRECTION('ref_axis',(1.,0.,0.)) ;
#37796 = DIRECTION('',(0.,1.,0.)) ;
#37797 = DIRECTION('center_axis',(0.,-1.,0.)) ;
#37798 = DIRECTION('ref_axis',(1.,0.,0.)) ;
#37799 = DIRECTION('center_axis',(0.,1.,0.)) ;
#37800 = DIRECTION('ref_axis',(1.,0.,0.)) ;
#37801 = DIRECTION('center_axis',(0.,1.,0.)) ;
#37802 = DIRECTION('ref_axis',(1.,0.,0.)) ;
#37803 = DIRECTION('',(0.,1.,0.)) ;
#37804 = DIRECTION('center_axis',(0.,-1.,0.)) ;
#37805 = DIRECTION('ref_axis',(1.,0.,0.)) ;
#37806 = DIRECTION('center_axis',(0.,1.,0.)) ;
#37807 = DIRECTION('ref_axis',(1.,0.,0.)) ;
#37808 = DIRECTION('center_axis',(0.,1.,0.)) ;
#37809 = DIRECTION('ref_axis',(1.,0.,0.)) ;
#37810 = DIRECTION('',(0.,1.,0.)) ;
#37811 = DIRECTION('center_axis',(0.,-1.,0.)) ;
#37812 = DIRECTION('ref_axis',(1.,0.,0.)) ;
#37813 = DIRECTION('center_axis',(0.,1.,0.)) ;
#37814 = DIRECTION('ref_axis',(1.,0.,0.)) ;
#37815 = DIRECTION('center_axis',(0.,1.,0.)) ;
#37816 = DIRECTION('ref_axis',(1.,0.,0.)) ;
#37817 = DIRECTION('',(0.,1.,0.)) ;
#37818 = DIRECTION('center_axis',(0.,-1.,0.)) ;
#37819 = DIRECTION('ref_axis',(1.,0.,0.)) ;
#37820 = DIRECTION('center_axis',(0.,1.,0.)) ;
#37821 = DIRECTION('ref_axis',(1.,0.,0.)) ;
#37822 = DIRECTION('center_axis',(0.,1.,0.)) ;
#37823 = DIRECTION('ref_axis',(1.,0.,0.)) ;
#37824 = DIRECTION('',(0.,1.,0.)) ;
#37825 = DIRECTION('center_axis',(0.,-1.,0.)) ;
#37826 = DIRECTION('ref_axis',(1.,0.,0.)) ;
#37827 = DIRECTION('center_axis',(0.,0.,1.)) ;
#37828 = DIRECTION('ref_axis',(1.,0.,0.)) ;
#37829 = DIRECTION('',(1.,0.,0.)) ;
#37830 = DIRECTION('',(0.,-1.,0.)) ;
#37831 = DIRECTION('',(-1.,0.,0.)) ;
#37832 = DIRECTION('',(0.,1.,0.)) ;
#37833 = DIRECTION('center_axis',(0.,1.,0.)) ;
#37834 = DIRECTION('ref_axis',(1.,0.,0.)) ;
#37835 = DIRECTION('center_axis',(0.,1.,0.)) ;
#37836 = DIRECTION('ref_axis',(1.,0.,0.)) ;
#37837 = DIRECTION('center_axis',(0.,-1.,0.)) ;
#37838 = DIRECTION('ref_axis',(-1.,0.,0.)) ;
#37839 = DIRECTION('center_axis',(0.,-1.,0.)) ;
#37840 = DIRECTION('ref_axis',(1.,0.,0.)) ;
#37841 = DIRECTION('center_axis',(0.,1.,0.)) ;
#37842 = DIRECTION('ref_axis',(6.12323399573677E-17,0.,1.)) ;
#37843 = DIRECTION('axis',(0.,0.,1.)) ;
#37844 = DIRECTION('refdir',(1.,0.,0.)) ;
#37845 = DIRECTION('center_axis',(0.,1.,0.)) ;
#37846 = DIRECTION('ref_axis',(1.,0.,0.)) ;
#37847 = DIRECTION('center_axis',(0.,1.,0.)) ;
#37848 = DIRECTION('ref_axis',(1.,0.,0.)) ;
#37849 = DIRECTION('center_axis',(0.,1.,0.)) ;
#37850 = DIRECTION('ref_axis',(1.,0.,0.)) ;
#37851 = DIRECTION('',(0.,-1.,0.)) ;
#37852 = DIRECTION('center_axis',(0.,-1.,0.)) ;
#37853 = DIRECTION('ref_axis',(1.,0.,0.)) ;
#37854 = DIRECTION('center_axis',(0.,-1.,0.)) ;
#37855 = DIRECTION('ref_axis',(-1.,0.,0.)) ;
#37856 = DIRECTION('center_axis',(0.,1.,0.)) ;
#37857 = DIRECTION('ref_axis',(0.,0.,1.)) ;
#37858 = DIRECTION('',(0.,0.,-1.)) ;
#37859 = DIRECTION('',(1.,0.,0.)) ;
#37860 = DIRECTION('',(0.,0.,-1.)) ;
#37861 = DIRECTION('center_axis',(0.,1.,0.)) ;
#37862 = DIRECTION('ref_axis',(0.,0.,1.)) ;
#37863 = DIRECTION('',(0.,0.,-1.)) ;
#37864 = DIRECTION('',(1.,0.,0.)) ;
#37865 = DIRECTION('',(0.,0.,-1.)) ;
#37866 = DIRECTION('center_axis',(0.,0.,1.)) ;
#37867 = DIRECTION('ref_axis',(1.,0.,0.)) ;
#37868 = DIRECTION('center_axis',(0.,0.,-1.)) ;
#37869 = DIRECTION('ref_axis',(1.,0.,0.)) ;
#37870 = DIRECTION('',(0.,0.,1.)) ;
#37871 = DIRECTION('center_axis',(0.,0.,1.)) ;
#37872 = DIRECTION('ref_axis',(1.,0.,0.)) ;
#37873 = DIRECTION('center_axis',(0.,0.,-1.)) ;
#37874 = DIRECTION('ref_axis',(-1.,0.,0.)) ;
#37875 = DIRECTION('center_axis',(0.,0.,1.)) ;
#37876 = DIRECTION('ref_axis',(1.,0.,0.)) ;
#37877 = DIRECTION('center_axis',(0.,0.,1.)) ;
#37878 = DIRECTION('ref_axis',(1.,0.,0.)) ;
#37879 = DIRECTION('center_axis',(0.,0.,1.)) ;
#37880 = DIRECTION('ref_axis',(1.,0.,0.)) ;
#37881 = DIRECTION('center_axis',(0.,0.,1.)) ;
#37882 = DIRECTION('ref_axis',(1.,0.,0.)) ;
#37883 = DIRECTION('',(0.,0.,1.)) ;
#37884 = DIRECTION('center_axis',(0.,1.,0.)) ;
#37885 = DIRECTION('ref_axis',(1.,0.,0.)) ;
#37886 = DIRECTION('center_axis',(0.,1.,0.)) ;
#37887 = DIRECTION('ref_axis',(1.,0.,0.)) ;
#37888 = DIRECTION('',(0.,1.,0.)) ;
#37889 = DIRECTION('center_axis',(0.,-1.,0.)) ;
#37890 = DIRECTION('ref_axis',(1.,0.,0.)) ;
#37891 = DIRECTION('center_axis',(0.,0.,1.)) ;
#37892 = DIRECTION('ref_axis',(1.,0.,0.)) ;
#37893 = DIRECTION('',(0.,-1.,0.)) ;
#37894 = DIRECTION('',(-1.,0.,0.)) ;
#37895 = DIRECTION('',(0.,1.,0.)) ;
#37896 = DIRECTION('',(1.,0.,0.)) ;
#37897 = DIRECTION('',(1.,0.,0.)) ;
#37898 = DIRECTION('',(0.,1.,0.)) ;
#37899 = DIRECTION('',(-1.,0.,0.)) ;
#37900 = DIRECTION('',(0.,-1.,0.)) ;
#37901 = DIRECTION('center_axis',(0.,0.,1.)) ;
#37902 = DIRECTION('ref_axis',(1.,0.,0.)) ;
#37903 = DIRECTION('',(0.,1.,0.)) ;
#37904 = DIRECTION('',(-1.,0.,0.)) ;
#37905 = DIRECTION('',(0.,-1.,0.)) ;
#37906 = DIRECTION('',(1.,0.,0.)) ;
#37907 = DIRECTION('',(0.,1.,0.)) ;
#37908 = DIRECTION('',(0.,-1.,0.)) ;
#37909 = DIRECTION('',(-1.,0.,0.)) ;
#37910 = DIRECTION('center_axis',(0.,1.,0.)) ;
#37911 = DIRECTION('ref_axis',(0.,0.,1.)) ;
#37912 = DIRECTION('',(0.,0.,-1.)) ;
#37913 = DIRECTION('',(0.,0.,-1.)) ;
#37914 = DIRECTION('center_axis',(1.,0.,0.)) ;
#37915 = DIRECTION('ref_axis',(0.,0.,-1.)) ;
#37916 = DIRECTION('',(0.,0.,-1.)) ;
#37917 = DIRECTION('center_axis',(0.,-1.,0.)) ;
#37918 = DIRECTION('ref_axis',(0.,0.,-1.)) ;
#37919 = DIRECTION('',(0.,0.,-1.)) ;
#37920 = DIRECTION('center_axis',(-1.,0.,0.)) ;
#37921 = DIRECTION('ref_axis',(0.,0.,1.)) ;
#37922 = DIRECTION('center_axis',(1.,0.,0.)) ;
#37923 = DIRECTION('ref_axis',(0.,0.,-1.)) ;
#37924 = DIRECTION('',(0.,-1.,0.)) ;
#37925 = DIRECTION('',(0.,0.,-1.)) ;
#37926 = DIRECTION('center_axis',(-1.,0.,0.)) ;
#37927 = DIRECTION('ref_axis',(0.,0.,1.)) ;
#37928 = DIRECTION('',(0.,0.,-1.)) ;
#37929 = DIRECTION('',(0.,1.,0.)) ;
#37930 = DIRECTION('center_axis',(0.,0.,1.)) ;
#37931 = DIRECTION('ref_axis',(1.,0.,0.)) ;
#37932 = DIRECTION('',(-1.,0.,0.)) ;
#37933 = DIRECTION('center_axis',(0.,-1.,0.)) ;
#37934 = DIRECTION('ref_axis',(0.,0.,-1.)) ;
#37935 = DIRECTION('center_axis',(0.,1.,0.)) ;
#37936 = DIRECTION('ref_axis',(0.,0.,1.)) ;
#37937 = DIRECTION('',(0.,0.,-1.)) ;
#37938 = DIRECTION('',(-1.,0.,0.)) ;
#37939 = DIRECTION('',(0.,0.,-1.)) ;
#37940 = DIRECTION('center_axis',(1.,0.,0.)) ;
#37941 = DIRECTION('ref_axis',(0.,0.,-1.)) ;
#37942 = DIRECTION('',(0.,0.,-1.)) ;
#37943 = DIRECTION('',(0.,1.,0.)) ;
#37944 = DIRECTION('center_axis',(0.,-1.,0.)) ;
#37945 = DIRECTION('ref_axis',(0.,0.,-1.)) ;
#37946 = DIRECTION('',(0.,0.,-1.)) ;
#37947 = DIRECTION('',(1.,0.,0.)) ;
#37948 = DIRECTION('center_axis',(-1.,0.,0.)) ;
#37949 = DIRECTION('ref_axis',(0.,0.,1.)) ;
#37950 = DIRECTION('',(0.,-1.,0.)) ;
#37951 = DIRECTION('center_axis',(0.,0.,1.)) ;
#37952 = DIRECTION('ref_axis',(1.,0.,0.)) ;
#37953 = DIRECTION('axis',(0.,0.,1.)) ;
#37954 = DIRECTION('refdir',(1.,0.,0.)) ;
#37955 = DIRECTION('center_axis',(0.,0.,1.)) ;
#37956 = DIRECTION('ref_axis',(1.,0.,0.)) ;
#37957 = DIRECTION('center_axis',(0.,0.,1.)) ;
#37958 = DIRECTION('ref_axis',(1.,0.,0.)) ;
#37959 = DIRECTION('',(0.,0.,-1.)) ;
#37960 = DIRECTION('center_axis',(0.,0.,-1.)) ;
#37961 = DIRECTION('ref_axis',(1.,0.,0.)) ;
#37962 = DIRECTION('center_axis',(0.,0.,-1.)) ;
#37963 = DIRECTION('ref_axis',(-1.,0.,0.)) ;
#37964 = DIRECTION('center_axis',(0.,0.,1.)) ;
#37965 = DIRECTION('ref_axis',(1.,0.,0.)) ;
#37966 = DIRECTION('center_axis',(0.,-1.,0.)) ;
#37967 = DIRECTION('ref_axis',(-1.,0.,0.)) ;
#37968 = DIRECTION('axis',(0.,0.,1.)) ;
#37969 = DIRECTION('refdir',(1.,0.,0.)) ;
#37970 = DIRECTION('center_axis',(0.,1.,0.)) ;
#37971 = DIRECTION('ref_axis',(1.,0.,0.)) ;
#37972 = DIRECTION('center_axis',(0.,1.,0.)) ;
#37973 = DIRECTION('ref_axis',(1.,0.,0.)) ;
#37974 = DIRECTION('center_axis',(0.,-1.,0.)) ;
#37975 = DIRECTION('ref_axis',(1.,0.,0.)) ;
#37976 = DIRECTION('center_axis',(0.,1.,0.)) ;
#37977 = DIRECTION('ref_axis',(1.,0.,0.)) ;
#37978 = DIRECTION('',(0.,-1.,0.)) ;
#37979 = DIRECTION('center_axis',(0.,-1.,0.)) ;
#37980 = DIRECTION('ref_axis',(1.,0.,0.)) ;
#37981 = DIRECTION('center_axis',(0.,-1.,0.)) ;
#37982 = DIRECTION('ref_axis',(-1.,0.,0.)) ;
#37983 = DIRECTION('center_axis',(0.,1.,0.)) ;
#37984 = DIRECTION('ref_axis',(1.,0.,0.)) ;
#37985 = DIRECTION('center_axis',(0.,1.,0.)) ;
#37986 = DIRECTION('ref_axis',(1.,0.,0.)) ;
#37987 = DIRECTION('',(0.,-1.,0.)) ;
#37988 = DIRECTION('center_axis',(0.,1.,0.)) ;
#37989 = DIRECTION('ref_axis',(1.,0.,0.)) ;
#37990 = DIRECTION('axis',(0.,0.,1.)) ;
#37991 = DIRECTION('refdir',(1.,0.,0.)) ;
#37992 = DIRECTION('center_axis',(0.,0.,1.)) ;
#37993 = DIRECTION('ref_axis',(1.,0.,0.)) ;
#37994 = DIRECTION('center_axis',(0.,1.,0.)) ;
#37995 = DIRECTION('ref_axis',(-1.,0.,0.)) ;
#37996 = DIRECTION('center_axis',(0.,0.,1.)) ;
#37997 = DIRECTION('ref_axis',(1.,0.,0.)) ;
#37998 = DIRECTION('center_axis',(-1.22464679914737E-16,1.,0.)) ;
#37999 = DIRECTION('ref_axis',(-1.,-1.22464679914737E-16,0.)) ;
#38000 = DIRECTION('center_axis',(0.,0.,1.)) ;
#38001 = DIRECTION('ref_axis',(1.,0.,0.)) ;
#38002 = DIRECTION('center_axis',(-1.22464679914737E-16,1.,0.)) ;
#38003 = DIRECTION('ref_axis',(-1.,-1.22464679914737E-16,0.)) ;
#38004 = DIRECTION('center_axis',(0.,-1.22927471708385E-18,1.)) ;
#38005 = DIRECTION('ref_axis',(-0.99979846524302,-0.0200755796355278,0.)) ;
#38006 = DIRECTION('center_axis',(0.999200958721789,0.,-0.0399680383488722)) ;
#38007 = DIRECTION('ref_axis',(0.0399680383488744,0.,0.999200958721789)) ;
#38008 = DIRECTION('center_axis',(0.999200958721789,0.,-0.0399680383488722)) ;
#38009 = DIRECTION('ref_axis',(0.0399680383488722,0.,0.999200958721789)) ;
#38010 = DIRECTION('center_axis',(-0.999200958721789,0.,0.0399680383488722)) ;
#38011 = DIRECTION('ref_axis',(0.0399680383488744,0.,0.999200958721789)) ;
#38012 = DIRECTION('',(0.999200958721789,0.,-0.0399680383488722)) ;
#38013 = DIRECTION('center_axis',(0.,0.,1.)) ;
#38014 = DIRECTION('ref_axis',(1.,0.,0.)) ;
#38015 = DIRECTION('center_axis',(0.,0.,1.)) ;
#38016 = DIRECTION('ref_axis',(1.,0.,0.)) ;
#38017 = DIRECTION('center_axis',(-0.999200958721789,0.,0.0399680383488714)) ;
#38018 = DIRECTION('ref_axis',(0.0399680383488714,0.,0.999200958721789)) ;
#38019 = DIRECTION('center_axis',(0.999353662725428,0.,-0.035947973479332)) ;
#38020 = DIRECTION('ref_axis',(0.035947973479332,0.,0.999353662725428)) ;
#38021 = DIRECTION('center_axis',(0.,-8.29277425593329E-18,1.)) ;
#38022 = DIRECTION('ref_axis',(-0.990786741964199,-0.135431281275663,0.)) ;
#38023 = DIRECTION('center_axis',(-0.999353662725428,0.,0.035947973479332)) ;
#38024 = DIRECTION('ref_axis',(0.035947973479332,0.,0.999353662725428)) ;
#38025 = DIRECTION('center_axis',(-0.999353662725428,0.,0.035947973479332)) ;
#38026 = DIRECTION('ref_axis',(0.035947973479332,0.,0.999353662725428)) ;
#38027 = DIRECTION('center_axis',(0.,-0.967074537262646,-0.254493299279644)) ;
#38028 = DIRECTION('ref_axis',(1.,0.,0.)) ;
#38029 = DIRECTION('center_axis',(0.,-0.967074537262646,-0.254493299279644)) ;
#38030 = DIRECTION('ref_axis',(1.,0.,0.)) ;
#38031 = DIRECTION('center_axis',(0.,0.,1.)) ;
#38032 = DIRECTION('ref_axis',(1.,0.,0.)) ;
#38033 = DIRECTION('center_axis',(0.,0.,1.)) ;
#38034 = DIRECTION('ref_axis',(1.,0.,0.)) ;
#38035 = DIRECTION('center_axis',(-1.,0.,0.)) ;
#38036 = DIRECTION('ref_axis',(0.,0.,1.)) ;
#38037 = DIRECTION('center_axis',(0.577350269189626,0.577350269189626,0.577350269189626)) ;
#38038 = DIRECTION('ref_axis',(-0.707106781186548,0.,0.707106781186548)) ;
#38039 = DIRECTION('center_axis',(0.,0.,1.)) ;
#38040 = DIRECTION('ref_axis',(1.,0.,0.)) ;
#38041 = DIRECTION('center_axis',(0.,0.,1.)) ;
#38042 = DIRECTION('ref_axis',(1.,0.,0.)) ;
#38043 = DIRECTION('center_axis',(-1.,0.,0.)) ;
#38044 = DIRECTION('ref_axis',(0.,0.,1.)) ;
#38045 = DIRECTION('center_axis',(-1.,0.,0.)) ;
#38046 = DIRECTION('ref_axis',(0.,0.,1.)) ;
#38047 = DIRECTION('center_axis',(-1.,0.,0.)) ;
#38048 = DIRECTION('ref_axis',(0.,0.,1.)) ;
#38049 = DIRECTION('',(-1.,0.,0.)) ;
#38050 = DIRECTION('center_axis',(1.,0.,0.)) ;
#38051 = DIRECTION('ref_axis',(0.,0.,-1.)) ;
#38052 = DIRECTION('center_axis',(-1.,0.,0.)) ;
#38053 = DIRECTION('ref_axis',(0.,0.,-1.)) ;
#38054 = DIRECTION('',(1.,0.,0.)) ;
#38055 = DIRECTION('center_axis',(-1.,0.,0.)) ;
#38056 = DIRECTION('ref_axis',(0.,0.,-1.)) ;
#38057 = DIRECTION('center_axis',(1.,0.,0.)) ;
#38058 = DIRECTION('ref_axis',(0.,0.,-1.)) ;
#38059 = DIRECTION('center_axis',(1.,0.,0.)) ;
#38060 = DIRECTION('ref_axis',(0.,0.,-1.)) ;
#38061 = DIRECTION('',(-1.,0.,0.)) ;
#38062 = DIRECTION('center_axis',(-0.999800219724343,0.,0.0199880123863293)) ;
#38063 = DIRECTION('ref_axis',(-0.0199880123863293,0.,-0.999800219724343)) ;
#38064 = DIRECTION('center_axis',(-1.,0.,0.)) ;
#38065 = DIRECTION('ref_axis',(0.,0.,-1.)) ;
#38066 = DIRECTION('center_axis',(-0.999800219724343,0.,0.0199880123863293)) ;
#38067 = DIRECTION('ref_axis',(-0.0199880123863293,0.,-0.999800219724343)) ;
#38068 = DIRECTION('center_axis',(1.,0.,0.)) ;
#38069 = DIRECTION('ref_axis',(0.,0.,-1.)) ;
#38070 = DIRECTION('center_axis',(0.999200958721789,0.,-0.0399680383488714)) ;
#38071 = DIRECTION('ref_axis',(0.0399680383488714,0.,0.999200958721789)) ;
#38072 = DIRECTION('center_axis',(0.999200958721789,0.,-0.0399680383488714)) ;
#38073 = DIRECTION('ref_axis',(0.0399680383488714,0.,0.999200958721789)) ;
#38074 = DIRECTION('',(-0.999200958721789,0.,0.0399680383488714)) ;
#38075 = DIRECTION('center_axis',(-0.999279332296661,0.,0.0379580827326481)) ;
#38076 = DIRECTION('ref_axis',(0.0379580827326481,0.,0.999279332296661)) ;
#38077 = DIRECTION('center_axis',(-0.999279332296661,0.,0.0379580827326481)) ;
#38078 = DIRECTION('ref_axis',(0.0379580827326481,0.,0.999279332296661)) ;
#38079 = DIRECTION('center_axis',(0.999200958721789,0.,-0.0399680383488714)) ;
#38080 = DIRECTION('ref_axis',(0.0399680383488714,0.,0.999200958721789)) ;
#38081 = DIRECTION('center_axis',(0.999353662725428,0.,-0.035947973479332)) ;
#38082 = DIRECTION('ref_axis',(0.035947973479332,0.,0.999353662725428)) ;
#38083 = DIRECTION('',(-0.999353662725428,0.,0.035947973479332)) ;
#38084 = DIRECTION('center_axis',(-0.703439363602225,0.680718270639751,0.20443996124076)) ;
#38085 = DIRECTION('ref_axis',(0.709904500032622,0.686974583149487,0.155246651944643)) ;
#38086 = DIRECTION('center_axis',(0.,-0.967074537262646,-0.254493299279644)) ;
#38087 = DIRECTION('ref_axis',(1.,0.,0.)) ;
#38088 = DIRECTION('',(0.,0.967074537262646,0.254493299279644)) ;
#38089 = DIRECTION('center_axis',(0.,0.967074537262646,0.254493299279644)) ;
#38090 = DIRECTION('ref_axis',(1.,0.,0.)) ;
#38091 = DIRECTION('center_axis',(0.,0.610535298209836,0.791989046414044)) ;
#38092 = DIRECTION('ref_axis',(0.,-0.791989046414044,0.610535298209836)) ;
#38093 = DIRECTION('center_axis',(0.,0.,-1.)) ;
#38094 = DIRECTION('ref_axis',(1.,0.,0.)) ;
#38095 = DIRECTION('center_axis',(0.,0.,-1.)) ;
#38096 = DIRECTION('ref_axis',(1.,0.,0.)) ;
#38097 = DIRECTION('',(0.,0.,1.)) ;
#38098 = DIRECTION('center_axis',(0.707106781186554,0.,0.707106781186541)) ;
#38099 = DIRECTION('ref_axis',(0.707106781186541,0.,-0.707106781186554)) ;
#38100 = DIRECTION('center_axis',(0.707106781186554,0.,0.707106781186541)) ;
#38101 = DIRECTION('ref_axis',(0.707106781186541,0.,-0.707106781186554)) ;
#38102 = DIRECTION('center_axis',(0.,0.,-1.)) ;
#38103 = DIRECTION('ref_axis',(1.,0.,0.)) ;
#38104 = DIRECTION('center_axis',(-1.,0.,0.)) ;
#38105 = DIRECTION('ref_axis',(0.,0.,1.)) ;
#38106 = DIRECTION('',(1.,0.,0.)) ;
#38107 = DIRECTION('center_axis',(1.,0.,0.)) ;
#38108 = DIRECTION('ref_axis',(0.,0.,1.)) ;
#38109 = DIRECTION('center_axis',(1.,0.,0.)) ;
#38110 = DIRECTION('ref_axis',(0.,0.,-1.)) ;
#38111 = DIRECTION('center_axis',(0.,0.,1.)) ;
#38112 = DIRECTION('ref_axis',(1.,0.,0.)) ;
#38113 = DIRECTION('center_axis',(1.,-6.12323399573679E-17,0.)) ;
#38114 = DIRECTION('ref_axis',(0.,-1.,0.)) ;
#38115 = DIRECTION('center_axis',(0.,0.,1.)) ;
#38116 = DIRECTION('ref_axis',(1.,0.,0.)) ;
#38117 = DIRECTION('center_axis',(0.,-1.22658185435577E-18,1.)) ;
#38118 = DIRECTION('ref_axis',(-0.99979934733292,-0.0200316018497702,0.)) ;
#38119 = DIRECTION('center_axis',(0.999353662725428,0.,-0.035947973479332)) ;
#38120 = DIRECTION('ref_axis',(0.0359479734793195,0.,0.999353662725429)) ;
#38121 = DIRECTION('center_axis',(0.,0.,1.)) ;
#38122 = DIRECTION('ref_axis',(1.,0.,0.)) ;
#38123 = DIRECTION('center_axis',(-0.999353662725428,0.,0.035947973479332)) ;
#38124 = DIRECTION('ref_axis',(0.0359479734793432,0.,0.999353662725428)) ;
#38125 = DIRECTION('center_axis',(0.,-0.967074537262646,-0.254493299279644)) ;
#38126 = DIRECTION('ref_axis',(1.,0.,0.)) ;
#38127 = DIRECTION('center_axis',(-0.999353662725428,0.,0.035947973479332)) ;
#38128 = DIRECTION('ref_axis',(0.0359479734793432,0.,0.999353662725428)) ;
#38129 = DIRECTION('center_axis',(0.999353662725428,0.,-0.035947973479332)) ;
#38130 = DIRECTION('ref_axis',(0.035947973479332,0.,0.999353662725428)) ;
#38131 = DIRECTION('',(0.999353662725428,0.,-0.035947973479332)) ;
#38132 = DIRECTION('center_axis',(0.,-0.967074537262646,-0.254493299279644)) ;
#38133 = DIRECTION('ref_axis',(1.,0.,0.)) ;
#38134 = DIRECTION('center_axis',(0.,0.,1.)) ;
#38135 = DIRECTION('ref_axis',(1.,0.,0.)) ;
#38136 = DIRECTION('center_axis',(-1.22464679914737E-16,1.,0.)) ;
#38137 = DIRECTION('ref_axis',(-1.,-1.22464679914737E-16,0.)) ;
#38138 = DIRECTION('center_axis',(0.,0.,1.)) ;
#38139 = DIRECTION('ref_axis',(1.,0.,0.)) ;
#38140 = DIRECTION('center_axis',(0.,0.,-1.)) ;
#38141 = DIRECTION('ref_axis',(1.,0.,0.)) ;
#38142 = DIRECTION('center_axis',(0.,0.967074537262646,0.254493299279644)) ;
#38143 = DIRECTION('ref_axis',(1.,-2.36847578586702E-14,-4.73695157173405E-14)) ;
#38144 = DIRECTION('center_axis',(0.,0.967074537262646,0.254493299279644)) ;
#38145 = DIRECTION('ref_axis',(1.,-2.36847578586702E-14,-4.73695157173405E-14)) ;
#38146 = DIRECTION('center_axis',(0.,0.,-1.)) ;
#38147 = DIRECTION('ref_axis',(1.,0.,0.)) ;
#38148 = DIRECTION('center_axis',(0.999353662725428,0.,-0.035947973479332)) ;
#38149 = DIRECTION('ref_axis',(0.035947973479332,0.,0.999353662725428)) ;
#38150 = DIRECTION('center_axis',(-0.999353662725428,0.,0.035947973479332)) ;
#38151 = DIRECTION('ref_axis',(0.035947973479332,0.,0.999353662725428)) ;
#38152 = DIRECTION('center_axis',(0.,-0.967074537262646,-0.254493299279644)) ;
#38153 = DIRECTION('ref_axis',(1.,0.,0.)) ;
#38154 = DIRECTION('',(0.,-0.967074537262646,-0.254493299279644)) ;
#38155 = DIRECTION('center_axis',(0.,-0.967074537262646,-0.254493299279644)) ;
#38156 = DIRECTION('ref_axis',(1.,1.48029736616689E-14,4.73695157173405E-14)) ;
#38157 = DIRECTION('center_axis',(0.,-0.967074537262646,-0.254493299279644)) ;
#38158 = DIRECTION('ref_axis',(1.,1.48029736616689E-14,4.73695157173405E-14)) ;
#38159 = DIRECTION('center_axis',(0.,0.,1.)) ;
#38160 = DIRECTION('ref_axis',(1.,0.,0.)) ;
#38161 = DIRECTION('center_axis',(0.,0.,1.)) ;
#38162 = DIRECTION('ref_axis',(1.,0.,0.)) ;
#38163 = DIRECTION('center_axis',(0.,0.,-1.)) ;
#38164 = DIRECTION('ref_axis',(1.,0.,0.)) ;
#38165 = DIRECTION('center_axis',(0.,0.967074537262646,0.254493299279644)) ;
#38166 = DIRECTION('ref_axis',(1.,0.,0.)) ;
#38167 = DIRECTION('center_axis',(0.,0.,-1.)) ;
#38168 = DIRECTION('ref_axis',(1.,0.,0.)) ;
#38169 = DIRECTION('center_axis',(0.,-1.,0.)) ;
#38170 = DIRECTION('ref_axis',(-1.,0.,0.)) ;
#38171 = DIRECTION('center_axis',(-1.,0.,0.)) ;
#38172 = DIRECTION('ref_axis',(0.,-3.43024899888577E-15,-1.)) ;
#38173 = DIRECTION('center_axis',(-1.,0.,0.)) ;
#38174 = DIRECTION('ref_axis',(0.,0.,1.)) ;
#38175 = DIRECTION('center_axis',(0.,0.,-1.)) ;
#38176 = DIRECTION('ref_axis',(1.,0.,0.)) ;
#38177 = DIRECTION('center_axis',(0.,0.,1.)) ;
#38178 = DIRECTION('ref_axis',(1.,0.,0.)) ;
#38179 = DIRECTION('',(0.,0.,-1.)) ;
#38180 = DIRECTION('center_axis',(0.,0.,1.)) ;
#38181 = DIRECTION('ref_axis',(1.,0.,0.)) ;
#38182 = DIRECTION('center_axis',(0.,-0.967074537262646,-0.254493299279644)) ;
#38183 = DIRECTION('ref_axis',(1.,0.,0.)) ;
#38184 = DIRECTION('center_axis',(1.,0.,0.)) ;
#38185 = DIRECTION('ref_axis',(0.,-1.,0.)) ;
#38186 = DIRECTION('center_axis',(0.,0.,1.)) ;
#38187 = DIRECTION('ref_axis',(1.,0.,0.)) ;
#38188 = DIRECTION('center_axis',(0.,1.,0.)) ;
#38189 = DIRECTION('ref_axis',(-1.,0.,0.)) ;
#38190 = DIRECTION('axis',(0.,0.,1.)) ;
#38191 = DIRECTION('refdir',(1.,0.,0.)) ;
#38192 = DIRECTION('center_axis',(0.,0.,1.)) ;
#38193 = DIRECTION('ref_axis',(1.,0.,0.)) ;
#38194 = DIRECTION('center_axis',(-0.707106781186548,0.,-0.707106781186548)) ;
#38195 = DIRECTION('ref_axis',(0.707106781186547,0.,-0.707106781186547)) ;
#38196 = DIRECTION('center_axis',(-0.707106781186548,0.,0.707106781186548)) ;
#38197 = DIRECTION('ref_axis',(0.707106781186547,0.,0.707106781186547)) ;
#38198 = DIRECTION('',(0.,0.,-1.)) ;
#38199 = DIRECTION('center_axis',(0.,0.,-1.)) ;
#38200 = DIRECTION('ref_axis',(1.,0.,0.)) ;
#38201 = DIRECTION('center_axis',(-0.707106781186548,0.,0.707106781186548)) ;
#38202 = DIRECTION('ref_axis',(0.707106781186547,0.,0.707106781186547)) ;
#38203 = DIRECTION('center_axis',(-0.707106781186548,0.,-0.707106781186548)) ;
#38204 = DIRECTION('ref_axis',(0.707106781186547,0.,-0.707106781186547)) ;
#38205 = DIRECTION('center_axis',(0.,0.,1.)) ;
#38206 = DIRECTION('ref_axis',(1.,0.,0.)) ;
#38207 = DIRECTION('center_axis',(0.,0.,-1.)) ;
#38208 = DIRECTION('ref_axis',(-1.,0.,0.)) ;
#38209 = DIRECTION('center_axis',(0.,0.,1.)) ;
#38210 = DIRECTION('ref_axis',(1.,0.,0.)) ;
#38211 = DIRECTION('',(1.,0.,0.)) ;
#38212 = DIRECTION('',(-1.,0.,0.)) ;
#38213 = DIRECTION('',(0.,1.,0.)) ;
#38214 = DIRECTION('center_axis',(1.,0.,0.)) ;
#38215 = DIRECTION('ref_axis',(0.,0.,-1.)) ;
#38216 = DIRECTION('center_axis',(1.,0.,0.)) ;
#38217 = DIRECTION('ref_axis',(0.,0.,-1.)) ;
#38218 = DIRECTION('center_axis',(1.,0.,0.)) ;
#38219 = DIRECTION('ref_axis',(0.,0.,-1.)) ;
#38220 = DIRECTION('center_axis',(1.,0.,0.)) ;
#38221 = DIRECTION('ref_axis',(0.,0.,-1.)) ;
#38222 = DIRECTION('',(-1.,0.,0.)) ;
#38223 = DIRECTION('center_axis',(-1.,0.,0.)) ;
#38224 = DIRECTION('ref_axis',(0.,0.,-1.)) ;
#38225 = DIRECTION('center_axis',(-1.,0.,0.)) ;
#38226 = DIRECTION('ref_axis',(0.,0.,1.)) ;
#38227 = DIRECTION('center_axis',(0.,0.,1.)) ;
#38228 = DIRECTION('ref_axis',(1.,0.,0.)) ;
#38229 = DIRECTION('center_axis',(0.,0.,1.)) ;
#38230 = DIRECTION('ref_axis',(1.,0.,0.)) ;
#38231 = DIRECTION('',(0.,0.,-1.)) ;
#38232 = DIRECTION('center_axis',(0.,0.,-1.)) ;
#38233 = DIRECTION('ref_axis',(1.,0.,0.)) ;
#38234 = DIRECTION('center_axis',(0.,0.,-1.)) ;
#38235 = DIRECTION('ref_axis',(-1.,0.,0.)) ;
#38236 = DIRECTION('center_axis',(0.,0.,1.)) ;
#38237 = DIRECTION('ref_axis',(1.,0.,0.)) ;
#38238 = DIRECTION('axis',(0.,0.,1.)) ;
#38239 = DIRECTION('refdir',(1.,0.,0.)) ;
#38240 = DIRECTION('center_axis',(0.,0.,1.)) ;
#38241 = DIRECTION('ref_axis',(1.,0.,0.)) ;
#38242 = DIRECTION('center_axis',(0.,0.,1.)) ;
#38243 = DIRECTION('ref_axis',(1.,0.,0.)) ;
#38244 = DIRECTION('',(0.,0.,-1.)) ;
#38245 = DIRECTION('center_axis',(0.,0.,-1.)) ;
#38246 = DIRECTION('ref_axis',(1.,0.,0.)) ;
#38247 = DIRECTION('center_axis',(0.,0.,-1.)) ;
#38248 = DIRECTION('ref_axis',(-1.,0.,0.)) ;
#38249 = DIRECTION('center_axis',(0.,0.,1.)) ;
#38250 = DIRECTION('ref_axis',(1.,0.,0.)) ;
#38251 = DIRECTION('axis',(0.,0.,1.)) ;
#38252 = DIRECTION('refdir',(1.,0.,0.)) ;
#38253 = DIRECTION('center_axis',(0.,0.,1.)) ;
#38254 = DIRECTION('ref_axis',(1.,0.,0.)) ;
#38255 = DIRECTION('center_axis',(0.,0.,1.)) ;
#38256 = DIRECTION('ref_axis',(1.,0.,0.)) ;
#38257 = DIRECTION('',(0.,0.,-1.)) ;
#38258 = DIRECTION('center_axis',(0.,0.,-1.)) ;
#38259 = DIRECTION('ref_axis',(1.,0.,0.)) ;
#38260 = DIRECTION('center_axis',(0.,0.,-1.)) ;
#38261 = DIRECTION('ref_axis',(-1.,0.,0.)) ;
#38262 = DIRECTION('center_axis',(0.,0.,1.)) ;
#38263 = DIRECTION('ref_axis',(1.,0.,0.)) ;
#38264 = DIRECTION('axis',(0.,0.,1.)) ;
#38265 = DIRECTION('refdir',(1.,0.,0.)) ;
#38266 = DIRECTION('center_axis',(0.,0.,1.)) ;
#38267 = DIRECTION('ref_axis',(1.,0.,0.)) ;
#38268 = DIRECTION('center_axis',(0.,0.,1.)) ;
#38269 = DIRECTION('ref_axis',(1.,0.,0.)) ;
#38270 = DIRECTION('',(0.,0.,-1.)) ;
#38271 = DIRECTION('center_axis',(0.,0.,-1.)) ;
#38272 = DIRECTION('ref_axis',(1.,0.,0.)) ;
#38273 = DIRECTION('center_axis',(0.,0.,1.)) ;
#38274 = DIRECTION('ref_axis',(1.,0.,0.)) ;
#38275 = DIRECTION('center_axis',(0.,0.,1.)) ;
#38276 = DIRECTION('ref_axis',(1.,0.,0.)) ;
#38277 = DIRECTION('',(0.,0.,1.)) ;
#38278 = DIRECTION('center_axis',(0.,0.,-1.)) ;
#38279 = DIRECTION('ref_axis',(1.,0.,0.)) ;
#38280 = DIRECTION('center_axis',(0.,0.,-1.)) ;
#38281 = DIRECTION('ref_axis',(-1.,0.,0.)) ;
#38282 = DIRECTION('center_axis',(0.,0.,1.)) ;
#38283 = DIRECTION('ref_axis',(1.,0.,0.)) ;
#38284 = DIRECTION('center_axis',(0.94299033358289,0.,0.332820117735135)) ;
#38285 = DIRECTION('ref_axis',(0.332820117735135,0.,-0.94299033358289)) ;
#38286 = DIRECTION('center_axis',(0.94299033358289,0.,0.332820117735135)) ;
#38287 = DIRECTION('ref_axis',(0.332820117735135,0.,-0.94299033358289)) ;
#38288 = DIRECTION('',(-0.94299033358289,0.,-0.332820117735135)) ;
#38289 = DIRECTION('center_axis',(0.94299033358289,0.,0.332820117735135)) ;
#38290 = DIRECTION('ref_axis',(0.332820117735135,0.,-0.94299033358289)) ;
#38291 = DIRECTION('center_axis',(1.,0.,0.)) ;
#38292 = DIRECTION('ref_axis',(0.,0.,-1.)) ;
#38293 = DIRECTION('center_axis',(1.,0.,0.)) ;
#38294 = DIRECTION('ref_axis',(0.,0.,-1.)) ;
#38295 = DIRECTION('',(1.,0.,0.)) ;
#38296 = DIRECTION('center_axis',(-1.,0.,0.)) ;
#38297 = DIRECTION('ref_axis',(0.,0.,-1.)) ;
#38298 = DIRECTION('center_axis',(1.,0.,0.)) ;
#38299 = DIRECTION('ref_axis',(0.,0.,-1.)) ;
#38300 = DIRECTION('center_axis',(1.,0.,0.)) ;
#38301 = DIRECTION('ref_axis',(0.,0.,-1.)) ;
#38302 = DIRECTION('',(-1.,0.,0.)) ;
#38303 = DIRECTION('center_axis',(-1.,0.,0.)) ;
#38304 = DIRECTION('ref_axis',(0.,0.,-1.)) ;
#38305 = DIRECTION('center_axis',(-1.,0.,0.)) ;
#38306 = DIRECTION('ref_axis',(0.,0.,1.)) ;
#38307 = DIRECTION('center_axis',(1.,0.,0.)) ;
#38308 = DIRECTION('ref_axis',(0.,0.,-1.)) ;
#38309 = DIRECTION('center_axis',(1.,0.,0.)) ;
#38310 = DIRECTION('ref_axis',(0.,0.,-1.)) ;
#38311 = DIRECTION('center_axis',(0.091482478332531,-0.920005415661246,0.381078720623595)) ;
#38312 = DIRECTION('ref_axis',(0.995806686138499,0.0845187893148324,-0.0350088288095587)) ;
#38313 = DIRECTION('center_axis',(1.,0.,0.)) ;
#38314 = DIRECTION('ref_axis',(0.,0.,-1.)) ;
#38315 = DIRECTION('',(1.,0.,0.)) ;
#38316 = DIRECTION('center_axis',(-1.,0.,0.)) ;
#38317 = DIRECTION('ref_axis',(0.,0.,-1.)) ;
#38318 = DIRECTION('center_axis',(1.,0.,0.)) ;
#38319 = DIRECTION('ref_axis',(0.,0.,-1.)) ;
#38320 = DIRECTION('center_axis',(1.,0.,0.)) ;
#38321 = DIRECTION('ref_axis',(0.,0.,-1.)) ;
#38322 = DIRECTION('',(-1.,0.,0.)) ;
#38323 = DIRECTION('center_axis',(-1.,0.,0.)) ;
#38324 = DIRECTION('ref_axis',(0.,0.,-1.)) ;
#38325 = DIRECTION('center_axis',(-1.,0.,0.)) ;
#38326 = DIRECTION('ref_axis',(0.,0.,1.)) ;
#38327 = DIRECTION('',(0.,0.382683432365099,0.923879532511283)) ;
#38328 = DIRECTION('center_axis',(-1.,0.,0.)) ;
#38329 = DIRECTION('ref_axis',(0.,-0.382683432365094,-0.923879532511285)) ;
#38330 = DIRECTION('center_axis',(-1.,0.,0.)) ;
#38331 = DIRECTION('ref_axis',(0.,0.,-1.)) ;
#38332 = DIRECTION('center_axis',(-1.,0.,0.)) ;
#38333 = DIRECTION('ref_axis',(0.,0.38268343236509,-0.923879532511287)) ;
#38334 = DIRECTION('center_axis',(-1.,0.,0.)) ;
#38335 = DIRECTION('ref_axis',(0.,0.,-1.)) ;
#38336 = DIRECTION('center_axis',(-1.,0.,0.)) ;
#38337 = DIRECTION('ref_axis',(0.,0.923879532511283,-0.382683432365099)) ;
#38338 = DIRECTION('center_axis',(1.,0.,0.)) ;
#38339 = DIRECTION('ref_axis',(0.,0.,-1.)) ;
#38340 = DIRECTION('center_axis',(0.091482478332531,-0.920005415661246,0.381078720623595)) ;
#38341 = DIRECTION('ref_axis',(0.995806686138499,0.0845187893148324,-0.0350088288095587)) ;
#38342 = DIRECTION('center_axis',(0.091482478332531,-0.920005415661246,0.381078720623595)) ;
#38343 = DIRECTION('ref_axis',(0.995806686138498,0.0845187893148324,-0.0350088288095587)) ;
#38344 = DIRECTION('center_axis',(0.,0.,1.)) ;
#38345 = DIRECTION('ref_axis',(-0.421632036455268,0.906767018497356,0.)) ;
#38346 = DIRECTION('center_axis',(0.0914824783325255,-0.381078720623586,0.92000541566125)) ;
#38347 = DIRECTION('ref_axis',(0.995806686138499,0.0350088288095558,-0.0845187893148275)) ;
#38348 = DIRECTION('center_axis',(-0.091482478332531,0.920005415661246,-0.381078720623595)) ;
#38349 = DIRECTION('ref_axis',(0.995806686138498,0.0845187893148324,-0.0350088288095587)) ;
#38350 = DIRECTION('center_axis',(0.,0.,1.)) ;
#38351 = DIRECTION('ref_axis',(1.,0.,0.)) ;
#38352 = DIRECTION('center_axis',(0.0914824783325241,0.381078720623591,0.920005415661248)) ;
#38353 = DIRECTION('ref_axis',(0.995806686138499,-0.0350088288095557,-0.0845187893148261)) ;
#38354 = DIRECTION('center_axis',(0.0914824783325241,0.381078720623591,0.920005415661248)) ;
#38355 = DIRECTION('ref_axis',(0.995806686138499,-0.0350088288095557,-0.0845187893148261)) ;
#38356 = DIRECTION('center_axis',(-0.0914824783325255,0.381078720623586,-0.92000541566125)) ;
#38357 = DIRECTION('ref_axis',(0.995806686138499,0.0350088288095558,-0.0845187893148275)) ;
#38358 = DIRECTION('center_axis',(0.,0.,1.)) ;
#38359 = DIRECTION('ref_axis',(1.,0.,0.)) ;
#38360 = DIRECTION('center_axis',(-0.0914824783325241,-0.381078720623591,
-0.920005415661248)) ;
#38361 = DIRECTION('ref_axis',(0.995806686138499,-0.0350088288095557,-0.0845187893148261)) ;
#38362 = DIRECTION('center_axis',(0.0914824783325315,0.920005415661255,0.381078720623574)) ;
#38363 = DIRECTION('ref_axis',(0.995806686138498,-0.0845187893148336,-0.035008828809557)) ;
#38364 = DIRECTION('center_axis',(0.0914824783325315,0.920005415661255,0.381078720623574)) ;
#38365 = DIRECTION('ref_axis',(0.995806686138498,-0.0845187893148336,-0.035008828809557)) ;
#38366 = DIRECTION('center_axis',(0.,0.,1.)) ;
#38367 = DIRECTION('ref_axis',(1.,0.,0.)) ;
#38368 = DIRECTION('center_axis',(-0.0914824783325315,-0.920005415661255,
-0.381078720623574)) ;
#38369 = DIRECTION('ref_axis',(0.995806686138498,-0.0845187893148336,-0.035008828809557)) ;
#38370 = DIRECTION('center_axis',(0.0914824783325258,0.92000541566125,-0.381078720623586)) ;
#38371 = DIRECTION('ref_axis',(0.995806686138499,-0.0845187893148279,0.0350088288095559)) ;
#38372 = DIRECTION('center_axis',(1.22464679914737E-16,-1.,0.)) ;
#38373 = DIRECTION('ref_axis',(-1.,-1.22464679914737E-16,0.)) ;
#38374 = DIRECTION('center_axis',(0.0914824783325258,0.92000541566125,-0.381078720623586)) ;
#38375 = DIRECTION('ref_axis',(0.995806686138499,-0.0845187893148279,0.0350088288095559)) ;
#38376 = DIRECTION('center_axis',(0.0914824783325258,0.92000541566125,-0.381078720623586)) ;
#38377 = DIRECTION('ref_axis',(0.995806686138499,-0.0845187893148279,0.0350088288095559)) ;
#38378 = DIRECTION('center_axis',(0.,0.,1.)) ;
#38379 = DIRECTION('ref_axis',(-0.0701393346692214,-0.997537204184465,0.)) ;
#38380 = DIRECTION('center_axis',(-0.0914824783325258,-0.92000541566125,0.381078720623586)) ;
#38381 = DIRECTION('ref_axis',(0.995806686138499,-0.0845187893148279,0.0350088288095559)) ;
#38382 = DIRECTION('center_axis',(0.0914824783325313,0.381078720623583,-0.920005415661251)) ;
#38383 = DIRECTION('ref_axis',(0.995806686138498,-0.0350088288095578,0.084518789314833)) ;
#38384 = DIRECTION('center_axis',(0.0914824783325313,0.381078720623583,-0.920005415661251)) ;
#38385 = DIRECTION('ref_axis',(0.995806686138498,-0.0350088288095578,0.084518789314833)) ;
#38386 = DIRECTION('center_axis',(0.,0.,1.)) ;
#38387 = DIRECTION('ref_axis',(1.,0.,0.)) ;
#38388 = DIRECTION('center_axis',(-0.0914824783325313,-0.381078720623583,
0.920005415661251)) ;
#38389 = DIRECTION('ref_axis',(0.995806686138498,-0.0350088288095578,0.084518789314833)) ;
#38390 = DIRECTION('center_axis',(0.0914824783325254,-0.381078720623587,-0.92000541566125)) ;
#38391 = DIRECTION('ref_axis',(0.995806686138499,0.0350088288095558,0.0845187893148275)) ;
#38392 = DIRECTION('center_axis',(0.0914824783325254,-0.381078720623587,-0.92000541566125)) ;
#38393 = DIRECTION('ref_axis',(0.995806686138499,0.0350088288095558,0.0845187893148275)) ;
#38394 = DIRECTION('center_axis',(0.,0.,1.)) ;
#38395 = DIRECTION('ref_axis',(1.,0.,0.)) ;
#38396 = DIRECTION('center_axis',(-0.0914824783325254,0.381078720623587,0.92000541566125)) ;
#38397 = DIRECTION('ref_axis',(0.995806686138499,0.0350088288095558,0.0845187893148275)) ;
#38398 = DIRECTION('center_axis',(0.0914824783325237,-0.920005415661249,-0.381078720623589)) ;
#38399 = DIRECTION('ref_axis',(0.995806686138499,0.0845187893148259,0.0350088288095553)) ;
#38400 = DIRECTION('center_axis',(0.0914824783325237,-0.920005415661249,-0.381078720623589)) ;
#38401 = DIRECTION('ref_axis',(0.995806686138499,0.0845187893148259,0.0350088288095553)) ;
#38402 = DIRECTION('center_axis',(0.,0.,1.)) ;
#38403 = DIRECTION('ref_axis',(1.,0.,0.)) ;
#38404 = DIRECTION('center_axis',(-0.0914824783325237,0.920005415661249,0.381078720623589)) ;
#38405 = DIRECTION('ref_axis',(0.995806686138499,0.0845187893148259,0.0350088288095553)) ;
#38406 = DIRECTION('center_axis',(0.0914824783325308,-0.920005415661242,0.381078720623606)) ;
#38407 = DIRECTION('ref_axis',(0.995806686138498,0.0845187893148318,-0.0350088288095597)) ;
#38408 = DIRECTION('center_axis',(1.22464679914732E-16,-1.,0.)) ;
#38409 = DIRECTION('ref_axis',(-1.,-1.22464679914732E-16,0.)) ;
#38410 = DIRECTION('center_axis',(0.0914824783325308,-0.920005415661242,0.381078720623606)) ;
#38411 = DIRECTION('ref_axis',(0.995806686138498,0.0845187893148318,-0.0350088288095597)) ;
#38412 = DIRECTION('center_axis',(0.0914824783325308,-0.920005415661242,0.381078720623606)) ;
#38413 = DIRECTION('ref_axis',(0.995806686138498,0.0845187893148318,-0.0350088288095597)) ;
#38414 = DIRECTION('center_axis',(0.,0.,1.)) ;
#38415 = DIRECTION('ref_axis',(-0.0701393346692214,0.997537204184465,0.)) ;
#38416 = DIRECTION('center_axis',(-0.0914824783325308,0.920005415661242,-0.381078720623606)) ;
#38417 = DIRECTION('ref_axis',(0.995806686138498,0.0845187893148318,-0.0350088288095597)) ;
#38418 = DIRECTION('center_axis',(0.0914824783325257,-0.381078720623581,0.920005415661252)) ;
#38419 = DIRECTION('ref_axis',(0.995806686138499,0.0350088288095554,-0.0845187893148279)) ;
#38420 = DIRECTION('center_axis',(0.0914824783325257,-0.381078720623581,0.920005415661252)) ;
#38421 = DIRECTION('ref_axis',(0.995806686138499,0.0350088288095554,-0.0845187893148279)) ;
#38422 = DIRECTION('center_axis',(0.,0.,1.)) ;
#38423 = DIRECTION('ref_axis',(1.,0.,0.)) ;
#38424 = DIRECTION('center_axis',(-0.0914824783325257,0.381078720623581,-0.920005415661252)) ;
#38425 = DIRECTION('ref_axis',(0.995806686138499,0.0350088288095554,-0.0845187893148279)) ;
#38426 = DIRECTION('center_axis',(0.091482478332532,0.381078720623593,0.920005415661247)) ;
#38427 = DIRECTION('ref_axis',(0.995806686138498,-0.0350088288095589,-0.0845187893148333)) ;
#38428 = DIRECTION('center_axis',(0.091482478332532,0.381078720623593,0.920005415661247)) ;
#38429 = DIRECTION('ref_axis',(0.995806686138498,-0.0350088288095589,-0.0845187893148333)) ;
#38430 = DIRECTION('center_axis',(0.,0.,1.)) ;
#38431 = DIRECTION('ref_axis',(1.,0.,0.)) ;
#38432 = DIRECTION('center_axis',(-0.091482478332532,-0.381078720623593,-0.920005415661247)) ;
#38433 = DIRECTION('ref_axis',(0.995806686138498,-0.0350088288095589,-0.0845187893148333)) ;
#38434 = DIRECTION('center_axis',(0.0914824783325256,0.920005415661251,0.381078720623585)) ;
#38435 = DIRECTION('ref_axis',(0.995806686138499,-0.0845187893148277,-0.0350088288095557)) ;
#38436 = DIRECTION('center_axis',(0.0914824783325256,0.920005415661251,0.381078720623585)) ;
#38437 = DIRECTION('ref_axis',(0.995806686138499,-0.0845187893148277,-0.0350088288095557)) ;
#38438 = DIRECTION('center_axis',(0.,0.,1.)) ;
#38439 = DIRECTION('ref_axis',(1.,0.,0.)) ;
#38440 = DIRECTION('center_axis',(-0.0914824783325256,-0.920005415661251,
-0.381078720623585)) ;
#38441 = DIRECTION('ref_axis',(0.995806686138499,-0.0845187893148277,-0.0350088288095557)) ;
#38442 = DIRECTION('center_axis',(0.0914824783325256,0.920005415661251,-0.381078720623585)) ;
#38443 = DIRECTION('ref_axis',(0.995806686138499,-0.0845187893148277,0.0350088288095557)) ;
#38444 = DIRECTION('center_axis',(1.22464679914737E-16,-1.,0.)) ;
#38445 = DIRECTION('ref_axis',(-1.,-1.22464679914737E-16,0.)) ;
#38446 = DIRECTION('center_axis',(0.0914824783325256,0.920005415661251,-0.381078720623585)) ;
#38447 = DIRECTION('ref_axis',(0.995806686138499,-0.0845187893148277,0.0350088288095557)) ;
#38448 = DIRECTION('center_axis',(0.0914824783325256,0.920005415661251,-0.381078720623585)) ;
#38449 = DIRECTION('ref_axis',(0.995806686138499,-0.0845187893148277,0.0350088288095557)) ;
#38450 = DIRECTION('center_axis',(0.,0.,1.)) ;
#38451 = DIRECTION('ref_axis',(-0.0701393346692214,-0.997537204184465,0.)) ;
#38452 = DIRECTION('center_axis',(-0.0914824783325256,-0.920005415661251,
0.381078720623585)) ;
#38453 = DIRECTION('ref_axis',(0.995806686138499,-0.0845187893148277,0.0350088288095557)) ;
#38454 = DIRECTION('center_axis',(0.0914824783325301,0.381078720623585,-0.92000541566125)) ;
#38455 = DIRECTION('ref_axis',(0.995806686138499,-0.0350088288095575,0.0845187893148319)) ;
#38456 = DIRECTION('center_axis',(0.0914824783325301,0.381078720623585,-0.92000541566125)) ;
#38457 = DIRECTION('ref_axis',(0.995806686138499,-0.0350088288095575,0.0845187893148319)) ;
#38458 = DIRECTION('center_axis',(0.,0.,1.)) ;
#38459 = DIRECTION('ref_axis',(1.,0.,0.)) ;
#38460 = DIRECTION('center_axis',(-0.0914824783325301,-0.381078720623585,
0.92000541566125)) ;
#38461 = DIRECTION('ref_axis',(0.995806686138499,-0.0350088288095575,0.0845187893148319)) ;
#38462 = DIRECTION('center_axis',(0.0914824783325252,-0.381078720623592,-0.920005415661248)) ;
#38463 = DIRECTION('ref_axis',(0.995806686138499,0.0350088288095562,0.0845187893148271)) ;
#38464 = DIRECTION('center_axis',(0.0914824783325252,-0.381078720623592,-0.920005415661248)) ;
#38465 = DIRECTION('ref_axis',(0.995806686138499,0.0350088288095562,0.0845187893148271)) ;
#38466 = DIRECTION('center_axis',(0.,0.,1.)) ;
#38467 = DIRECTION('ref_axis',(1.,0.,0.)) ;
#38468 = DIRECTION('center_axis',(-0.0914824783325252,0.381078720623592,0.920005415661248)) ;
#38469 = DIRECTION('ref_axis',(0.995806686138499,0.0350088288095562,0.0845187893148271)) ;
#38470 = DIRECTION('center_axis',(0.0914824783325312,-0.920005415661251,-0.381078720623584)) ;
#38471 = DIRECTION('ref_axis',(0.995806686138498,0.0845187893148329,0.0350088288095578)) ;
#38472 = DIRECTION('center_axis',(0.0914824783325312,-0.920005415661251,-0.381078720623584)) ;
#38473 = DIRECTION('ref_axis',(0.995806686138498,0.0845187893148329,0.0350088288095578)) ;
#38474 = DIRECTION('center_axis',(0.,0.,1.)) ;
#38475 = DIRECTION('ref_axis',(1.,0.,0.)) ;
#38476 = DIRECTION('center_axis',(-0.0914824783325312,0.920005415661251,0.381078720623584)) ;
#38477 = DIRECTION('ref_axis',(0.995806686138498,0.0845187893148329,0.0350088288095578)) ;
#38478 = DIRECTION('center_axis',(0.0914824783325253,-0.920005415661246,0.381078720623595)) ;
#38479 = DIRECTION('ref_axis',(0.995806686138499,0.0845187893148271,-0.0350088288095565)) ;
#38480 = DIRECTION('center_axis',(1.22464679914737E-16,-1.,0.)) ;
#38481 = DIRECTION('ref_axis',(-1.,-1.22464679914737E-16,0.)) ;
#38482 = DIRECTION('center_axis',(0.0914824783325253,-0.920005415661246,0.381078720623595)) ;
#38483 = DIRECTION('ref_axis',(0.995806686138499,0.0845187893148271,-0.0350088288095565)) ;
#38484 = DIRECTION('center_axis',(0.0914824783325253,-0.920005415661246,0.381078720623595)) ;
#38485 = DIRECTION('ref_axis',(0.995806686138499,0.0845187893148271,-0.0350088288095565)) ;
#38486 = DIRECTION('center_axis',(0.,0.,1.)) ;
#38487 = DIRECTION('ref_axis',(-0.0701393346692214,0.997537204184465,0.)) ;
#38488 = DIRECTION('center_axis',(-0.0914824783325253,0.920005415661246,-0.381078720623595)) ;
#38489 = DIRECTION('ref_axis',(0.995806686138499,0.0845187893148271,-0.0350088288095565)) ;
#38490 = DIRECTION('center_axis',(0.0914824783325254,-0.381078720623587,0.92000541566125)) ;
#38491 = DIRECTION('ref_axis',(0.995806686138499,0.0350088288095558,-0.0845187893148275)) ;
#38492 = DIRECTION('center_axis',(0.0914824783325254,-0.381078720623587,0.92000541566125)) ;
#38493 = DIRECTION('ref_axis',(0.995806686138499,0.0350088288095558,-0.0845187893148275)) ;
#38494 = DIRECTION('center_axis',(0.,0.,1.)) ;
#38495 = DIRECTION('ref_axis',(1.,0.,0.)) ;
#38496 = DIRECTION('center_axis',(-0.0914824783325254,0.381078720623587,-0.92000541566125)) ;
#38497 = DIRECTION('ref_axis',(0.995806686138499,0.0350088288095558,-0.0845187893148275)) ;
#38498 = DIRECTION('center_axis',(0.0914824783325299,0.38107872062359,0.920005415661248)) ;
#38499 = DIRECTION('ref_axis',(0.995806686138498,-0.0350088288095579,-0.0845187893148314)) ;
#38500 = DIRECTION('center_axis',(0.0914824783325299,0.38107872062359,0.920005415661248)) ;
#38501 = DIRECTION('ref_axis',(0.995806686138498,-0.0350088288095579,-0.0845187893148314)) ;
#38502 = DIRECTION('center_axis',(0.,0.,1.)) ;
#38503 = DIRECTION('ref_axis',(1.,0.,0.)) ;
#38504 = DIRECTION('center_axis',(-0.0914824783325299,-0.38107872062359,-0.920005415661248)) ;
#38505 = DIRECTION('ref_axis',(0.995806686138498,-0.0350088288095579,-0.0845187893148314)) ;
#38506 = DIRECTION('center_axis',(0.0914824783325257,0.920005415661255,0.381078720623574)) ;
#38507 = DIRECTION('ref_axis',(0.995806686138499,-0.0845187893148283,-0.0350088288095548)) ;
#38508 = DIRECTION('center_axis',(0.0914824783325257,0.920005415661255,0.381078720623574)) ;
#38509 = DIRECTION('ref_axis',(0.995806686138499,-0.0845187893148283,-0.0350088288095548)) ;
#38510 = DIRECTION('center_axis',(0.,0.,1.)) ;
#38511 = DIRECTION('ref_axis',(1.,0.,0.)) ;
#38512 = DIRECTION('center_axis',(-0.0914824783325257,-0.920005415661255,
-0.381078720623574)) ;
#38513 = DIRECTION('ref_axis',(0.995806686138499,-0.0845187893148283,-0.0350088288095548)) ;
#38514 = DIRECTION('center_axis',(0.0914824783325315,0.92000541566125,-0.381078720623586)) ;
#38515 = DIRECTION('ref_axis',(0.995806686138498,-0.0845187893148332,0.0350088288095581)) ;
#38516 = DIRECTION('center_axis',(1.22464679914737E-16,-1.,0.)) ;
#38517 = DIRECTION('ref_axis',(-1.,-1.22464679914737E-16,0.)) ;
#38518 = DIRECTION('center_axis',(0.0914824783325315,0.92000541566125,-0.381078720623586)) ;
#38519 = DIRECTION('ref_axis',(0.995806686138498,-0.0845187893148332,0.0350088288095581)) ;
#38520 = DIRECTION('center_axis',(0.0914824783325315,0.92000541566125,-0.381078720623586)) ;
#38521 = DIRECTION('ref_axis',(0.995806686138498,-0.0845187893148332,0.0350088288095581)) ;
#38522 = DIRECTION('center_axis',(0.,0.,1.)) ;
#38523 = DIRECTION('ref_axis',(-0.0701393346692214,-0.997537204184465,0.)) ;
#38524 = DIRECTION('center_axis',(-0.0914824783325315,-0.92000541566125,0.381078720623586)) ;
#38525 = DIRECTION('ref_axis',(0.995806686138498,-0.0845187893148332,0.0350088288095581)) ;
#38526 = DIRECTION('center_axis',(0.0914824783325256,0.381078720623584,-0.920005415661251)) ;
#38527 = DIRECTION('ref_axis',(0.995806686138499,-0.0350088288095556,0.0845187893148277)) ;
#38528 = DIRECTION('center_axis',(0.0914824783325256,0.381078720623584,-0.920005415661251)) ;
#38529 = DIRECTION('ref_axis',(0.995806686138499,-0.0350088288095556,0.0845187893148277)) ;
#38530 = DIRECTION('center_axis',(0.,0.,1.)) ;
#38531 = DIRECTION('ref_axis',(1.,0.,0.)) ;
#38532 = DIRECTION('center_axis',(-0.0914824783325256,-0.381078720623584,
0.920005415661251)) ;
#38533 = DIRECTION('ref_axis',(0.995806686138499,-0.0350088288095556,0.0845187893148277)) ;
#38534 = DIRECTION('center_axis',(0.0914824783325255,-0.381078720623586,-0.92000541566125)) ;
#38535 = DIRECTION('ref_axis',(0.995806686138499,0.0350088288095558,0.0845187893148275)) ;
#38536 = DIRECTION('center_axis',(0.0914824783325255,-0.381078720623586,-0.92000541566125)) ;
#38537 = DIRECTION('ref_axis',(0.995806686138499,0.0350088288095558,0.0845187893148275)) ;
#38538 = DIRECTION('center_axis',(0.,0.,1.)) ;
#38539 = DIRECTION('ref_axis',(1.,0.,0.)) ;
#38540 = DIRECTION('center_axis',(-0.0914824783325255,0.381078720623586,0.92000541566125)) ;
#38541 = DIRECTION('ref_axis',(0.995806686138499,0.0350088288095558,0.0845187893148275)) ;
#38542 = DIRECTION('center_axis',(0.091482478332531,-0.920005415661246,-0.381078720623595)) ;
#38543 = DIRECTION('ref_axis',(0.995806686138498,0.0845187893148324,0.0350088288095587)) ;
#38544 = DIRECTION('center_axis',(0.091482478332531,-0.920005415661246,-0.381078720623595)) ;
#38545 = DIRECTION('ref_axis',(0.995806686138498,0.0845187893148324,0.0350088288095587)) ;
#38546 = DIRECTION('center_axis',(0.,0.,1.)) ;
#38547 = DIRECTION('ref_axis',(1.,0.,0.)) ;
#38548 = DIRECTION('center_axis',(-0.091482478332531,0.920005415661246,0.381078720623595)) ;
#38549 = DIRECTION('ref_axis',(0.995806686138498,0.0845187893148324,0.0350088288095587)) ;
#38550 = DIRECTION('center_axis',(0.0914824783325236,-0.920005415661245,0.3810787206236)) ;
#38551 = DIRECTION('ref_axis',(0.995806686138499,0.0845187893148253,-0.0350088288095563)) ;
#38552 = DIRECTION('center_axis',(1.22464679914737E-16,-1.,0.)) ;
#38553 = DIRECTION('ref_axis',(-1.,-1.22464679914737E-16,0.)) ;
#38554 = DIRECTION('center_axis',(0.0914824783325236,-0.920005415661245,0.3810787206236)) ;
#38555 = DIRECTION('ref_axis',(0.995806686138499,0.0845187893148253,-0.0350088288095563)) ;
#38556 = DIRECTION('center_axis',(0.0914824783325236,-0.920005415661245,0.3810787206236)) ;
#38557 = DIRECTION('ref_axis',(0.995806686138499,0.0845187893148253,-0.0350088288095563)) ;
#38558 = DIRECTION('center_axis',(0.,0.,1.)) ;
#38559 = DIRECTION('ref_axis',(-0.0701393346692214,0.997537204184465,0.)) ;
#38560 = DIRECTION('center_axis',(-0.0914824783325236,0.920005415661245,-0.3810787206236)) ;
#38561 = DIRECTION('ref_axis',(0.995806686138499,0.0845187893148253,-0.0350088288095563)) ;
#38562 = DIRECTION('center_axis',(0.0914824783325314,-0.381078720623581,0.920005415661252)) ;
#38563 = DIRECTION('ref_axis',(0.995806686138498,0.0350088288095576,-0.0845187893148332)) ;
#38564 = DIRECTION('center_axis',(0.0914824783325314,-0.381078720623581,0.920005415661252)) ;
#38565 = DIRECTION('ref_axis',(0.995806686138498,0.0350088288095576,-0.0845187893148332)) ;
#38566 = DIRECTION('center_axis',(0.,0.,1.)) ;
#38567 = DIRECTION('ref_axis',(1.,0.,0.)) ;
#38568 = DIRECTION('center_axis',(-0.0914824783325314,0.381078720623581,-0.920005415661252)) ;
#38569 = DIRECTION('ref_axis',(0.995806686138498,0.0350088288095576,-0.0845187893148332)) ;
#38570 = DIRECTION('center_axis',(0.0914824783325263,0.381078720623593,0.920005415661247)) ;
#38571 = DIRECTION('ref_axis',(0.995806686138499,-0.0350088288095567,-0.0845187893148281)) ;
#38572 = DIRECTION('center_axis',(0.0914824783325263,0.381078720623593,0.920005415661247)) ;
#38573 = DIRECTION('ref_axis',(0.995806686138499,-0.0350088288095567,-0.0845187893148281)) ;
#38574 = DIRECTION('center_axis',(0.,0.,1.)) ;
#38575 = DIRECTION('ref_axis',(1.,0.,0.)) ;
#38576 = DIRECTION('center_axis',(-0.0914824783325263,-0.381078720623593,
-0.920005415661247)) ;
#38577 = DIRECTION('ref_axis',(0.995806686138499,-0.0350088288095567,-0.0845187893148281)) ;
#38578 = DIRECTION('center_axis',(0.0914824783325256,0.920005415661251,0.381078720623585)) ;
#38579 = DIRECTION('ref_axis',(0.995806686138499,-0.0845187893148277,-0.0350088288095557)) ;
#38580 = DIRECTION('center_axis',(0.0914824783325256,0.920005415661251,0.381078720623585)) ;
#38581 = DIRECTION('ref_axis',(0.995806686138499,-0.0845187893148277,-0.0350088288095557)) ;
#38582 = DIRECTION('center_axis',(0.,0.,1.)) ;
#38583 = DIRECTION('ref_axis',(1.,0.,0.)) ;
#38584 = DIRECTION('center_axis',(-0.0914824783325256,-0.920005415661251,
-0.381078720623585)) ;
#38585 = DIRECTION('ref_axis',(0.995806686138499,-0.0845187893148277,-0.0350088288095557)) ;
#38586 = DIRECTION('center_axis',(0.0914824783325317,0.920005415661254,-0.381078720623575)) ;
#38587 = DIRECTION('ref_axis',(0.995806686138498,-0.0845187893148337,0.0350088288095571)) ;
#38588 = DIRECTION('center_axis',(1.22464679914736E-16,-1.,0.)) ;
#38589 = DIRECTION('ref_axis',(-1.,-1.22464679914736E-16,0.)) ;
#38590 = DIRECTION('center_axis',(0.0914824783325317,0.920005415661254,-0.381078720623575)) ;
#38591 = DIRECTION('ref_axis',(0.995806686138498,-0.0845187893148337,0.0350088288095571)) ;
#38592 = DIRECTION('center_axis',(0.0914824783325317,0.920005415661254,-0.381078720623575)) ;
#38593 = DIRECTION('ref_axis',(0.995806686138498,-0.0845187893148337,0.0350088288095571)) ;
#38594 = DIRECTION('center_axis',(0.,0.,1.)) ;
#38595 = DIRECTION('ref_axis',(-0.0701393346692214,-0.997537204184465,0.)) ;
#38596 = DIRECTION('center_axis',(-0.0914824783325317,-0.920005415661254,
0.381078720623575)) ;
#38597 = DIRECTION('ref_axis',(0.995806686138498,-0.0845187893148337,0.0350088288095571)) ;
#38598 = DIRECTION('center_axis',(0.0914824783325234,0.381078720623582,-0.920005415661252)) ;
#38599 = DIRECTION('ref_axis',(0.995806686138499,-0.0350088288095545,0.0845187893148258)) ;
#38600 = DIRECTION('center_axis',(0.0914824783325234,0.381078720623582,-0.920005415661252)) ;
#38601 = DIRECTION('ref_axis',(0.995806686138499,-0.0350088288095545,0.0845187893148258)) ;
#38602 = DIRECTION('center_axis',(0.,0.,1.)) ;
#38603 = DIRECTION('ref_axis',(1.,0.,0.)) ;
#38604 = DIRECTION('center_axis',(-0.0914824783325234,-0.381078720623582,
0.920005415661252)) ;
#38605 = DIRECTION('ref_axis',(0.995806686138499,-0.0350088288095545,0.0845187893148258)) ;
#38606 = DIRECTION('center_axis',(0.091482478332531,-0.381078720623592,-0.920005415661248)) ;
#38607 = DIRECTION('ref_axis',(0.995806686138498,0.0350088288095584,0.0845187893148324)) ;
#38608 = DIRECTION('center_axis',(0.091482478332531,-0.381078720623592,-0.920005415661248)) ;
#38609 = DIRECTION('ref_axis',(0.995806686138498,0.0350088288095584,0.0845187893148324)) ;
#38610 = DIRECTION('center_axis',(0.,0.,1.)) ;
#38611 = DIRECTION('ref_axis',(1.,0.,0.)) ;
#38612 = DIRECTION('center_axis',(-0.091482478332531,0.381078720623592,0.920005415661248)) ;
#38613 = DIRECTION('ref_axis',(0.995806686138498,0.0350088288095584,0.0845187893148324)) ;
#38614 = DIRECTION('center_axis',(0.0914824783325255,-0.920005415661251,-0.381078720623585)) ;
#38615 = DIRECTION('ref_axis',(0.995806686138499,0.0845187893148276,0.0350088288095556)) ;
#38616 = DIRECTION('center_axis',(0.0914824783325255,-0.920005415661251,-0.381078720623585)) ;
#38617 = DIRECTION('ref_axis',(0.995806686138499,0.0845187893148276,0.0350088288095556)) ;
#38618 = DIRECTION('center_axis',(0.,0.,1.)) ;
#38619 = DIRECTION('ref_axis',(1.,0.,0.)) ;
#38620 = DIRECTION('center_axis',(-0.0914824783325255,0.920005415661251,0.381078720623585)) ;
#38621 = DIRECTION('ref_axis',(0.995806686138499,0.0845187893148276,0.0350088288095556)) ;
#38622 = DIRECTION('center_axis',(0.0914824783325253,-0.920005415661247,0.381078720623595)) ;
#38623 = DIRECTION('ref_axis',(0.995806686138499,0.084518789314827,-0.0350088288095565)) ;
#38624 = DIRECTION('center_axis',(1.22464679914737E-16,-1.,0.)) ;
#38625 = DIRECTION('ref_axis',(-1.,-1.22464679914737E-16,0.)) ;
#38626 = DIRECTION('center_axis',(0.0914824783325253,-0.920005415661247,0.381078720623595)) ;
#38627 = DIRECTION('ref_axis',(0.995806686138499,0.084518789314827,-0.0350088288095565)) ;
#38628 = DIRECTION('center_axis',(0.0914824783325253,-0.920005415661247,0.381078720623595)) ;
#38629 = DIRECTION('ref_axis',(0.995806686138499,0.084518789314827,-0.0350088288095565)) ;
#38630 = DIRECTION('center_axis',(0.,0.,1.)) ;
#38631 = DIRECTION('ref_axis',(-0.0701393346691978,0.997537204184467,0.)) ;
#38632 = DIRECTION('center_axis',(-0.0914824783325253,0.920005415661247,-0.381078720623595)) ;
#38633 = DIRECTION('ref_axis',(0.995806686138499,0.084518789314827,-0.0350088288095565)) ;
#38634 = DIRECTION('center_axis',(0.0914824783325311,-0.381078720623587,0.920005415661249)) ;
#38635 = DIRECTION('ref_axis',(0.995806686138498,0.035008828809558,-0.0845187893148328)) ;
#38636 = DIRECTION('center_axis',(0.0914824783325311,-0.381078720623587,0.920005415661249)) ;
#38637 = DIRECTION('ref_axis',(0.995806686138498,0.035008828809558,-0.0845187893148328)) ;
#38638 = DIRECTION('center_axis',(0.,0.,1.)) ;
#38639 = DIRECTION('ref_axis',(1.,0.,0.)) ;
#38640 = DIRECTION('center_axis',(-0.0914824783325311,0.381078720623587,-0.920005415661249)) ;
#38641 = DIRECTION('ref_axis',(0.995806686138498,0.035008828809558,-0.0845187893148328)) ;
#38642 = DIRECTION('center_axis',(0.0914824783325242,0.38107872062359,0.920005415661249)) ;
#38643 = DIRECTION('ref_axis',(0.995806686138499,-0.0350088288095556,-0.0845187893148262)) ;
#38644 = DIRECTION('center_axis',(0.0914824783325242,0.38107872062359,0.920005415661249)) ;
#38645 = DIRECTION('ref_axis',(0.995806686138499,-0.0350088288095556,-0.0845187893148262)) ;
#38646 = DIRECTION('center_axis',(0.,0.,1.)) ;
#38647 = DIRECTION('ref_axis',(1.,0.,0.)) ;
#38648 = DIRECTION('center_axis',(-0.0914824783325242,-0.38107872062359,-0.920005415661249)) ;
#38649 = DIRECTION('ref_axis',(0.995806686138499,-0.0350088288095556,-0.0845187893148262)) ;
#38650 = DIRECTION('center_axis',(0.0914824783325315,0.920005415661255,0.381078720623574)) ;
#38651 = DIRECTION('ref_axis',(0.995806686138498,-0.0845187893148336,-0.035008828809557)) ;
#38652 = DIRECTION('center_axis',(0.0914824783325315,0.920005415661255,0.381078720623574)) ;
#38653 = DIRECTION('ref_axis',(0.995806686138498,-0.0845187893148336,-0.035008828809557)) ;
#38654 = DIRECTION('center_axis',(0.,0.,1.)) ;
#38655 = DIRECTION('ref_axis',(1.,0.,0.)) ;
#38656 = DIRECTION('center_axis',(-0.0914824783325315,-0.920005415661255,
-0.381078720623574)) ;
#38657 = DIRECTION('ref_axis',(0.995806686138498,-0.0845187893148336,-0.035008828809557)) ;
#38658 = DIRECTION('center_axis',(0.0914824783325258,0.92000541566125,-0.381078720623586)) ;
#38659 = DIRECTION('ref_axis',(0.995806686138499,-0.0845187893148279,0.0350088288095559)) ;
#38660 = DIRECTION('center_axis',(1.22464679914737E-16,-1.,0.)) ;
#38661 = DIRECTION('ref_axis',(-1.,-1.22464679914737E-16,0.)) ;
#38662 = DIRECTION('center_axis',(0.0914824783325258,0.92000541566125,-0.381078720623586)) ;
#38663 = DIRECTION('ref_axis',(0.995806686138499,-0.0845187893148279,0.0350088288095559)) ;
#38664 = DIRECTION('center_axis',(0.0914824783325258,0.92000541566125,-0.381078720623586)) ;
#38665 = DIRECTION('ref_axis',(0.995806686138499,-0.0845187893148279,0.0350088288095559)) ;
#38666 = DIRECTION('center_axis',(0.,0.,1.)) ;
#38667 = DIRECTION('ref_axis',(-0.0701393346692214,-0.997537204184465,0.)) ;
#38668 = DIRECTION('center_axis',(-0.0914824783325258,-0.92000541566125,0.381078720623586)) ;
#38669 = DIRECTION('ref_axis',(0.995806686138499,-0.0845187893148279,0.0350088288095559)) ;
#38670 = DIRECTION('center_axis',(0.0914824783325255,0.381078720623584,-0.920005415661251)) ;
#38671 = DIRECTION('ref_axis',(0.995806686138499,-0.0350088288095556,0.0845187893148277)) ;
#38672 = DIRECTION('center_axis',(0.0914824783325255,0.381078720623584,-0.920005415661251)) ;
#38673 = DIRECTION('ref_axis',(0.995806686138499,-0.0350088288095556,0.0845187893148277)) ;
#38674 = DIRECTION('center_axis',(0.,0.,1.)) ;
#38675 = DIRECTION('ref_axis',(1.,0.,0.)) ;
#38676 = DIRECTION('center_axis',(-0.0914824783325255,-0.381078720623584,
0.920005415661251)) ;
#38677 = DIRECTION('ref_axis',(0.995806686138499,-0.0350088288095556,0.0845187893148277)) ;
#38678 = DIRECTION('center_axis',(0.0914824783325312,-0.381078720623586,-0.92000541566125)) ;
#38679 = DIRECTION('ref_axis',(0.995806686138498,0.0350088288095579,0.0845187893148329)) ;
#38680 = DIRECTION('center_axis',(0.0914824783325312,-0.381078720623586,-0.92000541566125)) ;
#38681 = DIRECTION('ref_axis',(0.995806686138498,0.0350088288095579,0.0845187893148329)) ;
#38682 = DIRECTION('center_axis',(0.,0.,1.)) ;
#38683 = DIRECTION('ref_axis',(1.,0.,0.)) ;
#38684 = DIRECTION('center_axis',(-0.0914824783325312,0.381078720623586,0.92000541566125)) ;
#38685 = DIRECTION('ref_axis',(0.995806686138498,0.0350088288095579,0.0845187893148329)) ;
#38686 = DIRECTION('center_axis',(0.0914824783325238,-0.920005415661249,-0.381078720623589)) ;
#38687 = DIRECTION('ref_axis',(0.995806686138499,0.0845187893148259,0.0350088288095554)) ;
#38688 = DIRECTION('center_axis',(0.0914824783325238,-0.920005415661249,-0.381078720623589)) ;
#38689 = DIRECTION('ref_axis',(0.995806686138499,0.0845187893148259,0.0350088288095554)) ;
#38690 = DIRECTION('center_axis',(0.,0.,1.)) ;
#38691 = DIRECTION('ref_axis',(1.,0.,0.)) ;
#38692 = DIRECTION('center_axis',(-0.0914824783325238,0.920005415661249,0.381078720623589)) ;
#38693 = DIRECTION('ref_axis',(0.995806686138499,0.0845187893148259,0.0350088288095554)) ;
#38694 = DIRECTION('center_axis',(0.0914824783325308,-0.920005415661242,0.381078720623606)) ;
#38695 = DIRECTION('ref_axis',(0.995806686138498,0.0845187893148317,-0.0350088288095596)) ;
#38696 = DIRECTION('center_axis',(1.22464679914732E-16,-1.,0.)) ;
#38697 = DIRECTION('ref_axis',(-1.,-1.22464679914732E-16,0.)) ;
#38698 = DIRECTION('center_axis',(0.0914824783325308,-0.920005415661242,0.381078720623606)) ;
#38699 = DIRECTION('ref_axis',(0.995806686138498,0.0845187893148317,-0.0350088288095596)) ;
#38700 = DIRECTION('center_axis',(0.0914824783325308,-0.920005415661242,0.381078720623606)) ;
#38701 = DIRECTION('ref_axis',(0.995806686138498,0.0845187893148317,-0.0350088288095596)) ;
#38702 = DIRECTION('center_axis',(0.,0.,1.)) ;
#38703 = DIRECTION('ref_axis',(-0.0701393346692214,0.997537204184465,0.)) ;
#38704 = DIRECTION('center_axis',(-0.0914824783325308,0.920005415661242,-0.381078720623606)) ;
#38705 = DIRECTION('ref_axis',(0.995806686138498,0.0845187893148317,-0.0350088288095596)) ;
#38706 = DIRECTION('center_axis',(0.0914824783325257,-0.381078720623582,0.920005415661252)) ;
#38707 = DIRECTION('ref_axis',(0.995806686138499,0.0350088288095554,-0.0845187893148279)) ;
#38708 = DIRECTION('center_axis',(0.0914824783325257,-0.381078720623582,0.920005415661252)) ;
#38709 = DIRECTION('ref_axis',(0.995806686138499,0.0350088288095554,-0.0845187893148279)) ;
#38710 = DIRECTION('center_axis',(0.,0.,1.)) ;
#38711 = DIRECTION('ref_axis',(1.,0.,0.)) ;
#38712 = DIRECTION('center_axis',(-0.0914824783325257,0.381078720623582,-0.920005415661252)) ;
#38713 = DIRECTION('ref_axis',(0.995806686138499,0.0350088288095554,-0.0845187893148279)) ;
#38714 = DIRECTION('center_axis',(0.0914824783325263,0.381078720623592,0.920005415661247)) ;
#38715 = DIRECTION('ref_axis',(0.995806686138499,-0.0350088288095567,-0.0845187893148281)) ;
#38716 = DIRECTION('center_axis',(0.0914824783325263,0.381078720623592,0.920005415661247)) ;
#38717 = DIRECTION('ref_axis',(0.995806686138499,-0.0350088288095567,-0.0845187893148281)) ;
#38718 = DIRECTION('center_axis',(0.,0.,1.)) ;
#38719 = DIRECTION('ref_axis',(1.,0.,0.)) ;
#38720 = DIRECTION('center_axis',(-0.0914824783325263,-0.381078720623592,
-0.920005415661247)) ;
#38721 = DIRECTION('ref_axis',(0.995806686138499,-0.0350088288095567,-0.0845187893148281)) ;
#38722 = DIRECTION('center_axis',(0.0914824783325313,0.92000541566125,0.381078720623585)) ;
#38723 = DIRECTION('ref_axis',(0.995806686138498,-0.084518789314833,-0.0350088288095579)) ;
#38724 = DIRECTION('center_axis',(0.0914824783325313,0.92000541566125,0.381078720623585)) ;
#38725 = DIRECTION('ref_axis',(0.995806686138498,-0.084518789314833,-0.0350088288095579)) ;
#38726 = DIRECTION('center_axis',(0.,0.,1.)) ;
#38727 = DIRECTION('ref_axis',(1.,0.,0.)) ;
#38728 = DIRECTION('center_axis',(-0.0914824783325313,-0.92000541566125,-0.381078720623585)) ;
#38729 = DIRECTION('ref_axis',(0.995806686138498,-0.084518789314833,-0.0350088288095579)) ;
#38730 = DIRECTION('center_axis',(0.091482478332526,0.920005415661255,-0.381078720623575)) ;
#38731 = DIRECTION('ref_axis',(0.995806686138499,-0.0845187893148284,0.0350088288095549)) ;
#38732 = DIRECTION('center_axis',(1.22464679914737E-16,-1.,0.)) ;
#38733 = DIRECTION('ref_axis',(-1.,-1.22464679914737E-16,0.)) ;
#38734 = DIRECTION('center_axis',(0.091482478332526,0.920005415661255,-0.381078720623575)) ;
#38735 = DIRECTION('ref_axis',(0.995806686138499,-0.0845187893148284,0.0350088288095549)) ;
#38736 = DIRECTION('center_axis',(0.091482478332526,0.920005415661255,-0.381078720623575)) ;
#38737 = DIRECTION('ref_axis',(0.995806686138499,-0.0845187893148284,0.0350088288095549)) ;
#38738 = DIRECTION('center_axis',(0.,0.,1.)) ;
#38739 = DIRECTION('ref_axis',(-0.0701393346692214,-0.997537204184465,0.)) ;
#38740 = DIRECTION('center_axis',(-0.091482478332526,-0.920005415661255,0.381078720623575)) ;
#38741 = DIRECTION('ref_axis',(0.995806686138499,-0.0845187893148284,0.0350088288095549)) ;
#38742 = DIRECTION('center_axis',(0.0914824783325291,0.381078720623582,-0.920005415661252)) ;
#38743 = DIRECTION('ref_axis',(0.995806686138499,-0.0350088288095568,0.0845187893148311)) ;
#38744 = DIRECTION('center_axis',(0.0914824783325291,0.381078720623582,-0.920005415661252)) ;
#38745 = DIRECTION('ref_axis',(0.995806686138499,-0.0350088288095568,0.0845187893148311)) ;
#38746 = DIRECTION('center_axis',(0.,0.,1.)) ;
#38747 = DIRECTION('ref_axis',(1.,0.,0.)) ;
#38748 = DIRECTION('center_axis',(-0.0914824783325291,-0.381078720623582,
0.920005415661252)) ;
#38749 = DIRECTION('ref_axis',(0.995806686138499,-0.0350088288095568,0.0845187893148311)) ;
#38750 = DIRECTION('center_axis',(0.0914824783325252,-0.381078720623591,-0.920005415661248)) ;
#38751 = DIRECTION('ref_axis',(0.995806686138499,0.0350088288095562,0.0845187893148272)) ;
#38752 = DIRECTION('center_axis',(0.0914824783325252,-0.381078720623591,-0.920005415661248)) ;
#38753 = DIRECTION('ref_axis',(0.995806686138499,0.0350088288095562,0.0845187893148272)) ;
#38754 = DIRECTION('center_axis',(0.,0.,1.)) ;
#38755 = DIRECTION('ref_axis',(1.,0.,0.)) ;
#38756 = DIRECTION('center_axis',(-0.0914824783325252,0.381078720623591,0.920005415661248)) ;
#38757 = DIRECTION('ref_axis',(0.995806686138499,0.0350088288095562,0.0845187893148272)) ;
#38758 = DIRECTION('center_axis',(0.0914824783325255,-0.920005415661251,-0.381078720623585)) ;
#38759 = DIRECTION('ref_axis',(0.995806686138499,0.0845187893148276,0.0350088288095556)) ;
#38760 = DIRECTION('center_axis',(0.0914824783325255,-0.920005415661251,-0.381078720623585)) ;
#38761 = DIRECTION('ref_axis',(0.995806686138499,0.0845187893148276,0.0350088288095556)) ;
#38762 = DIRECTION('center_axis',(0.,0.,1.)) ;
#38763 = DIRECTION('ref_axis',(1.,0.,0.)) ;
#38764 = DIRECTION('center_axis',(-0.0914824783325255,0.920005415661251,0.381078720623585)) ;
#38765 = DIRECTION('ref_axis',(0.995806686138499,0.0845187893148276,0.0350088288095556)) ;
#38766 = DIRECTION('center_axis',(0.091482478332531,-0.920005415661246,0.381078720623595)) ;
#38767 = DIRECTION('ref_axis',(0.995806686138498,0.0845187893148323,-0.0350088288095587)) ;
#38768 = DIRECTION('center_axis',(1.22464679914737E-16,-1.,0.)) ;
#38769 = DIRECTION('ref_axis',(-1.,-1.22464679914737E-16,0.)) ;
#38770 = DIRECTION('center_axis',(0.091482478332531,-0.920005415661246,0.381078720623595)) ;
#38771 = DIRECTION('ref_axis',(0.995806686138498,0.0845187893148323,-0.0350088288095587)) ;
#38772 = DIRECTION('center_axis',(0.091482478332531,-0.920005415661246,0.381078720623595)) ;
#38773 = DIRECTION('ref_axis',(0.995806686138498,0.0845187893148323,-0.0350088288095587)) ;
#38774 = DIRECTION('center_axis',(0.,0.,1.)) ;
#38775 = DIRECTION('ref_axis',(-0.0701393346692214,0.997537204184465,0.)) ;
#38776 = DIRECTION('center_axis',(-0.091482478332531,0.920005415661246,-0.381078720623595)) ;
#38777 = DIRECTION('ref_axis',(0.995806686138498,0.0845187893148323,-0.0350088288095587)) ;
#38778 = DIRECTION('center_axis',(0.0914824783325244,-0.381078720623583,0.920005415661252)) ;
#38779 = DIRECTION('ref_axis',(0.995806686138499,0.0350088288095551,-0.0845187893148267)) ;
#38780 = DIRECTION('center_axis',(0.0914824783325244,-0.381078720623583,0.920005415661252)) ;
#38781 = DIRECTION('ref_axis',(0.995806686138499,0.0350088288095551,-0.0845187893148267)) ;
#38782 = DIRECTION('center_axis',(0.,0.,1.)) ;
#38783 = DIRECTION('ref_axis',(1.,0.,0.)) ;
#38784 = DIRECTION('center_axis',(-0.0914824783325244,0.381078720623583,-0.920005415661252)) ;
#38785 = DIRECTION('ref_axis',(0.995806686138499,0.0350088288095551,-0.0845187893148267)) ;
#38786 = DIRECTION('center_axis',(0.0914824783325321,0.381078720623592,0.920005415661247)) ;
#38787 = DIRECTION('ref_axis',(0.995806686138498,-0.0350088288095589,-0.0845187893148334)) ;
#38788 = DIRECTION('center_axis',(0.0914824783325321,0.381078720623592,0.920005415661247)) ;
#38789 = DIRECTION('ref_axis',(0.995806686138498,-0.0350088288095589,-0.0845187893148334)) ;
#38790 = DIRECTION('center_axis',(0.,0.,1.)) ;
#38791 = DIRECTION('ref_axis',(1.,0.,0.)) ;
#38792 = DIRECTION('center_axis',(-0.0914824783325321,-0.381078720623592,
-0.920005415661247)) ;
#38793 = DIRECTION('ref_axis',(0.995806686138498,-0.0350088288095589,-0.0845187893148334)) ;
#38794 = DIRECTION('center_axis',(0.0914824783325248,0.920005415661252,0.381078720623582)) ;
#38795 = DIRECTION('ref_axis',(0.995806686138499,-0.0845187893148271,-0.0350088288095551)) ;
#38796 = DIRECTION('center_axis',(0.0914824783325248,0.920005415661252,0.381078720623582)) ;
#38797 = DIRECTION('ref_axis',(0.995806686138499,-0.0845187893148271,-0.0350088288095551)) ;
#38798 = DIRECTION('center_axis',(0.,0.,1.)) ;
#38799 = DIRECTION('ref_axis',(1.,0.,0.)) ;
#38800 = DIRECTION('center_axis',(-0.0914824783325248,-0.920005415661252,
-0.381078720623582)) ;
#38801 = DIRECTION('ref_axis',(0.995806686138499,-0.0845187893148271,-0.0350088288095551)) ;
#38802 = DIRECTION('center_axis',(0.0914824783325258,0.92000541566125,-0.381078720623586)) ;
#38803 = DIRECTION('ref_axis',(0.995806686138499,-0.0845187893148278,0.0350088288095558)) ;
#38804 = DIRECTION('center_axis',(1.22464679914737E-16,-1.,0.)) ;
#38805 = DIRECTION('ref_axis',(-1.,-1.22464679914737E-16,0.)) ;
#38806 = DIRECTION('center_axis',(0.0914824783325258,0.92000541566125,-0.381078720623586)) ;
#38807 = DIRECTION('ref_axis',(0.995806686138499,-0.0845187893148278,0.0350088288095558)) ;
#38808 = DIRECTION('center_axis',(0.0914824783325258,0.92000541566125,-0.381078720623586)) ;
#38809 = DIRECTION('ref_axis',(0.995806686138499,-0.0845187893148278,0.0350088288095558)) ;
#38810 = DIRECTION('center_axis',(0.,0.,1.)) ;
#38811 = DIRECTION('ref_axis',(-0.0701393346692214,-0.997537204184465,0.)) ;
#38812 = DIRECTION('center_axis',(-0.0914824783325258,-0.92000541566125,0.381078720623586)) ;
#38813 = DIRECTION('ref_axis',(0.995806686138499,-0.0845187893148278,0.0350088288095558)) ;
#38814 = DIRECTION('center_axis',(0.0914824783325312,0.381078720623584,-0.92000541566125)) ;
#38815 = DIRECTION('ref_axis',(0.995806686138498,-0.0350088288095578,0.084518789314833)) ;
#38816 = DIRECTION('center_axis',(0.0914824783325312,0.381078720623584,-0.92000541566125)) ;
#38817 = DIRECTION('ref_axis',(0.995806686138498,-0.0350088288095578,0.084518789314833)) ;
#38818 = DIRECTION('center_axis',(0.,0.,1.)) ;
#38819 = DIRECTION('ref_axis',(1.,0.,0.)) ;
#38820 = DIRECTION('center_axis',(-0.0914824783325312,-0.381078720623584,
0.92000541566125)) ;
#38821 = DIRECTION('ref_axis',(0.995806686138498,-0.0350088288095578,0.084518789314833)) ;
#38822 = DIRECTION('center_axis',(0.0914824783325243,-0.381078720623587,-0.92000541566125)) ;
#38823 = DIRECTION('ref_axis',(0.995806686138499,0.0350088288095554,0.0845187893148264)) ;
#38824 = DIRECTION('center_axis',(0.0914824783325243,-0.381078720623587,-0.92000541566125)) ;
#38825 = DIRECTION('ref_axis',(0.995806686138499,0.0350088288095554,0.0845187893148264)) ;
#38826 = DIRECTION('center_axis',(0.,0.,1.)) ;
#38827 = DIRECTION('ref_axis',(1.,0.,0.)) ;
#38828 = DIRECTION('center_axis',(-0.0914824783325243,0.381078720623587,0.92000541566125)) ;
#38829 = DIRECTION('ref_axis',(0.995806686138499,0.0350088288095554,0.0845187893148264)) ;
#38830 = DIRECTION('center_axis',(0.0914824783325312,-0.92000541566125,-0.381078720623584)) ;
#38831 = DIRECTION('ref_axis',(0.995806686138498,0.0845187893148329,0.0350088288095578)) ;
#38832 = DIRECTION('center_axis',(0.0914824783325312,-0.92000541566125,-0.381078720623584)) ;
#38833 = DIRECTION('ref_axis',(0.995806686138498,0.0845187893148329,0.0350088288095578)) ;
#38834 = DIRECTION('center_axis',(0.,0.,1.)) ;
#38835 = DIRECTION('ref_axis',(1.,0.,0.)) ;
#38836 = DIRECTION('center_axis',(-0.0914824783325312,0.92000541566125,0.381078720623584)) ;
#38837 = DIRECTION('ref_axis',(0.995806686138498,0.0845187893148329,0.0350088288095578)) ;
#38838 = DIRECTION('center_axis',(0.0914824783325252,-0.920005415661246,0.381078720623595)) ;
#38839 = DIRECTION('ref_axis',(0.995806686138499,0.084518789314827,-0.0350088288095565)) ;
#38840 = DIRECTION('center_axis',(1.22464679914736E-16,-1.,0.)) ;
#38841 = DIRECTION('ref_axis',(-1.,-1.22464679914736E-16,0.)) ;
#38842 = DIRECTION('center_axis',(0.0914824783325252,-0.920005415661246,0.381078720623595)) ;
#38843 = DIRECTION('ref_axis',(0.995806686138499,0.084518789314827,-0.0350088288095565)) ;
#38844 = DIRECTION('center_axis',(0.0914824783325252,-0.920005415661246,0.381078720623595)) ;
#38845 = DIRECTION('ref_axis',(0.995806686138499,0.084518789314827,-0.0350088288095565)) ;
#38846 = DIRECTION('center_axis',(0.,0.,1.)) ;
#38847 = DIRECTION('ref_axis',(-0.0701393346691978,0.997537204184467,0.)) ;
#38848 = DIRECTION('center_axis',(-0.0914824783325252,0.920005415661246,-0.381078720623595)) ;
#38849 = DIRECTION('ref_axis',(0.995806686138499,0.084518789314827,-0.0350088288095565)) ;
#38850 = DIRECTION('center_axis',(0.0914824783325244,-0.381078720623584,0.920005415661252)) ;
#38851 = DIRECTION('ref_axis',(0.995806686138499,0.0350088288095551,-0.0845187893148267)) ;
#38852 = DIRECTION('center_axis',(0.0914824783325244,-0.381078720623584,0.920005415661252)) ;
#38853 = DIRECTION('ref_axis',(0.995806686138499,0.0350088288095551,-0.0845187893148267)) ;
#38854 = DIRECTION('center_axis',(0.,0.,1.)) ;
#38855 = DIRECTION('ref_axis',(1.,0.,0.)) ;
#38856 = DIRECTION('center_axis',(-0.0914824783325244,0.381078720623584,-0.920005415661252)) ;
#38857 = DIRECTION('ref_axis',(0.995806686138499,0.0350088288095551,-0.0845187893148267)) ;
#38858 = DIRECTION('center_axis',(0.0914824783325321,0.381078720623592,0.920005415661247)) ;
#38859 = DIRECTION('ref_axis',(0.995806686138498,-0.0350088288095588,-0.0845187893148334)) ;
#38860 = DIRECTION('center_axis',(0.0914824783325321,0.381078720623592,0.920005415661247)) ;
#38861 = DIRECTION('ref_axis',(0.995806686138498,-0.0350088288095588,-0.0845187893148334)) ;
#38862 = DIRECTION('center_axis',(0.,0.,1.)) ;
#38863 = DIRECTION('ref_axis',(1.,0.,0.)) ;
#38864 = DIRECTION('center_axis',(-0.0914824783325321,-0.381078720623592,
-0.920005415661247)) ;
#38865 = DIRECTION('ref_axis',(0.995806686138498,-0.0350088288095588,-0.0845187893148334)) ;
#38866 = DIRECTION('center_axis',(0.0914824783325256,0.920005415661251,0.381078720623585)) ;
#38867 = DIRECTION('ref_axis',(0.995806686138499,-0.0845187893148278,-0.0350088288095557)) ;
#38868 = DIRECTION('center_axis',(0.0914824783325256,0.920005415661251,0.381078720623585)) ;
#38869 = DIRECTION('ref_axis',(0.995806686138499,-0.0845187893148278,-0.0350088288095557)) ;
#38870 = DIRECTION('center_axis',(0.,0.,1.)) ;
#38871 = DIRECTION('ref_axis',(1.,0.,0.)) ;
#38872 = DIRECTION('center_axis',(-0.0914824783325256,-0.920005415661251,
-0.381078720623585)) ;
#38873 = DIRECTION('ref_axis',(0.995806686138499,-0.0845187893148278,-0.0350088288095557)) ;
#38874 = DIRECTION('center_axis',(0.0914824783325307,0.920005415661251,-0.381078720623582)) ;
#38875 = DIRECTION('ref_axis',(0.995806686138498,-0.0845187893148325,0.0350088288095574)) ;
#38876 = DIRECTION('center_axis',(1.22464679914736E-16,-1.,0.)) ;
#38877 = DIRECTION('ref_axis',(-1.,-1.22464679914736E-16,0.)) ;
#38878 = DIRECTION('center_axis',(0.0914824783325307,0.920005415661251,-0.381078720623582)) ;
#38879 = DIRECTION('ref_axis',(0.995806686138498,-0.0845187893148325,0.0350088288095574)) ;
#38880 = DIRECTION('center_axis',(0.0914824783325307,0.920005415661251,-0.381078720623582)) ;
#38881 = DIRECTION('ref_axis',(0.995806686138498,-0.0845187893148325,0.0350088288095574)) ;
#38882 = DIRECTION('center_axis',(0.,0.,1.)) ;
#38883 = DIRECTION('ref_axis',(-0.0701393346692214,-0.997537204184465,0.)) ;
#38884 = DIRECTION('center_axis',(-0.0914824783325307,-0.920005415661251,
0.381078720623582)) ;
#38885 = DIRECTION('ref_axis',(0.995806686138498,-0.0845187893148325,0.0350088288095574)) ;
#38886 = DIRECTION('center_axis',(0.0914824783325255,0.381078720623585,-0.920005415661251)) ;
#38887 = DIRECTION('ref_axis',(0.995806686138499,-0.0350088288095557,0.0845187893148276)) ;
#38888 = DIRECTION('center_axis',(0.0914824783325255,0.381078720623585,-0.920005415661251)) ;
#38889 = DIRECTION('ref_axis',(0.995806686138499,-0.0350088288095557,0.0845187893148276)) ;
#38890 = DIRECTION('center_axis',(0.,0.,1.)) ;
#38891 = DIRECTION('ref_axis',(1.,0.,0.)) ;
#38892 = DIRECTION('center_axis',(-0.0914824783325255,-0.381078720623585,
0.920005415661251)) ;
#38893 = DIRECTION('ref_axis',(0.995806686138499,-0.0350088288095557,0.0845187893148276)) ;
#38894 = DIRECTION('center_axis',(0.0914824783325243,-0.381078720623587,-0.92000541566125)) ;
#38895 = DIRECTION('ref_axis',(0.995806686138499,0.0350088288095554,0.0845187893148264)) ;
#38896 = DIRECTION('center_axis',(0.0914824783325243,-0.381078720623587,-0.92000541566125)) ;
#38897 = DIRECTION('ref_axis',(0.995806686138499,0.0350088288095554,0.0845187893148264)) ;
#38898 = DIRECTION('center_axis',(0.,0.,1.)) ;
#38899 = DIRECTION('ref_axis',(1.,0.,0.)) ;
#38900 = DIRECTION('center_axis',(-0.0914824783325243,0.381078720623587,0.92000541566125)) ;
#38901 = DIRECTION('ref_axis',(0.995806686138499,0.0350088288095554,0.0845187893148264)) ;
#38902 = DIRECTION('center_axis',(0.0914824783325312,-0.92000541566125,-0.381078720623584)) ;
#38903 = DIRECTION('ref_axis',(0.995806686138498,0.0845187893148329,0.0350088288095578)) ;
#38904 = DIRECTION('center_axis',(0.0914824783325312,-0.92000541566125,-0.381078720623584)) ;
#38905 = DIRECTION('ref_axis',(0.995806686138498,0.0845187893148329,0.0350088288095578)) ;
#38906 = DIRECTION('center_axis',(0.,0.,1.)) ;
#38907 = DIRECTION('ref_axis',(1.,0.,0.)) ;
#38908 = DIRECTION('center_axis',(-0.0914824783325312,0.92000541566125,0.381078720623584)) ;
#38909 = DIRECTION('ref_axis',(0.995806686138498,0.0845187893148329,0.0350088288095578)) ;
#38910 = DIRECTION('center_axis',(0.0914824783325252,-0.920005415661246,0.381078720623595)) ;
#38911 = DIRECTION('ref_axis',(0.995806686138499,0.084518789314827,-0.0350088288095565)) ;
#38912 = DIRECTION('center_axis',(1.22464679914736E-16,-1.,0.)) ;
#38913 = DIRECTION('ref_axis',(-1.,-1.22464679914736E-16,0.)) ;
#38914 = DIRECTION('center_axis',(0.0914824783325252,-0.920005415661246,0.381078720623595)) ;
#38915 = DIRECTION('ref_axis',(0.995806686138499,0.084518789314827,-0.0350088288095565)) ;
#38916 = DIRECTION('center_axis',(0.0914824783325252,-0.920005415661246,0.381078720623595)) ;
#38917 = DIRECTION('ref_axis',(0.995806686138499,0.084518789314827,-0.0350088288095565)) ;
#38918 = DIRECTION('center_axis',(0.,0.,1.)) ;
#38919 = DIRECTION('ref_axis',(-0.0701393346691978,0.997537204184467,0.)) ;
#38920 = DIRECTION('center_axis',(-0.0914824783325252,0.920005415661246,-0.381078720623595)) ;
#38921 = DIRECTION('ref_axis',(0.995806686138499,0.084518789314827,-0.0350088288095565)) ;
#38922 = DIRECTION('center_axis',(0.0914824783325302,-0.381078720623583,0.920005415661251)) ;
#38923 = DIRECTION('ref_axis',(0.995806686138499,0.0350088288095573,-0.084518789314832)) ;
#38924 = DIRECTION('center_axis',(0.0914824783325302,-0.381078720623583,0.920005415661251)) ;
#38925 = DIRECTION('ref_axis',(0.995806686138499,0.0350088288095573,-0.084518789314832)) ;
#38926 = DIRECTION('center_axis',(0.,0.,1.)) ;
#38927 = DIRECTION('ref_axis',(1.,0.,0.)) ;
#38928 = DIRECTION('center_axis',(-0.0914824783325302,0.381078720623583,-0.920005415661251)) ;
#38929 = DIRECTION('ref_axis',(0.995806686138499,0.0350088288095573,-0.084518789314832)) ;
#38930 = DIRECTION('center_axis',(0.0914824783325264,0.381078720623592,0.920005415661248)) ;
#38931 = DIRECTION('ref_axis',(0.995806686138499,-0.0350088288095566,-0.0845187893148281)) ;
#38932 = DIRECTION('center_axis',(0.0914824783325264,0.381078720623592,0.920005415661248)) ;
#38933 = DIRECTION('ref_axis',(0.995806686138499,-0.0350088288095566,-0.0845187893148281)) ;
#38934 = DIRECTION('center_axis',(0.,0.,1.)) ;
#38935 = DIRECTION('ref_axis',(1.,0.,0.)) ;
#38936 = DIRECTION('center_axis',(-0.0914824783325264,-0.381078720623592,
-0.920005415661248)) ;
#38937 = DIRECTION('ref_axis',(0.995806686138499,-0.0350088288095566,-0.0845187893148281)) ;
#38938 = DIRECTION('center_axis',(0.0914824783325249,0.920005415661252,0.381078720623582)) ;
#38939 = DIRECTION('ref_axis',(0.995806686138499,-0.0845187893148272,-0.0350088288095551)) ;
#38940 = DIRECTION('center_axis',(0.0914824783325249,0.920005415661252,0.381078720623582)) ;
#38941 = DIRECTION('ref_axis',(0.995806686138499,-0.0845187893148272,-0.0350088288095551)) ;
#38942 = DIRECTION('center_axis',(0.,0.,1.)) ;
#38943 = DIRECTION('ref_axis',(1.,0.,0.)) ;
#38944 = DIRECTION('center_axis',(-0.0914824783325249,-0.920005415661252,
-0.381078720623582)) ;
#38945 = DIRECTION('ref_axis',(0.995806686138499,-0.0845187893148272,-0.0350088288095551)) ;
#38946 = DIRECTION('center_axis',(0.0914824783325315,0.92000541566125,-0.381078720623585)) ;
#38947 = DIRECTION('ref_axis',(0.995806686138498,-0.0845187893148331,0.035008828809558)) ;
#38948 = DIRECTION('center_axis',(1.22464679914737E-16,-1.,0.)) ;
#38949 = DIRECTION('ref_axis',(-1.,-1.22464679914737E-16,0.)) ;
#38950 = DIRECTION('center_axis',(0.0914824783325315,0.92000541566125,-0.381078720623585)) ;
#38951 = DIRECTION('ref_axis',(0.995806686138498,-0.0845187893148331,0.035008828809558)) ;
#38952 = DIRECTION('center_axis',(0.0914824783325315,0.92000541566125,-0.381078720623585)) ;
#38953 = DIRECTION('ref_axis',(0.995806686138498,-0.0845187893148331,0.035008828809558)) ;
#38954 = DIRECTION('center_axis',(0.,0.,1.)) ;
#38955 = DIRECTION('ref_axis',(-0.0701393346692214,-0.997537204184465,0.)) ;
#38956 = DIRECTION('center_axis',(-0.0914824783325315,-0.92000541566125,0.381078720623585)) ;
#38957 = DIRECTION('ref_axis',(0.995806686138498,-0.0845187893148331,0.035008828809558)) ;
#38958 = DIRECTION('center_axis',(0.0914824783325255,0.381078720623585,-0.920005415661251)) ;
#38959 = DIRECTION('ref_axis',(0.995806686138499,-0.0350088288095557,0.0845187893148276)) ;
#38960 = DIRECTION('center_axis',(0.0914824783325255,0.381078720623585,-0.920005415661251)) ;
#38961 = DIRECTION('ref_axis',(0.995806686138499,-0.0350088288095557,0.0845187893148276)) ;
#38962 = DIRECTION('center_axis',(0.,0.,1.)) ;
#38963 = DIRECTION('ref_axis',(1.,0.,0.)) ;
#38964 = DIRECTION('center_axis',(-0.0914824783325255,-0.381078720623585,
0.920005415661251)) ;
#38965 = DIRECTION('ref_axis',(0.995806686138499,-0.0350088288095557,0.0845187893148276)) ;
#38966 = DIRECTION('center_axis',(0.09148247833253,-0.381078720623586,-0.92000541566125)) ;
#38967 = DIRECTION('ref_axis',(0.995806686138499,0.0350088288095576,0.0845187893148318)) ;
#38968 = DIRECTION('center_axis',(0.09148247833253,-0.381078720623586,-0.92000541566125)) ;
#38969 = DIRECTION('ref_axis',(0.995806686138499,0.0350088288095576,0.0845187893148318)) ;
#38970 = DIRECTION('center_axis',(0.,0.,1.)) ;
#38971 = DIRECTION('ref_axis',(1.,0.,0.)) ;
#38972 = DIRECTION('center_axis',(-0.09148247833253,0.381078720623586,0.92000541566125)) ;
#38973 = DIRECTION('ref_axis',(0.995806686138499,0.0350088288095576,0.0845187893148318)) ;
#38974 = DIRECTION('center_axis',(0.0914824783325255,-0.920005415661251,-0.381078720623585)) ;
#38975 = DIRECTION('ref_axis',(0.995806686138499,0.0845187893148277,0.0350088288095557)) ;
#38976 = DIRECTION('center_axis',(0.0914824783325255,-0.920005415661251,-0.381078720623585)) ;
#38977 = DIRECTION('ref_axis',(0.995806686138499,0.0845187893148277,0.0350088288095557)) ;
#38978 = DIRECTION('center_axis',(0.,0.,1.)) ;
#38979 = DIRECTION('ref_axis',(1.,0.,0.)) ;
#38980 = DIRECTION('center_axis',(-0.0914824783325255,0.920005415661251,0.381078720623585)) ;
#38981 = DIRECTION('ref_axis',(0.995806686138499,0.0845187893148277,0.0350088288095557)) ;
#38982 = DIRECTION('center_axis',(0.0914824783325252,-0.920005415661246,0.381078720623595)) ;
#38983 = DIRECTION('ref_axis',(0.995806686138499,0.084518789314827,-0.0350088288095565)) ;
#38984 = DIRECTION('center_axis',(1.22464679914736E-16,-1.,0.)) ;
#38985 = DIRECTION('ref_axis',(-1.,-1.22464679914736E-16,0.)) ;
#38986 = DIRECTION('center_axis',(0.0914824783325252,-0.920005415661246,0.381078720623595)) ;
#38987 = DIRECTION('ref_axis',(0.995806686138499,0.084518789314827,-0.0350088288095565)) ;
#38988 = DIRECTION('center_axis',(0.0914824783325252,-0.920005415661246,0.381078720623595)) ;
#38989 = DIRECTION('ref_axis',(0.995806686138499,0.084518789314827,-0.0350088288095565)) ;
#38990 = DIRECTION('center_axis',(0.,0.,1.)) ;
#38991 = DIRECTION('ref_axis',(-0.0701393346692214,0.997537204184465,0.)) ;
#38992 = DIRECTION('center_axis',(-0.0914824783325252,0.920005415661246,-0.381078720623595)) ;
#38993 = DIRECTION('ref_axis',(0.995806686138499,0.084518789314827,-0.0350088288095565)) ;
#38994 = DIRECTION('center_axis',(0.0914824783325311,-0.381078720623588,0.920005415661249)) ;
#38995 = DIRECTION('ref_axis',(0.995806686138498,0.0350088288095581,-0.0845187893148327)) ;
#38996 = DIRECTION('center_axis',(0.0914824783325311,-0.381078720623588,0.920005415661249)) ;
#38997 = DIRECTION('ref_axis',(0.995806686138498,0.0350088288095581,-0.0845187893148327)) ;
#38998 = DIRECTION('center_axis',(0.,0.,1.)) ;
#38999 = DIRECTION('ref_axis',(1.,0.,0.)) ;
#39000 = DIRECTION('center_axis',(-0.0914824783325311,0.381078720623588,-0.920005415661249)) ;
#39001 = DIRECTION('ref_axis',(0.995806686138498,0.0350088288095581,-0.0845187893148327)) ;
#39002 = DIRECTION('center_axis',(0.0914824783325254,0.381078720623588,0.92000541566125)) ;
#39003 = DIRECTION('ref_axis',(0.995806686138499,-0.0350088288095559,-0.0845187893148274)) ;
#39004 = DIRECTION('center_axis',(0.0914824783325254,0.381078720623588,0.92000541566125)) ;
#39005 = DIRECTION('ref_axis',(0.995806686138499,-0.0350088288095559,-0.0845187893148274)) ;
#39006 = DIRECTION('center_axis',(0.,0.,1.)) ;
#39007 = DIRECTION('ref_axis',(1.,0.,0.)) ;
#39008 = DIRECTION('center_axis',(-0.0914824783325254,-0.381078720623588,
-0.92000541566125)) ;
#39009 = DIRECTION('ref_axis',(0.995806686138499,-0.0350088288095559,-0.0845187893148274)) ;
#39010 = DIRECTION('center_axis',(0.0914824783325313,0.92000541566125,0.381078720623585)) ;
#39011 = DIRECTION('ref_axis',(0.995806686138498,-0.084518789314833,-0.0350088288095579)) ;
#39012 = DIRECTION('center_axis',(0.0914824783325313,0.92000541566125,0.381078720623585)) ;
#39013 = DIRECTION('ref_axis',(0.995806686138498,-0.084518789314833,-0.0350088288095579)) ;
#39014 = DIRECTION('center_axis',(0.,0.,1.)) ;
#39015 = DIRECTION('ref_axis',(1.,0.,0.)) ;
#39016 = DIRECTION('center_axis',(-0.0914824783325313,-0.92000541566125,-0.381078720623585)) ;
#39017 = DIRECTION('ref_axis',(0.995806686138498,-0.084518789314833,-0.0350088288095579)) ;
#39018 = DIRECTION('center_axis',(0.091482478332525,0.920005415661252,-0.381078720623582)) ;
#39019 = DIRECTION('ref_axis',(0.995806686138499,-0.0845187893148272,0.0350088288095552)) ;
#39020 = DIRECTION('center_axis',(1.22464679914736E-16,-1.,0.)) ;
#39021 = DIRECTION('ref_axis',(-1.,-1.22464679914736E-16,0.)) ;
#39022 = DIRECTION('center_axis',(0.091482478332525,0.920005415661252,-0.381078720623582)) ;
#39023 = DIRECTION('ref_axis',(0.995806686138499,-0.0845187893148272,0.0350088288095552)) ;
#39024 = DIRECTION('center_axis',(0.091482478332525,0.920005415661252,-0.381078720623582)) ;
#39025 = DIRECTION('ref_axis',(0.995806686138499,-0.0845187893148272,0.0350088288095552)) ;
#39026 = DIRECTION('center_axis',(0.,0.,1.)) ;
#39027 = DIRECTION('ref_axis',(-0.0701393346692214,-0.997537204184465,0.)) ;
#39028 = DIRECTION('center_axis',(-0.091482478332525,-0.920005415661252,0.381078720623582)) ;
#39029 = DIRECTION('ref_axis',(0.995806686138499,-0.0845187893148272,0.0350088288095552)) ;
#39030 = DIRECTION('center_axis',(0.0914824783325255,0.381078720623585,-0.920005415661251)) ;
#39031 = DIRECTION('ref_axis',(0.995806686138499,-0.0350088288095557,0.0845187893148276)) ;
#39032 = DIRECTION('center_axis',(0.0914824783325255,0.381078720623585,-0.920005415661251)) ;
#39033 = DIRECTION('ref_axis',(0.995806686138499,-0.0350088288095557,0.0845187893148276)) ;
#39034 = DIRECTION('center_axis',(0.,0.,1.)) ;
#39035 = DIRECTION('ref_axis',(1.,0.,0.)) ;
#39036 = DIRECTION('center_axis',(-0.0914824783325255,-0.381078720623585,
0.920005415661251)) ;
#39037 = DIRECTION('ref_axis',(0.995806686138499,-0.0350088288095557,0.0845187893148276)) ;
#39038 = DIRECTION('center_axis',(0.09148247833253,-0.381078720623586,-0.92000541566125)) ;
#39039 = DIRECTION('ref_axis',(0.995806686138499,0.0350088288095575,0.0845187893148318)) ;
#39040 = DIRECTION('center_axis',(0.09148247833253,-0.381078720623586,-0.92000541566125)) ;
#39041 = DIRECTION('ref_axis',(0.995806686138499,0.0350088288095575,0.0845187893148318)) ;
#39042 = DIRECTION('center_axis',(0.,0.,1.)) ;
#39043 = DIRECTION('ref_axis',(1.,0.,0.)) ;
#39044 = DIRECTION('center_axis',(-0.09148247833253,0.381078720623586,0.92000541566125)) ;
#39045 = DIRECTION('ref_axis',(0.995806686138499,0.0350088288095575,0.0845187893148318)) ;
#39046 = DIRECTION('center_axis',(0.0914824783325255,-0.920005415661251,-0.381078720623585)) ;
#39047 = DIRECTION('ref_axis',(0.995806686138499,0.0845187893148277,0.0350088288095557)) ;
#39048 = DIRECTION('center_axis',(0.0914824783325255,-0.920005415661251,-0.381078720623585)) ;
#39049 = DIRECTION('ref_axis',(0.995806686138499,0.0845187893148277,0.0350088288095557)) ;
#39050 = DIRECTION('center_axis',(0.,0.,1.)) ;
#39051 = DIRECTION('ref_axis',(1.,0.,0.)) ;
#39052 = DIRECTION('center_axis',(-0.0914824783325255,0.920005415661251,0.381078720623585)) ;
#39053 = DIRECTION('ref_axis',(0.995806686138499,0.0845187893148277,0.0350088288095557)) ;
#39054 = DIRECTION('center_axis',(0.091482478332531,-0.920005415661246,0.381078720623595)) ;
#39055 = DIRECTION('ref_axis',(0.995806686138498,0.0845187893148323,-0.0350088288095587)) ;
#39056 = DIRECTION('center_axis',(1.22464679914736E-16,-1.,0.)) ;
#39057 = DIRECTION('ref_axis',(-1.,-1.22464679914736E-16,0.)) ;
#39058 = DIRECTION('center_axis',(0.091482478332531,-0.920005415661246,0.381078720623595)) ;
#39059 = DIRECTION('ref_axis',(0.995806686138498,0.0845187893148323,-0.0350088288095587)) ;
#39060 = DIRECTION('center_axis',(0.091482478332531,-0.920005415661246,0.381078720623595)) ;
#39061 = DIRECTION('ref_axis',(0.995806686138498,0.0845187893148323,-0.0350088288095587)) ;
#39062 = DIRECTION('center_axis',(0.,0.,1.)) ;
#39063 = DIRECTION('ref_axis',(-0.0701393346692214,0.997537204184465,0.)) ;
#39064 = DIRECTION('center_axis',(-0.091482478332531,0.920005415661246,-0.381078720623595)) ;
#39065 = DIRECTION('ref_axis',(0.995806686138498,0.0845187893148323,-0.0350088288095587)) ;
#39066 = DIRECTION('center_axis',(0.0914824783325254,-0.381078720623588,0.920005415661249)) ;
#39067 = DIRECTION('ref_axis',(0.995806686138499,0.0350088288095559,-0.0845187893148274)) ;
#39068 = DIRECTION('center_axis',(0.0914824783325254,-0.381078720623588,0.920005415661249)) ;
#39069 = DIRECTION('ref_axis',(0.995806686138499,0.0350088288095559,-0.0845187893148274)) ;
#39070 = DIRECTION('center_axis',(0.,0.,1.)) ;
#39071 = DIRECTION('ref_axis',(1.,0.,0.)) ;
#39072 = DIRECTION('center_axis',(-0.0914824783325254,0.381078720623588,-0.920005415661249)) ;
#39073 = DIRECTION('ref_axis',(0.995806686138499,0.0350088288095559,-0.0845187893148274)) ;
#39074 = DIRECTION('center_axis',(0.0914824783325254,0.381078720623587,0.92000541566125)) ;
#39075 = DIRECTION('ref_axis',(0.995806686138499,-0.0350088288095559,-0.0845187893148275)) ;
#39076 = DIRECTION('center_axis',(0.0914824783325254,0.381078720623587,0.92000541566125)) ;
#39077 = DIRECTION('ref_axis',(0.995806686138499,-0.0350088288095559,-0.0845187893148275)) ;
#39078 = DIRECTION('center_axis',(0.,0.,1.)) ;
#39079 = DIRECTION('ref_axis',(1.,0.,0.)) ;
#39080 = DIRECTION('center_axis',(-0.0914824783325254,-0.381078720623587,
-0.92000541566125)) ;
#39081 = DIRECTION('ref_axis',(0.995806686138499,-0.0350088288095559,-0.0845187893148275)) ;
#39082 = DIRECTION('center_axis',(0.0914824783325306,0.920005415661252,0.381078720623582)) ;
#39083 = DIRECTION('ref_axis',(0.995806686138498,-0.0845187893148324,-0.0350088288095574)) ;
#39084 = DIRECTION('center_axis',(0.0914824783325306,0.920005415661252,0.381078720623582)) ;
#39085 = DIRECTION('ref_axis',(0.995806686138498,-0.0845187893148324,-0.0350088288095574)) ;
#39086 = DIRECTION('center_axis',(0.,0.,1.)) ;
#39087 = DIRECTION('ref_axis',(1.,0.,0.)) ;
#39088 = DIRECTION('center_axis',(-0.0914824783325306,-0.920005415661252,
-0.381078720623582)) ;
#39089 = DIRECTION('ref_axis',(0.995806686138498,-0.0845187893148324,-0.0350088288095574)) ;
#39090 = DIRECTION('center_axis',(0.0914824783325257,0.92000541566125,-0.381078720623585)) ;
#39091 = DIRECTION('ref_axis',(0.995806686138499,-0.0845187893148278,0.0350088288095558)) ;
#39092 = DIRECTION('center_axis',(1.22464679914737E-16,-1.,0.)) ;
#39093 = DIRECTION('ref_axis',(-1.,-1.22464679914737E-16,0.)) ;
#39094 = DIRECTION('center_axis',(0.0914824783325257,0.92000541566125,-0.381078720623585)) ;
#39095 = DIRECTION('ref_axis',(0.995806686138499,-0.0845187893148278,0.0350088288095558)) ;
#39096 = DIRECTION('center_axis',(0.0914824783325257,0.92000541566125,-0.381078720623585)) ;
#39097 = DIRECTION('ref_axis',(0.995806686138499,-0.0845187893148278,0.0350088288095558)) ;
#39098 = DIRECTION('center_axis',(0.,0.,1.)) ;
#39099 = DIRECTION('ref_axis',(-0.0701393346692214,-0.997537204184465,0.)) ;
#39100 = DIRECTION('center_axis',(-0.0914824783325257,-0.92000541566125,0.381078720623585)) ;
#39101 = DIRECTION('ref_axis',(0.995806686138499,-0.0845187893148278,0.0350088288095558)) ;
#39102 = DIRECTION('center_axis',(0.0914824783325312,0.381078720623585,-0.92000541566125)) ;
#39103 = DIRECTION('ref_axis',(0.995806686138498,-0.0350088288095579,0.0845187893148329)) ;
#39104 = DIRECTION('center_axis',(0.0914824783325312,0.381078720623585,-0.92000541566125)) ;
#39105 = DIRECTION('ref_axis',(0.995806686138498,-0.0350088288095579,0.0845187893148329)) ;
#39106 = DIRECTION('center_axis',(0.,0.,1.)) ;
#39107 = DIRECTION('ref_axis',(1.,0.,0.)) ;
#39108 = DIRECTION('center_axis',(-0.0914824783325312,-0.381078720623585,
0.92000541566125)) ;
#39109 = DIRECTION('ref_axis',(0.995806686138498,-0.0350088288095579,0.0845187893148329)) ;
#39110 = DIRECTION('center_axis',(0.0914824783325243,-0.381078720623586,-0.92000541566125)) ;
#39111 = DIRECTION('ref_axis',(0.995806686138499,0.0350088288095553,0.0845187893148265)) ;
#39112 = DIRECTION('center_axis',(0.0914824783325243,-0.381078720623586,-0.92000541566125)) ;
#39113 = DIRECTION('ref_axis',(0.995806686138499,0.0350088288095553,0.0845187893148265)) ;
#39114 = DIRECTION('center_axis',(0.,0.,1.)) ;
#39115 = DIRECTION('ref_axis',(1.,0.,0.)) ;
#39116 = DIRECTION('center_axis',(-0.0914824783325243,0.381078720623586,0.92000541566125)) ;
#39117 = DIRECTION('ref_axis',(0.995806686138499,0.0350088288095553,0.0845187893148265)) ;
#39118 = DIRECTION('center_axis',(0.0914824783325255,-0.920005415661251,-0.381078720623585)) ;
#39119 = DIRECTION('ref_axis',(0.995806686138499,0.0845187893148277,0.0350088288095557)) ;
#39120 = DIRECTION('center_axis',(0.0914824783325255,-0.920005415661251,-0.381078720623585)) ;
#39121 = DIRECTION('ref_axis',(0.995806686138499,0.0845187893148277,0.0350088288095557)) ;
#39122 = DIRECTION('center_axis',(0.,0.,1.)) ;
#39123 = DIRECTION('ref_axis',(1.,0.,0.)) ;
#39124 = DIRECTION('center_axis',(-0.0914824783325255,0.920005415661251,0.381078720623585)) ;
#39125 = DIRECTION('ref_axis',(0.995806686138499,0.0845187893148277,0.0350088288095557)) ;
#39126 = DIRECTION('center_axis',(0.0914824783325307,-0.920005415661247,0.381078720623594)) ;
#39127 = DIRECTION('ref_axis',(0.995806686138498,0.0845187893148321,-0.0350088288095585)) ;
#39128 = DIRECTION('center_axis',(1.22464679914736E-16,-1.,0.)) ;
#39129 = DIRECTION('ref_axis',(-1.,-1.22464679914736E-16,0.)) ;
#39130 = DIRECTION('center_axis',(0.0914824783325307,-0.920005415661247,0.381078720623594)) ;
#39131 = DIRECTION('ref_axis',(0.995806686138498,0.0845187893148321,-0.0350088288095585)) ;
#39132 = DIRECTION('center_axis',(0.0914824783325307,-0.920005415661247,0.381078720623594)) ;
#39133 = DIRECTION('ref_axis',(0.995806686138498,0.0845187893148321,-0.0350088288095585)) ;
#39134 = DIRECTION('center_axis',(0.,0.,1.)) ;
#39135 = DIRECTION('ref_axis',(-0.0701393346692214,0.997537204184465,0.)) ;
#39136 = DIRECTION('center_axis',(-0.0914824783325307,0.920005415661247,-0.381078720623594)) ;
#39137 = DIRECTION('ref_axis',(0.995806686138498,0.0845187893148321,-0.0350088288095585)) ;
#39138 = DIRECTION('center_axis',(0.0914824783325255,-0.381078720623585,0.920005415661251)) ;
#39139 = DIRECTION('ref_axis',(0.995806686138499,0.0350088288095557,-0.0845187893148276)) ;
#39140 = DIRECTION('center_axis',(0.0914824783325255,-0.381078720623585,0.920005415661251)) ;
#39141 = DIRECTION('ref_axis',(0.995806686138499,0.0350088288095557,-0.0845187893148276)) ;
#39142 = DIRECTION('center_axis',(0.,0.,1.)) ;
#39143 = DIRECTION('ref_axis',(1.,0.,0.)) ;
#39144 = DIRECTION('center_axis',(-0.0914824783325255,0.381078720623585,-0.920005415661251)) ;
#39145 = DIRECTION('ref_axis',(0.995806686138499,0.0350088288095557,-0.0845187893148276)) ;
#39146 = DIRECTION('center_axis',(0.0914824783325311,0.381078720623587,0.920005415661249)) ;
#39147 = DIRECTION('ref_axis',(0.995806686138498,-0.035008828809558,-0.0845187893148328)) ;
#39148 = DIRECTION('center_axis',(0.0914824783325311,0.381078720623587,0.920005415661249)) ;
#39149 = DIRECTION('ref_axis',(0.995806686138498,-0.035008828809558,-0.0845187893148328)) ;
#39150 = DIRECTION('center_axis',(0.,0.,1.)) ;
#39151 = DIRECTION('ref_axis',(1.,0.,0.)) ;
#39152 = DIRECTION('center_axis',(-0.0914824783325311,-0.381078720623587,
-0.920005415661249)) ;
#39153 = DIRECTION('ref_axis',(0.995806686138498,-0.035008828809558,-0.0845187893148328)) ;
#39154 = DIRECTION('center_axis',(0.0914824783325253,0.920005415661251,0.381078720623584)) ;
#39155 = DIRECTION('ref_axis',(0.995806686138499,-0.0845187893148275,-0.0350088288095555)) ;
#39156 = DIRECTION('center_axis',(0.0914824783325253,0.920005415661251,0.381078720623584)) ;
#39157 = DIRECTION('ref_axis',(0.995806686138499,-0.0845187893148275,-0.0350088288095555)) ;
#39158 = DIRECTION('center_axis',(0.,0.,1.)) ;
#39159 = DIRECTION('ref_axis',(1.,0.,0.)) ;
#39160 = DIRECTION('center_axis',(-0.0914824783325253,-0.920005415661251,
-0.381078720623584)) ;
#39161 = DIRECTION('ref_axis',(0.995806686138499,-0.0845187893148275,-0.0350088288095555)) ;
#39162 = DIRECTION('center_axis',(0.0914824783325253,0.920005415661251,-0.381078720623584)) ;
#39163 = DIRECTION('ref_axis',(0.995806686138499,-0.0845187893148275,0.0350088288095555)) ;
#39164 = DIRECTION('center_axis',(1.22464679914736E-16,-1.,0.)) ;
#39165 = DIRECTION('ref_axis',(-1.,-1.22464679914736E-16,0.)) ;
#39166 = DIRECTION('center_axis',(0.0914824783325253,0.920005415661251,-0.381078720623584)) ;
#39167 = DIRECTION('ref_axis',(0.995806686138499,-0.0845187893148275,0.0350088288095555)) ;
#39168 = DIRECTION('center_axis',(0.0914824783325253,0.920005415661251,-0.381078720623584)) ;
#39169 = DIRECTION('ref_axis',(0.995806686138499,-0.0845187893148275,0.0350088288095555)) ;
#39170 = DIRECTION('center_axis',(0.,0.,1.)) ;
#39171 = DIRECTION('ref_axis',(-0.0701393346692214,-0.997537204184465,0.)) ;
#39172 = DIRECTION('center_axis',(-0.0914824783325253,-0.920005415661251,
0.381078720623584)) ;
#39173 = DIRECTION('ref_axis',(0.995806686138499,-0.0845187893148275,0.0350088288095555)) ;
#39174 = DIRECTION('center_axis',(0.0914824783325312,0.381078720623585,-0.92000541566125)) ;
#39175 = DIRECTION('ref_axis',(0.995806686138498,-0.0350088288095579,0.0845187893148329)) ;
#39176 = DIRECTION('center_axis',(0.0914824783325312,0.381078720623585,-0.92000541566125)) ;
#39177 = DIRECTION('ref_axis',(0.995806686138498,-0.0350088288095579,0.0845187893148329)) ;
#39178 = DIRECTION('center_axis',(0.,0.,1.)) ;
#39179 = DIRECTION('ref_axis',(1.,0.,0.)) ;
#39180 = DIRECTION('center_axis',(-0.0914824783325312,-0.381078720623585,
0.92000541566125)) ;
#39181 = DIRECTION('ref_axis',(0.995806686138498,-0.0350088288095579,0.0845187893148329)) ;
#39182 = DIRECTION('center_axis',(0.0914824783325254,-0.381078720623587,-0.92000541566125)) ;
#39183 = DIRECTION('ref_axis',(0.995806686138499,0.0350088288095559,0.0845187893148275)) ;
#39184 = DIRECTION('center_axis',(0.0914824783325254,-0.381078720623587,-0.92000541566125)) ;
#39185 = DIRECTION('ref_axis',(0.995806686138499,0.0350088288095559,0.0845187893148275)) ;
#39186 = DIRECTION('center_axis',(0.,0.,1.)) ;
#39187 = DIRECTION('ref_axis',(1.,0.,0.)) ;
#39188 = DIRECTION('center_axis',(-0.0914824783325254,0.381078720623587,0.92000541566125)) ;
#39189 = DIRECTION('ref_axis',(0.995806686138499,0.0350088288095559,0.0845187893148275)) ;
#39190 = DIRECTION('center_axis',(0.0914824783325306,-0.920005415661247,-0.381078720623593)) ;
#39191 = DIRECTION('ref_axis',(0.995806686138498,0.084518789314832,0.0350088288095584)) ;
#39192 = DIRECTION('center_axis',(0.0914824783325306,-0.920005415661247,-0.381078720623593)) ;
#39193 = DIRECTION('ref_axis',(0.995806686138498,0.084518789314832,0.0350088288095584)) ;
#39194 = DIRECTION('center_axis',(0.,0.,1.)) ;
#39195 = DIRECTION('ref_axis',(1.,0.,0.)) ;
#39196 = DIRECTION('center_axis',(-0.0914824783325306,0.920005415661247,0.381078720623593)) ;
#39197 = DIRECTION('ref_axis',(0.995806686138498,0.084518789314832,0.0350088288095584)) ;
#39198 = DIRECTION('center_axis',(0.0914824783325249,-0.920005415661247,0.381078720623594)) ;
#39199 = DIRECTION('ref_axis',(0.995806686138499,0.0845187893148268,-0.0350088288095563)) ;
#39200 = DIRECTION('center_axis',(1.22464679914737E-16,-1.,0.)) ;
#39201 = DIRECTION('ref_axis',(-1.,-1.22464679914737E-16,0.)) ;
#39202 = DIRECTION('center_axis',(0.0914824783325249,-0.920005415661247,0.381078720623594)) ;
#39203 = DIRECTION('ref_axis',(0.995806686138499,0.0845187893148268,-0.0350088288095563)) ;
#39204 = DIRECTION('center_axis',(0.0914824783325249,-0.920005415661247,0.381078720623594)) ;
#39205 = DIRECTION('ref_axis',(0.995806686138499,0.0845187893148268,-0.0350088288095563)) ;
#39206 = DIRECTION('center_axis',(0.,0.,1.)) ;
#39207 = DIRECTION('ref_axis',(-0.0701393346692214,0.997537204184465,0.)) ;
#39208 = DIRECTION('center_axis',(-0.0914824783325249,0.920005415661247,-0.381078720623594)) ;
#39209 = DIRECTION('ref_axis',(0.995806686138499,0.0845187893148268,-0.0350088288095563)) ;
#39210 = DIRECTION('center_axis',(0.0914824783325255,-0.381078720623586,0.92000541566125)) ;
#39211 = DIRECTION('ref_axis',(0.995806686138499,0.0350088288095557,-0.0845187893148276)) ;
#39212 = DIRECTION('center_axis',(0.0914824783325255,-0.381078720623586,0.92000541566125)) ;
#39213 = DIRECTION('ref_axis',(0.995806686138499,0.0350088288095557,-0.0845187893148276)) ;
#39214 = DIRECTION('center_axis',(0.,0.,1.)) ;
#39215 = DIRECTION('ref_axis',(1.,0.,0.)) ;
#39216 = DIRECTION('center_axis',(-0.0914824783325255,0.381078720623586,-0.92000541566125)) ;
#39217 = DIRECTION('ref_axis',(0.995806686138499,0.0350088288095557,-0.0845187893148276)) ;
#39218 = DIRECTION('center_axis',(0.0914824783325311,0.381078720623587,0.920005415661249)) ;
#39219 = DIRECTION('ref_axis',(0.995806686138498,-0.035008828809558,-0.0845187893148328)) ;
#39220 = DIRECTION('center_axis',(0.0914824783325311,0.381078720623587,0.920005415661249)) ;
#39221 = DIRECTION('ref_axis',(0.995806686138498,-0.035008828809558,-0.0845187893148328)) ;
#39222 = DIRECTION('center_axis',(0.,0.,1.)) ;
#39223 = DIRECTION('ref_axis',(1.,0.,0.)) ;
#39224 = DIRECTION('center_axis',(-0.0914824783325311,-0.381078720623587,
-0.920005415661249)) ;
#39225 = DIRECTION('ref_axis',(0.995806686138498,-0.035008828809558,-0.0845187893148328)) ;
#39226 = DIRECTION('center_axis',(0.0914824783325253,0.920005415661251,0.381078720623584)) ;
#39227 = DIRECTION('ref_axis',(0.995806686138499,-0.0845187893148275,-0.0350088288095555)) ;
#39228 = DIRECTION('center_axis',(0.0914824783325253,0.920005415661251,0.381078720623584)) ;
#39229 = DIRECTION('ref_axis',(0.995806686138499,-0.0845187893148275,-0.0350088288095555)) ;
#39230 = DIRECTION('center_axis',(0.,0.,1.)) ;
#39231 = DIRECTION('ref_axis',(1.,0.,0.)) ;
#39232 = DIRECTION('center_axis',(-0.0914824783325253,-0.920005415661251,
-0.381078720623584)) ;
#39233 = DIRECTION('ref_axis',(0.995806686138499,-0.0845187893148275,-0.0350088288095555)) ;
#39234 = DIRECTION('center_axis',(0.0914824783325311,0.920005415661251,-0.381078720623584)) ;
#39235 = DIRECTION('ref_axis',(0.995806686138498,-0.0845187893148328,0.0350088288095577)) ;
#39236 = DIRECTION('center_axis',(1.22464679914737E-16,-1.,0.)) ;
#39237 = DIRECTION('ref_axis',(-1.,-1.22464679914737E-16,0.)) ;
#39238 = DIRECTION('center_axis',(0.0914824783325311,0.920005415661251,-0.381078720623584)) ;
#39239 = DIRECTION('ref_axis',(0.995806686138498,-0.0845187893148328,0.0350088288095577)) ;
#39240 = DIRECTION('center_axis',(0.0914824783325311,0.920005415661251,-0.381078720623584)) ;
#39241 = DIRECTION('ref_axis',(0.995806686138498,-0.0845187893148328,0.0350088288095577)) ;
#39242 = DIRECTION('center_axis',(0.,0.,1.)) ;
#39243 = DIRECTION('ref_axis',(-0.0701393346692214,-0.997537204184465,0.)) ;
#39244 = DIRECTION('center_axis',(-0.0914824783325311,-0.920005415661251,
0.381078720623584)) ;
#39245 = DIRECTION('ref_axis',(0.995806686138498,-0.0845187893148328,0.0350088288095577)) ;
#39246 = DIRECTION('center_axis',(0.0914824783325255,0.381078720623586,-0.92000541566125)) ;
#39247 = DIRECTION('ref_axis',(0.995806686138499,-0.0350088288095557,0.0845187893148276)) ;
#39248 = DIRECTION('center_axis',(0.0914824783325255,0.381078720623586,-0.92000541566125)) ;
#39249 = DIRECTION('ref_axis',(0.995806686138499,-0.0350088288095557,0.0845187893148276)) ;
#39250 = DIRECTION('center_axis',(0.,0.,1.)) ;
#39251 = DIRECTION('ref_axis',(1.,0.,0.)) ;
#39252 = DIRECTION('center_axis',(-0.0914824783325255,-0.381078720623586,
0.92000541566125)) ;
#39253 = DIRECTION('ref_axis',(0.995806686138499,-0.0350088288095557,0.0845187893148276)) ;
#39254 = DIRECTION('center_axis',(0.0914824783325254,-0.381078720623587,-0.92000541566125)) ;
#39255 = DIRECTION('ref_axis',(0.995806686138499,0.0350088288095558,0.0845187893148275)) ;
#39256 = DIRECTION('center_axis',(0.0914824783325254,-0.381078720623587,-0.92000541566125)) ;
#39257 = DIRECTION('ref_axis',(0.995806686138499,0.0350088288095558,0.0845187893148275)) ;
#39258 = DIRECTION('center_axis',(0.,0.,1.)) ;
#39259 = DIRECTION('ref_axis',(1.,0.,0.)) ;
#39260 = DIRECTION('center_axis',(-0.0914824783325254,0.381078720623587,0.92000541566125)) ;
#39261 = DIRECTION('ref_axis',(0.995806686138499,0.0350088288095558,0.0845187893148275)) ;
#39262 = DIRECTION('center_axis',(0.0914824783325306,-0.920005415661247,-0.381078720623593)) ;
#39263 = DIRECTION('ref_axis',(0.995806686138498,0.084518789314832,0.0350088288095584)) ;
#39264 = DIRECTION('center_axis',(0.0914824783325306,-0.920005415661247,-0.381078720623593)) ;
#39265 = DIRECTION('ref_axis',(0.995806686138498,0.084518789314832,0.0350088288095584)) ;
#39266 = DIRECTION('center_axis',(0.,0.,1.)) ;
#39267 = DIRECTION('ref_axis',(1.,0.,0.)) ;
#39268 = DIRECTION('center_axis',(-0.0914824783325306,0.920005415661247,0.381078720623593)) ;
#39269 = DIRECTION('ref_axis',(0.995806686138498,0.084518789314832,0.0350088288095584)) ;
#39270 = DIRECTION('center_axis',(0.0914824783325249,-0.920005415661247,0.381078720623594)) ;
#39271 = DIRECTION('ref_axis',(0.995806686138499,0.0845187893148267,-0.0350088288095562)) ;
#39272 = DIRECTION('center_axis',(1.22464679914737E-16,-1.,0.)) ;
#39273 = DIRECTION('ref_axis',(-1.,-1.22464679914737E-16,0.)) ;
#39274 = DIRECTION('center_axis',(0.0914824783325249,-0.920005415661247,0.381078720623594)) ;
#39275 = DIRECTION('ref_axis',(0.995806686138499,0.0845187893148267,-0.0350088288095562)) ;
#39276 = DIRECTION('center_axis',(0.0914824783325249,-0.920005415661247,0.381078720623594)) ;
#39277 = DIRECTION('ref_axis',(0.995806686138499,0.0845187893148267,-0.0350088288095562)) ;
#39278 = DIRECTION('center_axis',(0.,0.,1.)) ;
#39279 = DIRECTION('ref_axis',(-0.0701393346692214,0.997537204184465,0.)) ;
#39280 = DIRECTION('center_axis',(-0.0914824783325249,0.920005415661247,-0.381078720623594)) ;
#39281 = DIRECTION('ref_axis',(0.995806686138499,0.0845187893148267,-0.0350088288095562)) ;
#39282 = DIRECTION('center_axis',(0.0914824783325312,-0.381078720623586,0.92000541566125)) ;
#39283 = DIRECTION('ref_axis',(0.995806686138498,0.0350088288095579,-0.0845187893148329)) ;
#39284 = DIRECTION('center_axis',(0.0914824783325312,-0.381078720623586,0.92000541566125)) ;
#39285 = DIRECTION('ref_axis',(0.995806686138498,0.0350088288095579,-0.0845187893148329)) ;
#39286 = DIRECTION('center_axis',(0.,0.,1.)) ;
#39287 = DIRECTION('ref_axis',(1.,0.,0.)) ;
#39288 = DIRECTION('center_axis',(-0.0914824783325312,0.381078720623586,-0.92000541566125)) ;
#39289 = DIRECTION('ref_axis',(0.995806686138498,0.0350088288095579,-0.0845187893148329)) ;
#39290 = DIRECTION('center_axis',(0.0914824783325254,0.381078720623587,0.92000541566125)) ;
#39291 = DIRECTION('ref_axis',(0.995806686138499,-0.0350088288095558,-0.0845187893148275)) ;
#39292 = DIRECTION('center_axis',(0.0914824783325254,0.381078720623587,0.92000541566125)) ;
#39293 = DIRECTION('ref_axis',(0.995806686138499,-0.0350088288095558,-0.0845187893148275)) ;
#39294 = DIRECTION('center_axis',(0.,0.,1.)) ;
#39295 = DIRECTION('ref_axis',(1.,0.,0.)) ;
#39296 = DIRECTION('center_axis',(-0.0914824783325254,-0.381078720623587,
-0.92000541566125)) ;
#39297 = DIRECTION('ref_axis',(0.995806686138499,-0.0350088288095558,-0.0845187893148275)) ;
#39298 = DIRECTION('center_axis',(0.0914824783325253,0.920005415661251,0.381078720623584)) ;
#39299 = DIRECTION('ref_axis',(0.995806686138499,-0.0845187893148275,-0.0350088288095555)) ;
#39300 = DIRECTION('center_axis',(0.0914824783325253,0.920005415661251,0.381078720623584)) ;
#39301 = DIRECTION('ref_axis',(0.995806686138499,-0.0845187893148275,-0.0350088288095555)) ;
#39302 = DIRECTION('center_axis',(0.,0.,1.)) ;
#39303 = DIRECTION('ref_axis',(1.,0.,0.)) ;
#39304 = DIRECTION('center_axis',(-0.0914824783325253,-0.920005415661251,
-0.381078720623584)) ;
#39305 = DIRECTION('ref_axis',(0.995806686138499,-0.0845187893148275,-0.0350088288095555)) ;
#39306 = DIRECTION('center_axis',(0.091482478332531,0.920005415661251,-0.381078720623584)) ;
#39307 = DIRECTION('ref_axis',(0.995806686138498,-0.0845187893148328,0.0350088288095577)) ;
#39308 = DIRECTION('center_axis',(1.22464679914737E-16,-1.,0.)) ;
#39309 = DIRECTION('ref_axis',(-1.,-1.22464679914737E-16,0.)) ;
#39310 = DIRECTION('center_axis',(0.091482478332531,0.920005415661251,-0.381078720623584)) ;
#39311 = DIRECTION('ref_axis',(0.995806686138498,-0.0845187893148328,0.0350088288095577)) ;
#39312 = DIRECTION('center_axis',(0.091482478332531,0.920005415661251,-0.381078720623584)) ;
#39313 = DIRECTION('ref_axis',(0.995806686138498,-0.0845187893148328,0.0350088288095577)) ;
#39314 = DIRECTION('center_axis',(0.,0.,1.)) ;
#39315 = DIRECTION('ref_axis',(-0.0701393346692214,-0.997537204184465,0.)) ;
#39316 = DIRECTION('center_axis',(-0.091482478332531,-0.920005415661251,0.381078720623584)) ;
#39317 = DIRECTION('ref_axis',(0.995806686138498,-0.0845187893148328,0.0350088288095577)) ;
#39318 = DIRECTION('center_axis',(0.0914824783325255,0.381078720623586,-0.92000541566125)) ;
#39319 = DIRECTION('ref_axis',(0.995806686138499,-0.0350088288095557,0.0845187893148276)) ;
#39320 = DIRECTION('center_axis',(0.0914824783325255,0.381078720623586,-0.92000541566125)) ;
#39321 = DIRECTION('ref_axis',(0.995806686138499,-0.0350088288095557,0.0845187893148276)) ;
#39322 = DIRECTION('center_axis',(0.,0.,1.)) ;
#39323 = DIRECTION('ref_axis',(1.,0.,0.)) ;
#39324 = DIRECTION('center_axis',(-0.0914824783325255,-0.381078720623586,
0.92000541566125)) ;
#39325 = DIRECTION('ref_axis',(0.995806686138499,-0.0350088288095557,0.0845187893148276)) ;
#39326 = DIRECTION('center_axis',(0.0914824783325311,-0.381078720623587,-0.920005415661249)) ;
#39327 = DIRECTION('ref_axis',(0.995806686138498,0.035008828809558,0.0845187893148328)) ;
#39328 = DIRECTION('center_axis',(0.0914824783325311,-0.381078720623587,-0.920005415661249)) ;
#39329 = DIRECTION('ref_axis',(0.995806686138498,0.035008828809558,0.0845187893148328)) ;
#39330 = DIRECTION('center_axis',(0.,0.,1.)) ;
#39331 = DIRECTION('ref_axis',(1.,0.,0.)) ;
#39332 = DIRECTION('center_axis',(-0.0914824783325311,0.381078720623587,0.920005415661249)) ;
#39333 = DIRECTION('ref_axis',(0.995806686138498,0.035008828809558,0.0845187893148328)) ;
#39334 = DIRECTION('center_axis',(0.0914824783325249,-0.920005415661247,-0.381078720623594)) ;
#39335 = DIRECTION('ref_axis',(0.995806686138499,0.0845187893148267,0.0350088288095562)) ;
#39336 = DIRECTION('center_axis',(0.0914824783325249,-0.920005415661247,-0.381078720623594)) ;
#39337 = DIRECTION('ref_axis',(0.995806686138499,0.0845187893148267,0.0350088288095562)) ;
#39338 = DIRECTION('center_axis',(0.,0.,1.)) ;
#39339 = DIRECTION('ref_axis',(1.,0.,0.)) ;
#39340 = DIRECTION('center_axis',(-0.0914824783325249,0.920005415661247,0.381078720623594)) ;
#39341 = DIRECTION('ref_axis',(0.995806686138499,0.0845187893148267,0.0350088288095562)) ;
#39342 = DIRECTION('center_axis',(0.0914824783325249,-0.920005415661247,0.381078720623594)) ;
#39343 = DIRECTION('ref_axis',(0.995806686138499,0.0845187893148268,-0.0350088288095563)) ;
#39344 = DIRECTION('center_axis',(1.22464679914736E-16,-1.,0.)) ;
#39345 = DIRECTION('ref_axis',(-1.,-1.22464679914736E-16,0.)) ;
#39346 = DIRECTION('center_axis',(0.0914824783325249,-0.920005415661247,0.381078720623594)) ;
#39347 = DIRECTION('ref_axis',(0.995806686138499,0.0845187893148268,-0.0350088288095563)) ;
#39348 = DIRECTION('center_axis',(0.0914824783325249,-0.920005415661247,0.381078720623594)) ;
#39349 = DIRECTION('ref_axis',(0.995806686138499,0.0845187893148268,-0.0350088288095563)) ;
#39350 = DIRECTION('center_axis',(0.,0.,1.)) ;
#39351 = DIRECTION('ref_axis',(-0.0701393346691978,0.997537204184467,0.)) ;
#39352 = DIRECTION('center_axis',(-0.0914824783325249,0.920005415661247,-0.381078720623594)) ;
#39353 = DIRECTION('ref_axis',(0.995806686138499,0.0845187893148268,-0.0350088288095563)) ;
#39354 = DIRECTION('center_axis',(0.0914824783325312,-0.381078720623586,0.92000541566125)) ;
#39355 = DIRECTION('ref_axis',(0.995806686138498,0.035008828809558,-0.0845187893148329)) ;
#39356 = DIRECTION('center_axis',(0.0914824783325312,-0.381078720623586,0.92000541566125)) ;
#39357 = DIRECTION('ref_axis',(0.995806686138498,0.035008828809558,-0.0845187893148329)) ;
#39358 = DIRECTION('center_axis',(0.,0.,1.)) ;
#39359 = DIRECTION('ref_axis',(1.,0.,0.)) ;
#39360 = DIRECTION('center_axis',(-0.0914824783325312,0.381078720623586,-0.92000541566125)) ;
#39361 = DIRECTION('ref_axis',(0.995806686138498,0.035008828809558,-0.0845187893148329)) ;
#39362 = DIRECTION('center_axis',(0.0914824783325254,0.381078720623587,0.92000541566125)) ;
#39363 = DIRECTION('ref_axis',(0.995806686138499,-0.0350088288095558,-0.0845187893148275)) ;
#39364 = DIRECTION('center_axis',(0.0914824783325254,0.381078720623587,0.92000541566125)) ;
#39365 = DIRECTION('ref_axis',(0.995806686138499,-0.0350088288095558,-0.0845187893148275)) ;
#39366 = DIRECTION('center_axis',(0.,0.,1.)) ;
#39367 = DIRECTION('ref_axis',(1.,0.,0.)) ;
#39368 = DIRECTION('center_axis',(-0.0914824783325254,-0.381078720623587,
-0.92000541566125)) ;
#39369 = DIRECTION('ref_axis',(0.995806686138499,-0.0350088288095558,-0.0845187893148275)) ;
#39370 = DIRECTION('center_axis',(0.091482478332531,0.920005415661251,0.381078720623584)) ;
#39371 = DIRECTION('ref_axis',(0.995806686138498,-0.0845187893148328,-0.0350088288095577)) ;
#39372 = DIRECTION('center_axis',(0.091482478332531,0.920005415661251,0.381078720623584)) ;
#39373 = DIRECTION('ref_axis',(0.995806686138498,-0.0845187893148328,-0.0350088288095577)) ;
#39374 = DIRECTION('center_axis',(0.,0.,1.)) ;
#39375 = DIRECTION('ref_axis',(1.,0.,0.)) ;
#39376 = DIRECTION('center_axis',(-0.091482478332531,-0.920005415661251,-0.381078720623584)) ;
#39377 = DIRECTION('ref_axis',(0.995806686138498,-0.0845187893148328,-0.0350088288095577)) ;
#39378 = DIRECTION('center_axis',(0.0914824783325253,0.920005415661251,-0.381078720623584)) ;
#39379 = DIRECTION('ref_axis',(0.995806686138499,-0.0845187893148275,0.0350088288095555)) ;
#39380 = DIRECTION('center_axis',(1.22464679914736E-16,-1.,0.)) ;
#39381 = DIRECTION('ref_axis',(-1.,-1.22464679914736E-16,0.)) ;
#39382 = DIRECTION('center_axis',(0.0914824783325253,0.920005415661251,-0.381078720623584)) ;
#39383 = DIRECTION('ref_axis',(0.995806686138499,-0.0845187893148275,0.0350088288095555)) ;
#39384 = DIRECTION('center_axis',(0.0914824783325253,0.920005415661251,-0.381078720623584)) ;
#39385 = DIRECTION('ref_axis',(0.995806686138499,-0.0845187893148275,0.0350088288095555)) ;
#39386 = DIRECTION('center_axis',(0.,0.,1.)) ;
#39387 = DIRECTION('ref_axis',(-0.0701393346692214,-0.997537204184465,0.)) ;
#39388 = DIRECTION('center_axis',(-0.0914824783325253,-0.920005415661251,
0.381078720623584)) ;
#39389 = DIRECTION('ref_axis',(0.995806686138499,-0.0845187893148275,0.0350088288095555)) ;
#39390 = DIRECTION('center_axis',(0.0914824783325255,0.381078720623586,-0.92000541566125)) ;
#39391 = DIRECTION('ref_axis',(0.995806686138499,-0.0350088288095558,0.0845187893148276)) ;
#39392 = DIRECTION('center_axis',(0.0914824783325255,0.381078720623586,-0.92000541566125)) ;
#39393 = DIRECTION('ref_axis',(0.995806686138499,-0.0350088288095558,0.0845187893148276)) ;
#39394 = DIRECTION('center_axis',(0.,0.,1.)) ;
#39395 = DIRECTION('ref_axis',(1.,0.,0.)) ;
#39396 = DIRECTION('center_axis',(-0.0914824783325255,-0.381078720623586,
0.92000541566125)) ;
#39397 = DIRECTION('ref_axis',(0.995806686138499,-0.0350088288095558,0.0845187893148276)) ;
#39398 = DIRECTION('center_axis',(0.0914824783325311,-0.381078720623587,-0.920005415661249)) ;
#39399 = DIRECTION('ref_axis',(0.995806686138498,0.035008828809558,0.0845187893148328)) ;
#39400 = DIRECTION('center_axis',(0.0914824783325311,-0.381078720623587,-0.920005415661249)) ;
#39401 = DIRECTION('ref_axis',(0.995806686138498,0.035008828809558,0.0845187893148328)) ;
#39402 = DIRECTION('center_axis',(0.,0.,1.)) ;
#39403 = DIRECTION('ref_axis',(1.,0.,0.)) ;
#39404 = DIRECTION('center_axis',(-0.0914824783325311,0.381078720623587,0.920005415661249)) ;
#39405 = DIRECTION('ref_axis',(0.995806686138498,0.035008828809558,0.0845187893148328)) ;
#39406 = DIRECTION('center_axis',(0.091482478332525,-0.920005415661247,-0.381078720623594)) ;
#39407 = DIRECTION('ref_axis',(0.995806686138499,0.0845187893148268,0.0350088288095563)) ;
#39408 = DIRECTION('center_axis',(0.091482478332525,-0.920005415661247,-0.381078720623594)) ;
#39409 = DIRECTION('ref_axis',(0.995806686138499,0.0845187893148268,0.0350088288095563)) ;
#39410 = DIRECTION('center_axis',(0.,0.,1.)) ;
#39411 = DIRECTION('ref_axis',(1.,0.,0.)) ;
#39412 = DIRECTION('center_axis',(-0.091482478332525,0.920005415661247,0.381078720623594)) ;
#39413 = DIRECTION('ref_axis',(0.995806686138499,0.0845187893148268,0.0350088288095563)) ;
#39414 = DIRECTION('center_axis',(0.0914824783325307,-0.920005415661246,0.381078720623594)) ;
#39415 = DIRECTION('ref_axis',(0.995806686138498,0.0845187893148321,-0.0350088288095585)) ;
#39416 = DIRECTION('center_axis',(1.22464679914737E-16,-1.,0.)) ;
#39417 = DIRECTION('ref_axis',(-1.,-1.22464679914737E-16,0.)) ;
#39418 = DIRECTION('center_axis',(0.0914824783325307,-0.920005415661246,0.381078720623594)) ;
#39419 = DIRECTION('ref_axis',(0.995806686138498,0.0845187893148321,-0.0350088288095585)) ;
#39420 = DIRECTION('center_axis',(0.0914824783325307,-0.920005415661246,0.381078720623594)) ;
#39421 = DIRECTION('ref_axis',(0.995806686138498,0.0845187893148321,-0.0350088288095585)) ;
#39422 = DIRECTION('center_axis',(0.,0.,1.)) ;
#39423 = DIRECTION('ref_axis',(-0.0701393346692214,0.997537204184465,0.)) ;
#39424 = DIRECTION('center_axis',(-0.0914824783325307,0.920005415661246,-0.381078720623594)) ;
#39425 = DIRECTION('ref_axis',(0.995806686138498,0.0845187893148321,-0.0350088288095585)) ;
#39426 = DIRECTION('center_axis',(0.0914824783325254,-0.381078720623587,0.92000541566125)) ;
#39427 = DIRECTION('ref_axis',(0.995806686138499,0.0350088288095558,-0.0845187893148275)) ;
#39428 = DIRECTION('center_axis',(0.0914824783325254,-0.381078720623587,0.92000541566125)) ;
#39429 = DIRECTION('ref_axis',(0.995806686138499,0.0350088288095558,-0.0845187893148275)) ;
#39430 = DIRECTION('center_axis',(0.,0.,1.)) ;
#39431 = DIRECTION('ref_axis',(1.,0.,0.)) ;
#39432 = DIRECTION('center_axis',(-0.0914824783325254,0.381078720623587,-0.92000541566125)) ;
#39433 = DIRECTION('ref_axis',(0.995806686138499,0.0350088288095558,-0.0845187893148275)) ;
#39434 = DIRECTION('center_axis',(0.0914824783325254,0.381078720623587,0.92000541566125)) ;
#39435 = DIRECTION('ref_axis',(0.995806686138499,-0.0350088288095559,-0.0845187893148275)) ;
#39436 = DIRECTION('center_axis',(0.0914824783325254,0.381078720623587,0.92000541566125)) ;
#39437 = DIRECTION('ref_axis',(0.995806686138499,-0.0350088288095559,-0.0845187893148275)) ;
#39438 = DIRECTION('center_axis',(0.,0.,1.)) ;
#39439 = DIRECTION('ref_axis',(1.,0.,0.)) ;
#39440 = DIRECTION('center_axis',(-0.0914824783325254,-0.381078720623587,
-0.92000541566125)) ;
#39441 = DIRECTION('ref_axis',(0.995806686138499,-0.0350088288095559,-0.0845187893148275)) ;
#39442 = DIRECTION('center_axis',(0.0914824783325311,0.920005415661251,0.381078720623584)) ;
#39443 = DIRECTION('ref_axis',(0.995806686138498,-0.0845187893148328,-0.0350088288095577)) ;
#39444 = DIRECTION('center_axis',(0.0914824783325311,0.920005415661251,0.381078720623584)) ;
#39445 = DIRECTION('ref_axis',(0.995806686138498,-0.0845187893148328,-0.0350088288095577)) ;
#39446 = DIRECTION('center_axis',(0.,0.,1.)) ;
#39447 = DIRECTION('ref_axis',(1.,0.,0.)) ;
#39448 = DIRECTION('center_axis',(-0.0914824783325311,-0.920005415661251,
-0.381078720623584)) ;
#39449 = DIRECTION('ref_axis',(0.995806686138498,-0.0845187893148328,-0.0350088288095577)) ;
#39450 = DIRECTION('center_axis',(0.0914824783325254,0.920005415661251,-0.381078720623584)) ;
#39451 = DIRECTION('ref_axis',(0.995806686138499,-0.0845187893148275,0.0350088288095555)) ;
#39452 = DIRECTION('center_axis',(1.22464679914737E-16,-1.,0.)) ;
#39453 = DIRECTION('ref_axis',(-1.,-1.22464679914737E-16,0.)) ;
#39454 = DIRECTION('center_axis',(0.0914824783325254,0.920005415661251,-0.381078720623584)) ;
#39455 = DIRECTION('ref_axis',(0.995806686138499,-0.0845187893148275,0.0350088288095555)) ;
#39456 = DIRECTION('center_axis',(0.0914824783325254,0.920005415661251,-0.381078720623584)) ;
#39457 = DIRECTION('ref_axis',(0.995806686138499,-0.0845187893148275,0.0350088288095555)) ;
#39458 = DIRECTION('center_axis',(0.,0.,1.)) ;
#39459 = DIRECTION('ref_axis',(-0.0701393346692214,-0.997537204184465,0.)) ;
#39460 = DIRECTION('center_axis',(-0.0914824783325254,-0.920005415661251,
0.381078720623584)) ;
#39461 = DIRECTION('ref_axis',(0.995806686138499,-0.0845187893148275,0.0350088288095555)) ;
#39462 = DIRECTION('center_axis',(0.0914824783325311,0.381078720623587,-0.920005415661249)) ;
#39463 = DIRECTION('ref_axis',(0.995806686138498,-0.035008828809558,0.0845187893148328)) ;
#39464 = DIRECTION('center_axis',(0.0914824783325311,0.381078720623587,-0.920005415661249)) ;
#39465 = DIRECTION('ref_axis',(0.995806686138498,-0.035008828809558,0.0845187893148328)) ;
#39466 = DIRECTION('center_axis',(0.,0.,1.)) ;
#39467 = DIRECTION('ref_axis',(1.,0.,0.)) ;
#39468 = DIRECTION('center_axis',(-0.0914824783325311,-0.381078720623587,
0.920005415661249)) ;
#39469 = DIRECTION('ref_axis',(0.995806686138498,-0.035008828809558,0.0845187893148328)) ;
#39470 = DIRECTION('center_axis',(0.0914824783325254,-0.381078720623587,-0.92000541566125)) ;
#39471 = DIRECTION('ref_axis',(0.995806686138499,0.0350088288095559,0.0845187893148275)) ;
#39472 = DIRECTION('center_axis',(0.0914824783325254,-0.381078720623587,-0.92000541566125)) ;
#39473 = DIRECTION('ref_axis',(0.995806686138499,0.0350088288095559,0.0845187893148275)) ;
#39474 = DIRECTION('center_axis',(0.,0.,1.)) ;
#39475 = DIRECTION('ref_axis',(1.,0.,0.)) ;
#39476 = DIRECTION('center_axis',(-0.0914824783325254,0.381078720623587,0.92000541566125)) ;
#39477 = DIRECTION('ref_axis',(0.995806686138499,0.0350088288095559,0.0845187893148275)) ;
#39478 = DIRECTION('center_axis',(0.091482478332525,-0.920005415661247,-0.381078720623594)) ;
#39479 = DIRECTION('ref_axis',(0.995806686138499,0.0845187893148268,0.0350088288095563)) ;
#39480 = DIRECTION('center_axis',(0.091482478332525,-0.920005415661247,-0.381078720623594)) ;
#39481 = DIRECTION('ref_axis',(0.995806686138499,0.0845187893148268,0.0350088288095563)) ;
#39482 = DIRECTION('center_axis',(0.091482478332531,-0.920005415661246,0.381078720623595)) ;
#39483 = DIRECTION('ref_axis',(-0.692805212515615,-0.333687184544024,-0.639275997032796)) ;
#39484 = DIRECTION('center_axis',(-0.0989489060815955,0.703636665469238,-0.703636665469181)) ;
#39485 = DIRECTION('ref_axis',(-3.31831546202878E-14,0.707106781186516,0.707106781186579)) ;
#39486 = DIRECTION('center_axis',(0.0914824783325255,-0.381078720623586,0.92000541566125)) ;
#39487 = DIRECTION('ref_axis',(-0.839445610209476,-0.526507333754943,-0.134614616599765)) ;
#39488 = DIRECTION('center_axis',(-0.0989489060816109,0.,-0.995092515289535)) ;
#39489 = DIRECTION('ref_axis',(1.40655517650999E-14,1.,-1.41604447882206E-15)) ;
#39490 = DIRECTION('center_axis',(0.0914824783325241,0.381078720623591,0.920005415661248)) ;
#39491 = DIRECTION('ref_axis',(0.995806686138499,-0.0350088288095557,-0.0845187893148261)) ;
#39492 = DIRECTION('',(-0.0914824783325241,-0.381078720623591,-0.920005415661248)) ;
#39493 = DIRECTION('center_axis',(-0.0989489060815947,-0.703636665469224,
-0.703636665469195)) ;
#39494 = DIRECTION('ref_axis',(-2.3378433245451E-14,0.707106781186535,-0.707106781186561)) ;
#39495 = DIRECTION('center_axis',(-0.0989489060815947,-0.703636665469224,
-0.703636665469195)) ;
#39496 = DIRECTION('ref_axis',(-2.3378433245451E-14,0.707106781186535,-0.707106781186561)) ;
#39497 = DIRECTION('center_axis',(0.0914824783325315,0.920005415661255,0.381078720623574)) ;
#39498 = DIRECTION('ref_axis',(0.995806686138498,-0.0845187893148336,-0.035008828809557)) ;
#39499 = DIRECTION('',(-0.0914824783325315,-0.920005415661255,-0.381078720623574)) ;
#39500 = DIRECTION('center_axis',(-0.0989489060816085,-0.995092515289535,
6.08202833592793E-14)) ;
#39501 = DIRECTION('ref_axis',(-1.23494582202129E-14,-5.9918929754176E-14,
-1.)) ;
#39502 = DIRECTION('center_axis',(-0.0989489060816085,-0.995092515289535,
6.08202833592793E-14)) ;
#39503 = DIRECTION('ref_axis',(-1.23494582202129E-14,-5.9918929754176E-14,
-1.)) ;
#39504 = DIRECTION('center_axis',(0.0914824783325258,0.92000541566125,-0.381078720623586)) ;
#39505 = DIRECTION('ref_axis',(0.995806686138499,-0.0845187893148279,0.0350088288095559)) ;
#39506 = DIRECTION('',(-0.0914824783325258,-0.92000541566125,0.381078720623586)) ;
#39507 = DIRECTION('center_axis',(-0.0989489060816219,-0.703636665469234,
0.70363666546918)) ;
#39508 = DIRECTION('ref_axis',(4.33621020017968E-14,-0.707106781186523,-0.707106781186572)) ;
#39509 = DIRECTION('center_axis',(-0.0989489060816219,-0.703636665469234,
0.70363666546918)) ;
#39510 = DIRECTION('ref_axis',(4.33621020017968E-14,-0.707106781186523,-0.707106781186572)) ;
#39511 = DIRECTION('center_axis',(0.0914824783325313,0.381078720623583,-0.920005415661251)) ;
#39512 = DIRECTION('ref_axis',(0.995806686138498,-0.0350088288095578,0.084518789314833)) ;
#39513 = DIRECTION('',(-0.0914824783325313,-0.381078720623583,0.920005415661251)) ;
#39514 = DIRECTION('center_axis',(-0.0989489060816132,-2.16674034761705E-15,
0.995092515289534)) ;
#39515 = DIRECTION('ref_axis',(4.78474679960641E-15,-1.,-1.6933726801959E-15)) ;
#39516 = DIRECTION('center_axis',(-0.0989489060816132,-2.16674034761705E-15,
0.995092515289534)) ;
#39517 = DIRECTION('ref_axis',(4.78474679960641E-15,-1.,-1.6933726801959E-15)) ;
#39518 = DIRECTION('center_axis',(0.0914824783325254,-0.381078720623587,-0.92000541566125)) ;
#39519 = DIRECTION('ref_axis',(0.995806686138499,0.0350088288095558,0.0845187893148275)) ;
#39520 = DIRECTION('',(-0.0914824783325254,0.381078720623587,0.92000541566125)) ;
#39521 = DIRECTION('center_axis',(-0.0989489060815864,0.703636665469225,0.703636665469195)) ;
#39522 = DIRECTION('ref_axis',(-4.72700907286251E-14,-0.707106781186536,0.707106781186559)) ;
#39523 = DIRECTION('center_axis',(-0.0989489060815864,0.703636665469225,0.703636665469195)) ;
#39524 = DIRECTION('ref_axis',(-4.72700907286251E-14,-0.707106781186536,0.707106781186559)) ;
#39525 = DIRECTION('center_axis',(0.0914824783325237,-0.920005415661249,-0.381078720623589)) ;
#39526 = DIRECTION('ref_axis',(0.995806686138499,0.0845187893148259,0.0350088288095553)) ;
#39527 = DIRECTION('',(-0.0914824783325237,0.920005415661249,0.381078720623589)) ;
#39528 = DIRECTION('center_axis',(-0.0989489060816074,0.995092515289535,-1.78746959168219E-14)) ;
#39529 = DIRECTION('ref_axis',(7.99239828537599E-15,1.86738777329889E-14,
1.)) ;
#39530 = DIRECTION('center_axis',(-0.0989489060816074,0.995092515289535,-1.78746959168219E-14)) ;
#39531 = DIRECTION('ref_axis',(7.99239828537599E-15,1.86738777329889E-14,
1.)) ;
#39532 = DIRECTION('center_axis',(0.0914824783325308,-0.920005415661242,0.381078720623606)) ;
#39533 = DIRECTION('ref_axis',(0.995806686138498,0.0845187893148318,-0.0350088288095597)) ;
#39534 = DIRECTION('',(-0.0914824783325308,0.920005415661241,-0.381078720623606)) ;
#39535 = DIRECTION('center_axis',(-0.0989489060815945,0.703636665469208,-0.70363666546921)) ;
#39536 = DIRECTION('ref_axis',(-3.81282839941823E-14,0.707106781186546,0.707106781186549)) ;
#39537 = DIRECTION('center_axis',(-0.0989489060815945,0.703636665469208,-0.70363666546921)) ;
#39538 = DIRECTION('ref_axis',(-3.81282839941823E-14,0.707106781186546,0.707106781186549)) ;
#39539 = DIRECTION('center_axis',(0.0914824783325257,-0.381078720623581,0.920005415661252)) ;
#39540 = DIRECTION('ref_axis',(0.995806686138499,0.0350088288095554,-0.0845187893148279)) ;
#39541 = DIRECTION('',(-0.0914824783325257,0.381078720623581,-0.920005415661252)) ;
#39542 = DIRECTION('center_axis',(-0.0989489060816132,-4.35802109972037E-14,
-0.995092515289534)) ;
#39543 = DIRECTION('ref_axis',(1.53539584452172E-14,1.,-4.53187694081149E-14)) ;
#39544 = DIRECTION('center_axis',(-0.0989489060816132,-4.35802109972037E-14,
-0.995092515289534)) ;
#39545 = DIRECTION('ref_axis',(1.53539584452172E-14,1.,-4.53187694081149E-14)) ;
#39546 = DIRECTION('center_axis',(0.091482478332532,0.381078720623593,0.920005415661247)) ;
#39547 = DIRECTION('ref_axis',(0.995806686138498,-0.0350088288095589,-0.0845187893148333)) ;
#39548 = DIRECTION('',(-0.091482478332532,-0.381078720623593,-0.920005415661247)) ;
#39549 = DIRECTION('center_axis',(-0.0989489060816209,-0.703636665469204,
-0.703636665469211)) ;
#39550 = DIRECTION('ref_axis',(2.21060648227627E-14,0.707106781186549,-0.707106781186546)) ;
#39551 = DIRECTION('center_axis',(-0.0989489060816209,-0.703636665469204,
-0.703636665469211)) ;
#39552 = DIRECTION('ref_axis',(2.21060648227627E-14,0.707106781186549,-0.707106781186546)) ;
#39553 = DIRECTION('center_axis',(0.0914824783325256,0.920005415661251,0.381078720623585)) ;
#39554 = DIRECTION('ref_axis',(0.995806686138499,-0.0845187893148277,-0.0350088288095557)) ;
#39555 = DIRECTION('',(-0.0914824783325256,-0.920005415661251,-0.381078720623585)) ;
#39556 = DIRECTION('center_axis',(-0.098948906081604,-0.995092515289535,5.2432441356011E-14)) ;
#39557 = DIRECTION('ref_axis',(-8.39870080690671E-15,-5.18744071321563E-14,
-1.)) ;
#39558 = DIRECTION('center_axis',(-0.098948906081604,-0.995092515289535,5.2432441356011E-14)) ;
#39559 = DIRECTION('ref_axis',(-8.39870080690671E-15,-5.18744071321563E-14,
-1.)) ;
#39560 = DIRECTION('center_axis',(0.0914824783325256,0.920005415661251,-0.381078720623585)) ;
#39561 = DIRECTION('ref_axis',(0.995806686138499,-0.0845187893148277,0.0350088288095557)) ;
#39562 = DIRECTION('',(-0.0914824783325256,-0.920005415661251,0.381078720623585)) ;
#39563 = DIRECTION('center_axis',(-0.0989489060816204,-0.703636665469235,
0.70363666546918)) ;
#39564 = DIRECTION('ref_axis',(4.02934487470771E-14,-0.707106781186523,-0.707106781186572)) ;
#39565 = DIRECTION('center_axis',(-0.0989489060816204,-0.703636665469235,
0.70363666546918)) ;
#39566 = DIRECTION('ref_axis',(4.02934487470771E-14,-0.707106781186523,-0.707106781186572)) ;
#39567 = DIRECTION('center_axis',(0.0914824783325301,0.381078720623585,-0.92000541566125)) ;
#39568 = DIRECTION('ref_axis',(0.995806686138499,-0.0350088288095575,0.0845187893148319)) ;
#39569 = DIRECTION('',(-0.0914824783325301,-0.381078720623585,0.92000541566125)) ;
#39570 = DIRECTION('center_axis',(-0.0989489060816109,0.,0.995092515289535)) ;
#39571 = DIRECTION('ref_axis',(1.78024657460216E-15,-1.,1.88449524788967E-16)) ;
#39572 = DIRECTION('center_axis',(-0.0989489060816109,0.,0.995092515289535)) ;
#39573 = DIRECTION('ref_axis',(1.78024657460216E-15,-1.,1.88449524788967E-16)) ;
#39574 = DIRECTION('center_axis',(0.0914824783325252,-0.381078720623592,-0.920005415661248)) ;
#39575 = DIRECTION('ref_axis',(0.995806686138499,0.0350088288095562,0.0845187893148271)) ;
#39576 = DIRECTION('',(-0.0914824783325252,0.381078720623592,0.920005415661248)) ;
#39577 = DIRECTION('center_axis',(-0.098948906081596,0.703636665469203,0.703636665469215)) ;
#39578 = DIRECTION('ref_axis',(-2.01600895880624E-14,-0.707106781186555,0.70710678118654)) ;
#39579 = DIRECTION('center_axis',(-0.098948906081596,0.703636665469203,0.703636665469215)) ;
#39580 = DIRECTION('ref_axis',(-2.01600895880624E-14,-0.707106781186555,0.70710678118654)) ;
#39581 = DIRECTION('center_axis',(0.0914824783325312,-0.920005415661251,-0.381078720623584)) ;
#39582 = DIRECTION('ref_axis',(0.995806686138498,0.0845187893148329,0.0350088288095578)) ;
#39583 = DIRECTION('',(-0.0914824783325312,0.92000541566125,0.381078720623584)) ;
#39584 = DIRECTION('center_axis',(-0.0989489060816085,0.995092515289535,-6.26465533084806E-14)) ;
#39585 = DIRECTION('ref_axis',(-1.31353328342264E-14,6.16290089525266E-14,
1.)) ;
#39586 = DIRECTION('center_axis',(-0.0989489060816085,0.995092515289535,-6.26465533084806E-14)) ;
#39587 = DIRECTION('ref_axis',(-1.31353328342264E-14,6.16290089525266E-14,
1.)) ;
#39588 = DIRECTION('center_axis',(0.0914824783325253,-0.920005415661246,0.381078720623595)) ;
#39589 = DIRECTION('ref_axis',(0.995806686138499,0.0845187893148271,-0.0350088288095565)) ;
#39590 = DIRECTION('',(-0.0914824783325253,0.920005415661246,-0.381078720623595)) ;
#39591 = DIRECTION('center_axis',(-0.098948906081588,0.703636665469237,-0.703636665469183)) ;
#39592 = DIRECTION('ref_axis',(-3.65458425945363E-14,0.707106781186518,0.707106781186577)) ;
#39593 = DIRECTION('center_axis',(-0.098948906081588,0.703636665469237,-0.703636665469183)) ;
#39594 = DIRECTION('ref_axis',(-3.65458425945363E-14,0.707106781186518,0.707106781186577)) ;
#39595 = DIRECTION('center_axis',(0.0914824783325254,-0.381078720623587,0.92000541566125)) ;
#39596 = DIRECTION('ref_axis',(0.995806686138499,0.0350088288095558,-0.0845187893148275)) ;
#39597 = DIRECTION('',(-0.0914824783325254,0.381078720623587,-0.92000541566125)) ;
#39598 = DIRECTION('center_axis',(-0.0989489060816109,0.,-0.995092515289535)) ;
#39599 = DIRECTION('ref_axis',(1.4022783078623E-14,1.,-1.41604447882206E-15)) ;
#39600 = DIRECTION('center_axis',(-0.0989489060816109,0.,-0.995092515289535)) ;
#39601 = DIRECTION('ref_axis',(1.4022783078623E-14,1.,-1.41604447882206E-15)) ;
#39602 = DIRECTION('center_axis',(0.0914824783325299,0.38107872062359,0.920005415661248)) ;
#39603 = DIRECTION('ref_axis',(0.995806686138498,-0.0350088288095579,-0.0845187893148314)) ;
#39604 = DIRECTION('',(-0.0914824783325299,-0.38107872062359,-0.920005415661248)) ;
#39605 = DIRECTION('center_axis',(-0.0989489060816232,-0.703636665469224,
-0.703636665469191)) ;
#39606 = DIRECTION('ref_axis',(3.05314960587173E-14,0.707106781186529,-0.707106781186566)) ;
#39607 = DIRECTION('center_axis',(-0.0989489060816232,-0.703636665469224,
-0.703636665469191)) ;
#39608 = DIRECTION('ref_axis',(3.05314960587173E-14,0.707106781186529,-0.707106781186566)) ;
#39609 = DIRECTION('center_axis',(0.0914824783325257,0.920005415661255,0.381078720623574)) ;
#39610 = DIRECTION('ref_axis',(0.995806686138499,-0.0845187893148283,-0.0350088288095548)) ;
#39611 = DIRECTION('',(-0.0914824783325257,-0.920005415661255,-0.381078720623574)) ;
#39612 = DIRECTION('center_axis',(-0.0989489060816096,-0.995092515289535,
6.65156456481759E-14)) ;
#39613 = DIRECTION('ref_axis',(4.57624945303127E-15,-6.72584373100524E-14,
-1.)) ;
#39614 = DIRECTION('center_axis',(-0.0989489060816096,-0.995092515289535,
6.65156456481759E-14)) ;
#39615 = DIRECTION('ref_axis',(4.57624945303127E-15,-6.72584373100524E-14,
-1.)) ;
#39616 = DIRECTION('center_axis',(0.0914824783325315,0.92000541566125,-0.381078720623586)) ;
#39617 = DIRECTION('ref_axis',(0.995806686138498,-0.0845187893148332,0.0350088288095581)) ;
#39618 = DIRECTION('',(-0.0914824783325315,-0.92000541566125,0.381078720623586)) ;
#39619 = DIRECTION('center_axis',(-0.098948906081596,-0.703636665469235,0.703636665469184)) ;
#39620 = DIRECTION('ref_axis',(-3.45945212740262E-14,-0.707106781186519,-0.707106781186576)) ;
#39621 = DIRECTION('center_axis',(-0.098948906081596,-0.703636665469235,0.703636665469184)) ;
#39622 = DIRECTION('ref_axis',(-3.45945212740262E-14,-0.707106781186519,-0.707106781186576)) ;
#39623 = DIRECTION('center_axis',(0.0914824783325256,0.381078720623584,-0.920005415661251)) ;
#39624 = DIRECTION('ref_axis',(0.995806686138499,-0.0350088288095556,0.0845187893148277)) ;
#39625 = DIRECTION('',(-0.0914824783325255,-0.381078720623584,0.920005415661251)) ;
#39626 = DIRECTION('center_axis',(-0.0989489060816109,0.,0.995092515289535)) ;
#39627 = DIRECTION('ref_axis',(1.40655517651E-14,-1.,1.3953283963098E-15)) ;
#39628 = DIRECTION('center_axis',(-0.0989489060816109,0.,0.995092515289535)) ;
#39629 = DIRECTION('ref_axis',(1.40655517651E-14,-1.,1.3953283963098E-15)) ;
#39630 = DIRECTION('center_axis',(0.0914824783325255,-0.381078720623586,-0.92000541566125)) ;
#39631 = DIRECTION('ref_axis',(0.995806686138499,0.0350088288095558,0.0845187893148275)) ;
#39632 = DIRECTION('',(-0.0914824783325255,0.381078720623586,0.92000541566125)) ;
#39633 = DIRECTION('center_axis',(-0.0989489060815955,0.70363666546922,0.703636665469198)) ;
#39634 = DIRECTION('ref_axis',(-2.49234520444301E-14,-0.707106781186538,0.707106781186557)) ;
#39635 = DIRECTION('center_axis',(-0.0989489060815955,0.70363666546922,0.703636665469198)) ;
#39636 = DIRECTION('ref_axis',(-2.49234520444301E-14,-0.707106781186538,0.707106781186557)) ;
#39637 = DIRECTION('center_axis',(0.091482478332531,-0.920005415661246,-0.381078720623595)) ;
#39638 = DIRECTION('ref_axis',(0.995806686138498,0.0845187893148324,0.0350088288095587)) ;
#39639 = DIRECTION('',(-0.091482478332531,0.920005415661246,0.381078720623595)) ;
#39640 = DIRECTION('center_axis',(-0.0989489060816065,0.995092515289535,-5.10705597623483E-15)) ;
#39641 = DIRECTION('ref_axis',(-1.26381468539324E-14,3.88860916576948E-15,
1.)) ;
#39642 = DIRECTION('center_axis',(-0.0989489060816065,0.995092515289535,-5.10705597623483E-15)) ;
#39643 = DIRECTION('ref_axis',(-1.26381468539324E-14,3.88860916576948E-15,
1.)) ;
#39644 = DIRECTION('center_axis',(0.0914824783325236,-0.920005415661245,0.3810787206236)) ;
#39645 = DIRECTION('ref_axis',(0.995806686138499,0.0845187893148253,-0.0350088288095563)) ;
#39646 = DIRECTION('',(-0.0914824783325235,0.920005415661245,-0.3810787206236)) ;
#39647 = DIRECTION('center_axis',(-0.0989489060816173,0.703636665469211,-0.703636665469204)) ;
#39648 = DIRECTION('ref_axis',(3.62090391885301E-14,0.707106781186547,0.707106781186548)) ;
#39649 = DIRECTION('center_axis',(-0.0989489060816173,0.703636665469211,-0.703636665469204)) ;
#39650 = DIRECTION('ref_axis',(3.62090391885301E-14,0.707106781186547,0.707106781186548)) ;
#39651 = DIRECTION('center_axis',(0.0914824783325314,-0.381078720623581,0.920005415661252)) ;
#39652 = DIRECTION('ref_axis',(0.995806686138498,0.0350088288095576,-0.0845187893148332)) ;
#39653 = DIRECTION('',(-0.0914824783325314,0.381078720623581,-0.920005415661252)) ;
#39654 = DIRECTION('center_axis',(-0.0989489060816132,-4.14134706495866E-14,
-0.995092515289534)) ;
#39655 = DIRECTION('ref_axis',(4.70455551246209E-16,1.,-4.16426671532777E-14)) ;
#39656 = DIRECTION('center_axis',(-0.0989489060816132,-4.14134706495866E-14,
-0.995092515289534)) ;
#39657 = DIRECTION('ref_axis',(4.70455551246209E-16,1.,-4.16426671532777E-14)) ;
#39658 = DIRECTION('center_axis',(0.0914824783325263,0.381078720623593,0.920005415661247)) ;
#39659 = DIRECTION('ref_axis',(0.995806686138499,-0.0350088288095567,-0.0845187893148281)) ;
#39660 = DIRECTION('',(-0.0914824783325263,-0.381078720623593,-0.920005415661247)) ;
#39661 = DIRECTION('center_axis',(-0.098948906081588,-0.703636665469206,-0.703636665469214)) ;
#39662 = DIRECTION('ref_axis',(-4.28809542789309E-14,0.707106781186554,-0.707106781186541)) ;
#39663 = DIRECTION('center_axis',(-0.098948906081588,-0.703636665469206,-0.703636665469214)) ;
#39664 = DIRECTION('ref_axis',(-4.28809542789309E-14,0.707106781186554,-0.707106781186541)) ;
#39665 = DIRECTION('center_axis',(0.0914824783325256,0.920005415661251,0.381078720623585)) ;
#39666 = DIRECTION('ref_axis',(0.995806686138499,-0.0845187893148277,-0.0350088288095557)) ;
#39667 = DIRECTION('',(-0.0914824783325256,-0.920005415661251,-0.381078720623585)) ;
#39668 = DIRECTION('center_axis',(-0.0989489060816085,-0.995092515289535,
4.61337389853213E-14)) ;
#39669 = DIRECTION('ref_axis',(3.44822534720232E-15,-4.66893721575551E-14,
-1.)) ;
#39670 = DIRECTION('center_axis',(-0.0989489060816085,-0.995092515289535,
4.61337389853213E-14)) ;
#39671 = DIRECTION('ref_axis',(3.44822534720232E-15,-4.66893721575551E-14,
-1.)) ;
#39672 = DIRECTION('center_axis',(0.0914824783325317,0.920005415661254,-0.381078720623575)) ;
#39673 = DIRECTION('ref_axis',(0.995806686138498,-0.0845187893148337,0.0350088288095571)) ;
#39674 = DIRECTION('',(-0.0914824783325317,-0.920005415661254,0.381078720623575)) ;
#39675 = DIRECTION('center_axis',(-0.0989489060815971,-0.703636665469235,
0.703636665469183)) ;
#39676 = DIRECTION('ref_axis',(-3.36749945147721E-14,-0.707106781186519,-0.707106781186576)) ;
#39677 = DIRECTION('center_axis',(-0.0989489060815971,-0.703636665469235,
0.703636665469183)) ;
#39678 = DIRECTION('ref_axis',(-3.36749945147721E-14,-0.707106781186519,-0.707106781186576)) ;
#39679 = DIRECTION('center_axis',(0.0914824783325234,0.381078720623582,-0.920005415661252)) ;
#39680 = DIRECTION('ref_axis',(0.995806686138499,-0.0350088288095545,0.0845187893148258)) ;
#39681 = DIRECTION('',(-0.0914824783325234,-0.381078720623582,0.920005415661252)) ;
#39682 = DIRECTION('center_axis',(-0.0989489060816109,4.14134706495867E-14,
0.995092515289535)) ;
#39683 = DIRECTION('ref_axis',(1.57549148809384E-14,-1.,4.31629603053873E-14)) ;
#39684 = DIRECTION('center_axis',(-0.0989489060816109,4.14134706495867E-14,
0.995092515289535)) ;
#39685 = DIRECTION('ref_axis',(1.57549148809384E-14,-1.,4.31629603053873E-14)) ;
#39686 = DIRECTION('center_axis',(0.091482478332531,-0.381078720623592,-0.920005415661248)) ;
#39687 = DIRECTION('ref_axis',(0.995806686138498,0.0350088288095584,0.0845187893148324)) ;
#39688 = DIRECTION('',(-0.091482478332531,0.381078720623591,0.920005415661247)) ;
#39689 = DIRECTION('center_axis',(-0.0989489060816217,0.703636665469202,0.703636665469212)) ;
#39690 = DIRECTION('ref_axis',(2.68961577081787E-14,-0.707106781186551,0.707106781186544)) ;
#39691 = DIRECTION('center_axis',(-0.0989489060816217,0.703636665469202,0.703636665469212)) ;
#39692 = DIRECTION('ref_axis',(2.68961577081787E-14,-0.707106781186551,0.707106781186544)) ;
#39693 = DIRECTION('center_axis',(0.0914824783325255,-0.920005415661251,-0.381078720623585)) ;
#39694 = DIRECTION('ref_axis',(0.995806686138499,0.0845187893148276,0.0350088288095556)) ;
#39695 = DIRECTION('',(-0.0914824783325255,0.920005415661251,0.381078720623585)) ;
#39696 = DIRECTION('center_axis',(-0.098948906081604,0.995092515289535,-6.50298460973902E-14)) ;
#39697 = DIRECTION('ref_axis',(-9.37703451006639E-15,6.44357040025749E-14,
1.)) ;
#39698 = DIRECTION('center_axis',(-0.098948906081604,0.995092515289535,-6.50298460973902E-14)) ;
#39699 = DIRECTION('ref_axis',(-9.37703451006639E-15,6.44357040025749E-14,
1.)) ;
#39700 = DIRECTION('center_axis',(0.0914824783325253,-0.920005415661247,0.381078720623595)) ;
#39701 = DIRECTION('ref_axis',(0.995806686138499,0.084518789314827,-0.0350088288095565)) ;
#39702 = DIRECTION('',(-0.0914824783325253,0.920005415661246,-0.381078720623595)) ;
#39703 = DIRECTION('center_axis',(-0.0989489060816193,0.703636665469236,-0.703636665469179)) ;
#39704 = DIRECTION('ref_axis',(3.96946871364003E-14,0.707106781186521,0.707106781186574)) ;
#39705 = DIRECTION('center_axis',(-0.0989489060816193,0.703636665469236,-0.703636665469179)) ;
#39706 = DIRECTION('ref_axis',(3.96946871364003E-14,0.707106781186521,0.707106781186574)) ;
#39707 = DIRECTION('center_axis',(0.0914824783325311,-0.381078720623587,0.920005415661249)) ;
#39708 = DIRECTION('ref_axis',(0.995806686138498,0.035008828809558,-0.0845187893148328)) ;
#39709 = DIRECTION('',(-0.0914824783325311,0.381078720623587,-0.920005415661249)) ;
#39710 = DIRECTION('center_axis',(-0.0989489060816109,2.16674034761701E-15,
-0.995092515289535)) ;
#39711 = DIRECTION('ref_axis',(-8.55373729538575E-16,1.,2.21795735026448E-15)) ;
#39712 = DIRECTION('center_axis',(-0.0989489060816109,2.16674034761701E-15,
-0.995092515289535)) ;
#39713 = DIRECTION('ref_axis',(-8.55373729538575E-16,1.,2.21795735026448E-15)) ;
#39714 = DIRECTION('center_axis',(0.0914824783325242,0.38107872062359,0.920005415661249)) ;
#39715 = DIRECTION('ref_axis',(0.995806686138499,-0.0350088288095556,-0.0845187893148262)) ;
#39716 = DIRECTION('',(-0.0914824783325242,-0.38107872062359,-0.920005415661249)) ;
#39717 = DIRECTION('center_axis',(-0.098948906081595,-0.703636665469224,-0.703636665469195)) ;
#39718 = DIRECTION('ref_axis',(-2.30683602684933E-14,0.707106781186534,-0.70710678118656)) ;
#39719 = DIRECTION('center_axis',(-0.098948906081595,-0.703636665469224,-0.703636665469195)) ;
#39720 = DIRECTION('ref_axis',(-2.30683602684933E-14,0.707106781186534,-0.70710678118656)) ;
#39721 = DIRECTION('center_axis',(0.0914824783325315,0.920005415661255,0.381078720623574)) ;
#39722 = DIRECTION('ref_axis',(0.995806686138498,-0.0845187893148336,-0.035008828809557)) ;
#39723 = DIRECTION('',(-0.0914824783325315,-0.920005415661255,-0.381078720623574)) ;
#39724 = DIRECTION('center_axis',(-0.0989489060816085,-0.995092515289535,
6.21821649529419E-14)) ;
#39725 = DIRECTION('ref_axis',(-1.25098407945014E-14,-6.12460955564131E-14,
-1.)) ;
#39726 = DIRECTION('center_axis',(-0.0989489060816085,-0.995092515289535,
6.21821649529419E-14)) ;
#39727 = DIRECTION('ref_axis',(-1.25098407945014E-14,-6.12460955564131E-14,
-1.)) ;
#39728 = DIRECTION('center_axis',(0.0914824783325258,0.92000541566125,-0.381078720623586)) ;
#39729 = DIRECTION('ref_axis',(0.995806686138499,-0.0845187893148279,0.0350088288095559)) ;
#39730 = DIRECTION('',(-0.0914824783325258,-0.92000541566125,0.381078720623586)) ;
#39731 = DIRECTION('center_axis',(-0.0989489060815885,-0.703636665469235,
0.703636665469185)) ;
#39732 = DIRECTION('ref_axis',(-3.78182110172248E-14,-0.70710678118652,-0.707106781186575)) ;
#39733 = DIRECTION('center_axis',(-0.0989489060815885,-0.703636665469235,
0.703636665469185)) ;
#39734 = DIRECTION('ref_axis',(-3.78182110172248E-14,-0.70710678118652,-0.707106781186575)) ;
#39735 = DIRECTION('center_axis',(0.0914824783325255,0.381078720623584,-0.920005415661251)) ;
#39736 = DIRECTION('ref_axis',(0.995806686138499,-0.0350088288095556,0.0845187893148277)) ;
#39737 = DIRECTION('',(-0.0914824783325255,-0.381078720623584,0.920005415661251)) ;
#39738 = DIRECTION('center_axis',(-0.0989489060816109,0.,0.995092515289535)) ;
#39739 = DIRECTION('ref_axis',(1.40334752502423E-14,-1.,1.3953283963098E-15)) ;
#39740 = DIRECTION('center_axis',(-0.0989489060816109,0.,0.995092515289535)) ;
#39741 = DIRECTION('ref_axis',(1.40334752502423E-14,-1.,1.3953283963098E-15)) ;
#39742 = DIRECTION('center_axis',(0.0914824783325312,-0.381078720623586,-0.92000541566125)) ;
#39743 = DIRECTION('ref_axis',(0.995806686138498,0.0350088288095579,0.0845187893148329)) ;
#39744 = DIRECTION('',(-0.0914824783325312,0.381078720623586,0.92000541566125)) ;
#39745 = DIRECTION('center_axis',(-0.0989489060816175,0.703636665469224,0.703636665469192)) ;
#39746 = DIRECTION('ref_axis',(1.2600724253265E-14,-0.707106781186531,0.707106781186564)) ;
#39747 = DIRECTION('center_axis',(-0.0989489060816175,0.703636665469224,0.703636665469192)) ;
#39748 = DIRECTION('ref_axis',(1.2600724253265E-14,-0.707106781186531,0.707106781186564)) ;
#39749 = DIRECTION('center_axis',(0.0914824783325238,-0.920005415661249,-0.381078720623589)) ;
#39750 = DIRECTION('ref_axis',(0.995806686138499,0.0845187893148259,0.0350088288095554)) ;
#39751 = DIRECTION('',(-0.0914824783325237,0.920005415661249,0.381078720623589)) ;
#39752 = DIRECTION('center_axis',(-0.0989489060816076,0.995092515289535,-1.53211679287045E-14)) ;
#39753 = DIRECTION('ref_axis',(8.62858249672031E-15,1.6239403907435E-14,1.)) ;
#39754 = DIRECTION('center_axis',(-0.0989489060816076,0.995092515289535,-1.53211679287045E-14)) ;
#39755 = DIRECTION('ref_axis',(8.62858249672031E-15,1.6239403907435E-14,1.)) ;
#39756 = DIRECTION('center_axis',(0.0914824783325308,-0.920005415661242,0.381078720623606)) ;
#39757 = DIRECTION('ref_axis',(0.995806686138498,0.0845187893148317,-0.0350088288095596)) ;
#39758 = DIRECTION('',(-0.0914824783325308,0.920005415661242,-0.381078720623606)) ;
#39759 = DIRECTION('center_axis',(-0.0989489060815925,0.703636665469211,-0.703636665469208)) ;
#39760 = DIRECTION('ref_axis',(-4.25013821864484E-14,0.707106781186543,0.707106781186552)) ;
#39761 = DIRECTION('center_axis',(-0.0989489060815925,0.703636665469211,-0.703636665469208)) ;
#39762 = DIRECTION('ref_axis',(-4.25013821864484E-14,0.707106781186543,0.707106781186552)) ;
#39763 = DIRECTION('center_axis',(0.0914824783325257,-0.381078720623582,0.920005415661252)) ;
#39764 = DIRECTION('ref_axis',(0.995806686138499,0.0350088288095554,-0.0845187893148279)) ;
#39765 = DIRECTION('',(-0.0914824783325257,0.381078720623582,-0.920005415661252)) ;
#39766 = DIRECTION('center_axis',(-0.0989489060816109,-4.35802109972037E-14,
-0.995092515289535)) ;
#39767 = DIRECTION('ref_axis',(9.55880142759342E-15,1.,-4.4753420833748E-14)) ;
#39768 = DIRECTION('center_axis',(-0.0989489060816109,-4.35802109972037E-14,
-0.995092515289535)) ;
#39769 = DIRECTION('ref_axis',(9.55880142759342E-15,1.,-4.4753420833748E-14)) ;
#39770 = DIRECTION('center_axis',(0.0914824783325263,0.381078720623592,0.920005415661247)) ;
#39771 = DIRECTION('ref_axis',(0.995806686138499,-0.0350088288095567,-0.0845187893148281)) ;
#39772 = DIRECTION('',(-0.0914824783325263,-0.381078720623592,-0.920005415661247)) ;
#39773 = DIRECTION('center_axis',(-0.0989489060815955,-0.703636665469203,
-0.703636665469215)) ;
#39774 = DIRECTION('ref_axis',(-2.4260537404038E-14,0.707106781186555,-0.70710678118654)) ;
#39775 = DIRECTION('center_axis',(-0.0989489060815955,-0.703636665469203,
-0.703636665469215)) ;
#39776 = DIRECTION('ref_axis',(-2.4260537404038E-14,0.707106781186555,-0.70710678118654)) ;
#39777 = DIRECTION('center_axis',(0.0914824783325313,0.92000541566125,0.381078720623585)) ;
#39778 = DIRECTION('ref_axis',(0.995806686138498,-0.084518789314833,-0.0350088288095579)) ;
#39779 = DIRECTION('',(-0.0914824783325313,-0.92000541566125,-0.381078720623585)) ;
#39780 = DIRECTION('center_axis',(-0.0989489060816096,-0.995092515289535,
4.42611517940352E-14)) ;
#39781 = DIRECTION('ref_axis',(-8.98142416015488E-15,-4.35926519523351E-14,
-1.)) ;
#39782 = DIRECTION('center_axis',(-0.0989489060816096,-0.995092515289535,
4.42611517940352E-14)) ;
#39783 = DIRECTION('ref_axis',(-8.98142416015488E-15,-4.35926519523351E-14,
-1.)) ;
#39784 = DIRECTION('center_axis',(0.091482478332526,0.920005415661255,-0.381078720623575)) ;
#39785 = DIRECTION('ref_axis',(0.995806686138499,-0.0845187893148284,0.0350088288095549)) ;
#39786 = DIRECTION('',(-0.0914824783325259,-0.920005415661255,0.381078720623575)) ;
#39787 = DIRECTION('center_axis',(-0.0989489060816214,-0.703636665469236,
0.703636665469179)) ;
#39788 = DIRECTION('ref_axis',(4.08868642719443E-14,-0.707106781186522,-0.707106781186573)) ;
#39789 = DIRECTION('center_axis',(-0.0989489060816214,-0.703636665469236,
0.703636665469179)) ;
#39790 = DIRECTION('ref_axis',(4.08868642719443E-14,-0.707106781186522,-0.707106781186573)) ;
#39791 = DIRECTION('center_axis',(0.0914824783325291,0.381078720623582,-0.920005415661252)) ;
#39792 = DIRECTION('ref_axis',(0.995806686138499,-0.0350088288095568,0.0845187893148311)) ;
#39793 = DIRECTION('',(-0.0914824783325291,-0.381078720623582,0.920005415661252)) ;
#39794 = DIRECTION('center_axis',(-0.0989489060816133,4.14134706495866E-14,
0.995092515289534)) ;
#39795 = DIRECTION('ref_axis',(6.59172380325654E-15,-1.,4.22561304999312E-14)) ;
#39796 = DIRECTION('center_axis',(-0.0989489060816133,4.14134706495866E-14,
0.995092515289534)) ;
#39797 = DIRECTION('ref_axis',(6.59172380325654E-15,-1.,4.22561304999312E-14)) ;
#39798 = DIRECTION('center_axis',(0.0914824783325252,-0.381078720623591,-0.920005415661248)) ;
#39799 = DIRECTION('ref_axis',(0.995806686138499,0.0350088288095562,0.0845187893148272)) ;
#39800 = DIRECTION('',(-0.0914824783325252,0.381078720623591,0.920005415661248)) ;
#39801 = DIRECTION('center_axis',(-0.0989489060815885,0.703636665469205,0.703636665469215)) ;
#39802 = DIRECTION('ref_axis',(-3.85987395454284E-14,-0.707106781186555,0.70710678118654)) ;
#39803 = DIRECTION('center_axis',(-0.0989489060815885,0.703636665469205,0.703636665469215)) ;
#39804 = DIRECTION('ref_axis',(-3.85987395454284E-14,-0.707106781186555,0.70710678118654)) ;
#39805 = DIRECTION('center_axis',(0.0914824783325255,-0.920005415661251,-0.381078720623585)) ;
#39806 = DIRECTION('ref_axis',(0.995806686138499,0.0845187893148276,0.0350088288095556)) ;
#39807 = DIRECTION('',(-0.0914824783325255,0.920005415661251,0.381078720623585)) ;
#39808 = DIRECTION('center_axis',(-0.0989489060816085,0.995092515289535,-6.11144365156102E-14)) ;
#39809 = DIRECTION('ref_axis',(2.2453560400387E-15,6.1689820678611E-14,1.)) ;
#39810 = DIRECTION('center_axis',(-0.0989489060816085,0.995092515289535,-6.11144365156102E-14)) ;
#39811 = DIRECTION('ref_axis',(2.2453560400387E-15,6.1689820678611E-14,1.)) ;
#39812 = DIRECTION('center_axis',(0.091482478332531,-0.920005415661246,0.381078720623595)) ;
#39813 = DIRECTION('ref_axis',(0.995806686138498,0.0845187893148323,-0.0350088288095587)) ;
#39814 = DIRECTION('',(-0.091482478332531,0.920005415661246,-0.381078720623595)) ;
#39815 = DIRECTION('center_axis',(-0.0989489060815932,0.70363666546921,-0.703636665469208)) ;
#39816 = DIRECTION('ref_axis',(-4.25548430445443E-14,0.707106781186543,0.707106781186552)) ;
#39817 = DIRECTION('center_axis',(-0.0989489060815932,0.70363666546921,-0.703636665469208)) ;
#39818 = DIRECTION('ref_axis',(-4.25548430445443E-14,0.707106781186543,0.707106781186552)) ;
#39819 = DIRECTION('center_axis',(0.0914824783325244,-0.381078720623583,0.920005415661252)) ;
#39820 = DIRECTION('ref_axis',(0.995806686138499,0.0350088288095551,-0.0845187893148267)) ;
#39821 = DIRECTION('',(-0.0914824783325244,0.381078720623583,-0.920005415661251)) ;
#39822 = DIRECTION('center_axis',(-0.0989489060815898,-4.35802109972035E-14,
-0.995092515289537)) ;
#39823 = DIRECTION('ref_axis',(-3.85720091163795E-14,1.,-3.99259053476647E-14)) ;
#39824 = DIRECTION('center_axis',(-0.0989489060815898,-4.35802109972035E-14,
-0.995092515289537)) ;
#39825 = DIRECTION('ref_axis',(-3.85720091163795E-14,1.,-3.99259053476647E-14)) ;
#39826 = DIRECTION('center_axis',(0.0914824783325321,0.381078720623592,0.920005415661247)) ;
#39827 = DIRECTION('ref_axis',(0.995806686138498,-0.0350088288095589,-0.0845187893148334)) ;
#39828 = DIRECTION('',(-0.091482478332532,-0.381078720623592,-0.920005415661247)) ;
#39829 = DIRECTION('center_axis',(-0.0989489060816185,-0.703636665469205,
-0.70363666546921)) ;
#39830 = DIRECTION('ref_axis',(1.60115269998003E-14,0.707106781186549,-0.707106781186546)) ;
#39831 = DIRECTION('center_axis',(-0.0989489060816185,-0.703636665469205,
-0.70363666546921)) ;
#39832 = DIRECTION('ref_axis',(1.60115269998003E-14,0.707106781186549,-0.707106781186546)) ;
#39833 = DIRECTION('center_axis',(0.0914824783325248,0.920005415661252,0.381078720623582)) ;
#39834 = DIRECTION('ref_axis',(0.995806686138499,-0.0845187893148271,-0.0350088288095551)) ;
#39835 = DIRECTION('',(-0.0914824783325248,-0.920005415661252,-0.381078720623582)) ;
#39836 = DIRECTION('center_axis',(-0.0989489060816036,-0.995092515289535,
5.58371453401675E-14)) ;
#39837 = DIRECTION('ref_axis',(-7.30809930174505E-15,-5.5452943320968E-14,
-1.)) ;
#39838 = DIRECTION('center_axis',(-0.0989489060816036,-0.995092515289535,
5.58371453401675E-14)) ;
#39839 = DIRECTION('ref_axis',(-7.30809930174505E-15,-5.5452943320968E-14,
-1.)) ;
#39840 = DIRECTION('center_axis',(0.0914824783325258,0.92000541566125,-0.381078720623586)) ;
#39841 = DIRECTION('ref_axis',(0.995806686138499,-0.0845187893148278,0.0350088288095558)) ;
#39842 = DIRECTION('',(-0.0914824783325258,-0.92000541566125,0.381078720623586)) ;
#39843 = DIRECTION('center_axis',(-0.0989489060816206,-0.703636665469235,
0.70363666546918)) ;
#39844 = DIRECTION('ref_axis',(4.03736400342214E-14,-0.707106781186522,-0.707106781186573)) ;
#39845 = DIRECTION('center_axis',(-0.0989489060816206,-0.703636665469235,
0.70363666546918)) ;
#39846 = DIRECTION('ref_axis',(4.03736400342214E-14,-0.707106781186522,-0.707106781186573)) ;
#39847 = DIRECTION('center_axis',(0.0914824783325312,0.381078720623584,-0.92000541566125)) ;
#39848 = DIRECTION('ref_axis',(0.995806686138498,-0.0350088288095578,0.084518789314833)) ;
#39849 = DIRECTION('',(-0.0914824783325312,-0.381078720623584,0.92000541566125)) ;
#39850 = DIRECTION('center_axis',(-0.0989489060816133,-2.16674034761706E-15,
0.995092515289534)) ;
#39851 = DIRECTION('ref_axis',(4.89166851579873E-15,-1.,-1.67265659768364E-15)) ;
#39852 = DIRECTION('center_axis',(-0.0989489060816133,-2.16674034761706E-15,
0.995092515289534)) ;
#39853 = DIRECTION('ref_axis',(4.89166851579873E-15,-1.,-1.67265659768364E-15)) ;
#39854 = DIRECTION('center_axis',(0.0914824783325243,-0.381078720623587,-0.92000541566125)) ;
#39855 = DIRECTION('ref_axis',(0.995806686138499,0.0350088288095554,0.0845187893148264)) ;
#39856 = DIRECTION('',(-0.0914824783325243,0.381078720623587,0.92000541566125)) ;
#39857 = DIRECTION('center_axis',(-0.0989489060815945,0.703636665469201,0.703636665469218)) ;
#39858 = DIRECTION('ref_axis',(-2.16463014431357E-14,-0.707106781186558,0.707106781186537)) ;
#39859 = DIRECTION('center_axis',(-0.0989489060815945,0.703636665469201,0.703636665469218)) ;
#39860 = DIRECTION('ref_axis',(-2.16463014431357E-14,-0.707106781186558,0.707106781186537)) ;
#39861 = DIRECTION('center_axis',(0.0914824783325312,-0.92000541566125,-0.381078720623584)) ;
#39862 = DIRECTION('ref_axis',(0.995806686138498,0.0845187893148329,0.0350088288095578)) ;
#39863 = DIRECTION('',(-0.0914824783325312,0.92000541566125,0.381078720623584)) ;
#39864 = DIRECTION('center_axis',(-0.0989489060816085,0.995092515289535,-6.33274941053119E-14)) ;
#39865 = DIRECTION('ref_axis',(-1.32208702071803E-14,6.23146444576098E-14,
1.)) ;
#39866 = DIRECTION('center_axis',(-0.0989489060816085,0.995092515289535,-6.33274941053119E-14)) ;
#39867 = DIRECTION('ref_axis',(-1.32208702071803E-14,6.23146444576098E-14,
1.)) ;
#39868 = DIRECTION('center_axis',(0.0914824783325252,-0.920005415661246,0.381078720623595)) ;
#39869 = DIRECTION('ref_axis',(0.995806686138499,0.084518789314827,-0.0350088288095565)) ;
#39870 = DIRECTION('',(-0.0914824783325252,0.920005415661246,-0.381078720623595)) ;
#39871 = DIRECTION('center_axis',(-0.098948906081588,0.703636665469212,-0.703636665469208)) ;
#39872 = DIRECTION('ref_axis',(-3.98443775390689E-14,0.707106781186543,0.707106781186552)) ;
#39873 = DIRECTION('center_axis',(-0.098948906081588,0.703636665469212,-0.703636665469208)) ;
#39874 = DIRECTION('ref_axis',(-3.98443775390689E-14,0.707106781186543,0.707106781186552)) ;
#39875 = DIRECTION('center_axis',(0.0914824783325244,-0.381078720623584,0.920005415661252)) ;
#39876 = DIRECTION('ref_axis',(0.995806686138499,0.0350088288095551,-0.0845187893148267)) ;
#39877 = DIRECTION('',(-0.0914824783325244,0.381078720623583,-0.920005415661251)) ;
#39878 = DIRECTION('center_axis',(-0.0989489060816109,-4.35802109972033E-14,
-0.995092515289535)) ;
#39879 = DIRECTION('ref_axis',(1.24831103654534E-14,1.,-4.50601525070747E-14)) ;
#39880 = DIRECTION('center_axis',(-0.0989489060816109,-4.35802109972033E-14,
-0.995092515289535)) ;
#39881 = DIRECTION('ref_axis',(1.24831103654534E-14,1.,-4.50601525070747E-14)) ;
#39882 = DIRECTION('center_axis',(0.0914824783325321,0.381078720623592,0.920005415661247)) ;
#39883 = DIRECTION('ref_axis',(0.995806686138498,-0.0350088288095588,-0.0845187893148334)) ;
#39884 = DIRECTION('',(-0.0914824783325321,-0.381078720623592,-0.920005415661247)) ;
#39885 = DIRECTION('center_axis',(-0.0989489060816214,-0.703636665469203,
-0.703636665469212)) ;
#39886 = DIRECTION('ref_axis',(2.32073584995436E-14,0.707106781186551,-0.707106781186544)) ;
#39887 = DIRECTION('center_axis',(-0.0989489060816214,-0.703636665469203,
-0.703636665469212)) ;
#39888 = DIRECTION('ref_axis',(2.32073584995436E-14,0.707106781186551,-0.707106781186544)) ;
#39889 = DIRECTION('center_axis',(0.0914824783325256,0.920005415661251,0.381078720623585)) ;
#39890 = DIRECTION('ref_axis',(0.995806686138499,-0.0845187893148278,-0.0350088288095557)) ;
#39891 = DIRECTION('',(-0.0914824783325256,-0.92000541566125,-0.381078720623585)) ;
#39892 = DIRECTION('center_axis',(-0.0989489060816082,-0.995092515289535,
5.17051833170949E-14)) ;
#39893 = DIRECTION('ref_axis',(1.83370743269828E-15,-5.20962696932553E-14,
-1.)) ;
#39894 = DIRECTION('center_axis',(-0.0989489060816082,-0.995092515289535,
5.17051833170949E-14)) ;
#39895 = DIRECTION('ref_axis',(1.83370743269828E-15,-5.20962696932553E-14,
-1.)) ;
#39896 = DIRECTION('center_axis',(0.0914824783325307,0.920005415661251,-0.381078720623582)) ;
#39897 = DIRECTION('ref_axis',(0.995806686138498,-0.0845187893148325,0.0350088288095574)) ;
#39898 = DIRECTION('',(-0.0914824783325307,-0.920005415661251,0.381078720623582)) ;
#39899 = DIRECTION('center_axis',(-0.0989489060815945,-0.703636665469239,
0.70363666546918)) ;
#39900 = DIRECTION('ref_axis',(-3.59845035845265E-14,-0.707106781186516,-0.707106781186579)) ;
#39901 = DIRECTION('center_axis',(-0.0989489060815945,-0.703636665469239,
0.70363666546918)) ;
#39902 = DIRECTION('ref_axis',(-3.59845035845265E-14,-0.707106781186516,-0.707106781186579)) ;
#39903 = DIRECTION('center_axis',(0.0914824783325255,0.381078720623585,-0.920005415661251)) ;
#39904 = DIRECTION('ref_axis',(0.995806686138499,-0.0350088288095557,0.0845187893148276)) ;
#39905 = DIRECTION('',(-0.0914824783325255,-0.381078720623585,0.920005415661251)) ;
#39906 = DIRECTION('center_axis',(-0.0989489060816109,0.,0.995092515289535)) ;
#39907 = DIRECTION('ref_axis',(1.39853604779557E-14,-1.,1.3953283963098E-15)) ;
#39908 = DIRECTION('center_axis',(-0.0989489060816109,0.,0.995092515289535)) ;
#39909 = DIRECTION('ref_axis',(1.39853604779557E-14,-1.,1.3953283963098E-15)) ;
#39910 = DIRECTION('center_axis',(0.0914824783325243,-0.381078720623587,-0.92000541566125)) ;
#39911 = DIRECTION('ref_axis',(0.995806686138499,0.0350088288095554,0.0845187893148264)) ;
#39912 = DIRECTION('',(-0.0914824783325243,0.381078720623587,0.92000541566125)) ;
#39913 = DIRECTION('center_axis',(-0.0989489060815945,0.7036366654692,0.703636665469218)) ;
#39914 = DIRECTION('ref_axis',(-2.16195710140876E-14,-0.707106781186558,0.707106781186537)) ;
#39915 = DIRECTION('center_axis',(-0.0989489060815945,0.7036366654692,0.703636665469218)) ;
#39916 = DIRECTION('ref_axis',(-2.16195710140876E-14,-0.707106781186558,0.707106781186537)) ;
#39917 = DIRECTION('center_axis',(0.0914824783325312,-0.92000541566125,-0.381078720623584)) ;
#39918 = DIRECTION('ref_axis',(0.995806686138498,0.0845187893148329,0.0350088288095578)) ;
#39919 = DIRECTION('',(-0.0914824783325312,0.92000541566125,0.381078720623584)) ;
#39920 = DIRECTION('center_axis',(-0.0989489060816096,0.995092515289535,-6.26465533084806E-14)) ;
#39921 = DIRECTION('ref_axis',(-1.0510404701705E-14,6.19317310614961E-14,
1.)) ;
#39922 = DIRECTION('center_axis',(-0.0989489060816096,0.995092515289535,-6.26465533084806E-14)) ;
#39923 = DIRECTION('ref_axis',(-1.0510404701705E-14,6.19317310614961E-14,
1.)) ;
#39924 = DIRECTION('center_axis',(0.0914824783325252,-0.920005415661246,0.381078720623595)) ;
#39925 = DIRECTION('ref_axis',(0.995806686138499,0.084518789314827,-0.0350088288095565)) ;
#39926 = DIRECTION('',(-0.0914824783325252,0.920005415661247,-0.381078720623595)) ;
#39927 = DIRECTION('center_axis',(-0.0989489060816214,0.703636665469211,-0.703636665469204)) ;
#39928 = DIRECTION('ref_axis',(4.14909719684307E-14,0.707106781186547,0.707106781186548)) ;
#39929 = DIRECTION('center_axis',(-0.0989489060816214,0.703636665469211,-0.703636665469204)) ;
#39930 = DIRECTION('ref_axis',(4.14909719684307E-14,0.707106781186547,0.707106781186548)) ;
#39931 = DIRECTION('center_axis',(0.0914824783325302,-0.381078720623583,0.920005415661251)) ;
#39932 = DIRECTION('ref_axis',(0.995806686138499,0.0350088288095573,-0.084518789314832)) ;
#39933 = DIRECTION('',(-0.0914824783325301,0.381078720623583,-0.920005415661251)) ;
#39934 = DIRECTION('center_axis',(-0.0989489060815886,-4.14134706495869E-14,
-0.995092515289537)) ;
#39935 = DIRECTION('ref_axis',(-5.62996296610662E-14,1.,-3.60112340135734E-14)) ;
#39936 = DIRECTION('center_axis',(-0.0989489060815886,-4.14134706495869E-14,
-0.995092515289537)) ;
#39937 = DIRECTION('ref_axis',(-5.62996296610662E-14,1.,-3.60112340135734E-14)) ;
#39938 = DIRECTION('center_axis',(0.0914824783325264,0.381078720623592,0.920005415661248)) ;
#39939 = DIRECTION('ref_axis',(0.995806686138499,-0.0350088288095566,-0.0845187893148281)) ;
#39940 = DIRECTION('',(-0.0914824783325264,-0.381078720623592,-0.920005415661248)) ;
#39941 = DIRECTION('center_axis',(-0.0989489060815706,-0.703636665469207,
-0.703636665469215)) ;
#39942 = DIRECTION('ref_axis',(-8.51150321748982E-14,0.707106781186557,-0.707106781186538)) ;
#39943 = DIRECTION('center_axis',(-0.0989489060815706,-0.703636665469207,
-0.703636665469215)) ;
#39944 = DIRECTION('ref_axis',(-8.51150321748982E-14,0.707106781186557,-0.707106781186538)) ;
#39945 = DIRECTION('center_axis',(0.0914824783325249,0.920005415661252,0.381078720623582)) ;
#39946 = DIRECTION('ref_axis',(0.995806686138499,-0.0845187893148272,-0.0350088288095551)) ;
#39947 = DIRECTION('',(-0.0914824783325248,-0.920005415661252,-0.381078720623582)) ;
#39948 = DIRECTION('center_axis',(-0.098948906081608,-0.995092515289535,5.73229448909532E-14)) ;
#39949 = DIRECTION('ref_axis',(3.14349845605419E-15,-5.7904791925403E-14,
-1.)) ;
#39950 = DIRECTION('center_axis',(-0.098948906081608,-0.995092515289535,5.73229448909532E-14)) ;
#39951 = DIRECTION('ref_axis',(3.14349845605419E-15,-5.7904791925403E-14,
-1.)) ;
#39952 = DIRECTION('center_axis',(0.0914824783325315,0.92000541566125,-0.381078720623585)) ;
#39953 = DIRECTION('ref_axis',(0.995806686138498,-0.0845187893148331,0.035008828809558)) ;
#39954 = DIRECTION('',(-0.0914824783325315,-0.92000541566125,0.381078720623585)) ;
#39955 = DIRECTION('center_axis',(-0.098948906081596,-0.703636665469235,0.703636665469183)) ;
#39956 = DIRECTION('ref_axis',(-3.43379091551647E-14,-0.707106781186519,-0.707106781186576)) ;
#39957 = DIRECTION('center_axis',(-0.098948906081596,-0.703636665469235,0.703636665469183)) ;
#39958 = DIRECTION('ref_axis',(-3.43379091551647E-14,-0.707106781186519,-0.707106781186576)) ;
#39959 = DIRECTION('center_axis',(0.0914824783325255,0.381078720623585,-0.920005415661251)) ;
#39960 = DIRECTION('ref_axis',(0.995806686138499,-0.0350088288095557,0.0845187893148276)) ;
#39961 = DIRECTION('',(-0.0914824783325255,-0.381078720623585,0.920005415661251)) ;
#39962 = DIRECTION('center_axis',(-0.0989489060816133,0.,0.995092515289534)) ;
#39963 = DIRECTION('ref_axis',(1.96896340368161E-14,-1.,1.9600087099505E-15)) ;
#39964 = DIRECTION('center_axis',(-0.0989489060816133,0.,0.995092515289534)) ;
#39965 = DIRECTION('ref_axis',(1.96896340368161E-14,-1.,1.9600087099505E-15)) ;
#39966 = DIRECTION('center_axis',(0.09148247833253,-0.381078720623586,-0.92000541566125)) ;
#39967 = DIRECTION('ref_axis',(0.995806686138499,0.0350088288095576,0.0845187893148318)) ;
#39968 = DIRECTION('',(-0.09148247833253,0.381078720623586,0.92000541566125)) ;
#39969 = DIRECTION('center_axis',(-0.0989489060816217,0.703636665469199,0.703636665469216)) ;
#39970 = DIRECTION('ref_axis',(2.92377432927906E-14,-0.707106781186554,0.707106781186541)) ;
#39971 = DIRECTION('center_axis',(-0.0989489060816217,0.703636665469199,0.703636665469216)) ;
#39972 = DIRECTION('ref_axis',(2.92377432927906E-14,-0.707106781186554,0.707106781186541)) ;
#39973 = DIRECTION('center_axis',(0.0914824783325255,-0.920005415661251,-0.381078720623585)) ;
#39974 = DIRECTION('ref_axis',(0.995806686138499,0.0845187893148277,0.0350088288095557)) ;
#39975 = DIRECTION('',(-0.0914824783325255,0.920005415661251,0.381078720623585)) ;
#39976 = DIRECTION('center_axis',(-0.098948906081604,0.995092515289535,-6.1284671714818E-14)) ;
#39977 = DIRECTION('ref_axis',(-9.02953893244136E-15,6.07114869754513E-14,
1.)) ;
#39978 = DIRECTION('center_axis',(-0.098948906081604,0.995092515289535,-6.1284671714818E-14)) ;
#39979 = DIRECTION('ref_axis',(-9.02953893244136E-15,6.07114869754513E-14,
1.)) ;
#39980 = DIRECTION('center_axis',(0.0914824783325252,-0.920005415661246,0.381078720623595)) ;
#39981 = DIRECTION('ref_axis',(0.995806686138499,0.084518789314827,-0.0350088288095565)) ;
#39982 = DIRECTION('',(-0.0914824783325252,0.920005415661247,-0.381078720623595)) ;
#39983 = DIRECTION('center_axis',(-0.0989489060816196,0.703636665469237,-0.703636665469178)) ;
#39984 = DIRECTION('ref_axis',(4.05660991233678E-14,0.707106781186521,0.707106781186574)) ;
#39985 = DIRECTION('center_axis',(-0.0989489060816196,0.703636665469237,-0.703636665469178)) ;
#39986 = DIRECTION('ref_axis',(4.05660991233678E-14,0.707106781186521,0.707106781186574)) ;
#39987 = DIRECTION('center_axis',(0.0914824783325311,-0.381078720623588,0.920005415661249)) ;
#39988 = DIRECTION('ref_axis',(0.995806686138498,0.0350088288095581,-0.0845187893148327)) ;
#39989 = DIRECTION('',(-0.0914824783325311,0.381078720623588,-0.920005415661249)) ;
#39990 = DIRECTION('center_axis',(-0.0989489060816132,0.,-0.995092515289534)) ;
#39991 = DIRECTION('ref_axis',(4.56021119560253E-15,1.,-4.86493808675064E-16)) ;
#39992 = DIRECTION('center_axis',(-0.0989489060816132,0.,-0.995092515289534)) ;
#39993 = DIRECTION('ref_axis',(4.56021119560253E-15,1.,-4.86493808675064E-16)) ;
#39994 = DIRECTION('center_axis',(0.0914824783325254,0.381078720623588,0.92000541566125)) ;
#39995 = DIRECTION('ref_axis',(0.995806686138499,-0.0350088288095559,-0.0845187893148274)) ;
#39996 = DIRECTION('',(-0.0914824783325254,-0.381078720623588,-0.92000541566125)) ;
#39997 = DIRECTION('center_axis',(-0.098948906081596,-0.7036366654692,-0.703636665469218)) ;
#39998 = DIRECTION('ref_axis',(-2.07588511987394E-14,0.707106781186558,-0.707106781186537)) ;
#39999 = DIRECTION('center_axis',(-0.098948906081596,-0.7036366654692,-0.703636665469218)) ;
#40000 = DIRECTION('ref_axis',(-2.07588511987394E-14,0.707106781186558,-0.707106781186537)) ;
#40001 = DIRECTION('center_axis',(0.0914824783325313,0.92000541566125,0.381078720623585)) ;
#40002 = DIRECTION('ref_axis',(0.995806686138498,-0.084518789314833,-0.0350088288095579)) ;
#40003 = DIRECTION('',(-0.0914824783325313,-0.92000541566125,-0.381078720623585)) ;
#40004 = DIRECTION('center_axis',(-0.098948906081607,-0.995092515289535,4.78824082194844E-14)) ;
#40005 = DIRECTION('ref_axis',(-1.56693775079845E-14,-4.65096100222067E-14,
-1.)) ;
#40006 = DIRECTION('center_axis',(-0.098948906081607,-0.995092515289535,4.78824082194844E-14)) ;
#40007 = DIRECTION('ref_axis',(-1.56693775079845E-14,-4.65096100222067E-14,
-1.)) ;
#40008 = DIRECTION('center_axis',(0.091482478332525,0.920005415661252,-0.381078720623582)) ;
#40009 = DIRECTION('ref_axis',(0.995806686138499,-0.0845187893148272,0.0350088288095552)) ;
#40010 = DIRECTION('',(-0.091482478332525,-0.920005415661252,0.381078720623582)) ;
#40011 = DIRECTION('center_axis',(-0.098948906081588,-0.703636665469236,0.703636665469183)) ;
#40012 = DIRECTION('ref_axis',(-3.72408337497862E-14,-0.707106781186518,-0.707106781186577)) ;
#40013 = DIRECTION('center_axis',(-0.098948906081588,-0.703636665469236,0.703636665469183)) ;
#40014 = DIRECTION('ref_axis',(-3.72408337497862E-14,-0.707106781186518,-0.707106781186577)) ;
#40015 = DIRECTION('center_axis',(0.0914824783325255,0.381078720623585,-0.920005415661251)) ;
#40016 = DIRECTION('ref_axis',(0.995806686138499,-0.0350088288095557,0.0845187893148276)) ;
#40017 = DIRECTION('',(-0.0914824783325255,-0.381078720623585,0.920005415661251)) ;
#40018 = DIRECTION('center_axis',(-0.0989489060816109,0.,0.995092515289535)) ;
#40019 = DIRECTION('ref_axis',(1.3953283963098E-14,-1.,1.3953283963098E-15)) ;
#40020 = DIRECTION('center_axis',(-0.0989489060816109,0.,0.995092515289535)) ;
#40021 = DIRECTION('ref_axis',(1.3953283963098E-14,-1.,1.3953283963098E-15)) ;
#40022 = DIRECTION('center_axis',(0.09148247833253,-0.381078720623586,-0.92000541566125)) ;
#40023 = DIRECTION('ref_axis',(0.995806686138499,0.0350088288095575,0.0845187893148318)) ;
#40024 = DIRECTION('',(-0.09148247833253,0.381078720623586,0.92000541566125)) ;
#40025 = DIRECTION('center_axis',(-0.0989489060816199,0.7036366654692,0.703636665469215)) ;
#40026 = DIRECTION('ref_axis',(2.45438799519476E-14,-0.707106781186553,0.707106781186542)) ;
#40027 = DIRECTION('center_axis',(-0.0989489060816199,0.7036366654692,0.703636665469215)) ;
#40028 = DIRECTION('ref_axis',(2.45438799519476E-14,-0.707106781186553,0.707106781186542)) ;
#40029 = DIRECTION('center_axis',(0.0914824783325255,-0.920005415661251,-0.381078720623585)) ;
#40030 = DIRECTION('ref_axis',(0.995806686138499,0.0845187893148277,0.0350088288095557)) ;
#40031 = DIRECTION('',(-0.0914824783325255,0.920005415661251,0.381078720623585)) ;
#40032 = DIRECTION('center_axis',(-0.0989489060816096,0.995092515289535,-6.40084349021432E-14)) ;
#40033 = DIRECTION('ref_axis',(4.3891364496947E-15,6.47517913260685E-14,1.)) ;
#40034 = DIRECTION('center_axis',(-0.0989489060816096,0.995092515289535,-6.40084349021432E-14)) ;
#40035 = DIRECTION('ref_axis',(4.3891364496947E-15,6.47517913260685E-14,1.)) ;
#40036 = DIRECTION('center_axis',(0.091482478332531,-0.920005415661246,0.381078720623595)) ;
#40037 = DIRECTION('ref_axis',(0.995806686138498,0.0845187893148323,-0.0350088288095587)) ;
#40038 = DIRECTION('',(-0.0914824783325309,0.920005415661246,-0.381078720623595)) ;
#40039 = DIRECTION('center_axis',(-0.098948906081595,0.703636665469237,-0.703636665469181)) ;
#40040 = DIRECTION('ref_axis',(-3.42791022112591E-14,0.707106781186517,0.707106781186578)) ;
#40041 = DIRECTION('center_axis',(-0.098948906081595,0.703636665469237,-0.703636665469181)) ;
#40042 = DIRECTION('ref_axis',(-3.42791022112591E-14,0.707106781186517,0.707106781186578)) ;
#40043 = DIRECTION('center_axis',(0.0914824783325254,-0.381078720623588,0.920005415661249)) ;
#40044 = DIRECTION('ref_axis',(0.995806686138499,0.0350088288095559,-0.0845187893148274)) ;
#40045 = DIRECTION('',(-0.0914824783325254,0.381078720623588,-0.920005415661249)) ;
#40046 = DIRECTION('center_axis',(-0.0989489060816109,0.,-0.995092515289535)) ;
#40047 = DIRECTION('ref_axis',(1.38784387617634E-14,1.,-1.37327579234513E-15)) ;
#40048 = DIRECTION('center_axis',(-0.0989489060816109,0.,-0.995092515289535)) ;
#40049 = DIRECTION('ref_axis',(1.38784387617634E-14,1.,-1.37327579234513E-15)) ;
#40050 = DIRECTION('center_axis',(0.0914824783325254,0.381078720623587,0.92000541566125)) ;
#40051 = DIRECTION('ref_axis',(0.995806686138499,-0.0350088288095559,-0.0845187893148275)) ;
#40052 = DIRECTION('',(-0.0914824783325254,-0.381078720623587,-0.92000541566125)) ;
#40053 = DIRECTION('center_axis',(-0.0989489060815934,-0.7036366654692,-0.703636665469219)) ;
#40054 = DIRECTION('ref_axis',(-2.68052742494152E-14,0.707106781186559,-0.707106781186536)) ;
#40055 = DIRECTION('center_axis',(-0.0989489060815934,-0.7036366654692,-0.703636665469219)) ;
#40056 = DIRECTION('ref_axis',(-2.68052742494152E-14,0.707106781186559,-0.707106781186536)) ;
#40057 = DIRECTION('center_axis',(0.0914824783325306,0.920005415661252,0.381078720623582)) ;
#40058 = DIRECTION('ref_axis',(0.995806686138498,-0.0845187893148324,-0.0350088288095574)) ;
#40059 = DIRECTION('',(-0.0914824783325306,-0.920005415661251,-0.381078720623582)) ;
#40060 = DIRECTION('center_axis',(-0.0989489060816092,-0.995092515289535,
5.41347933480892E-14)) ;
#40061 = DIRECTION('ref_axis',(-8.53235295214711E-15,-5.35470637298399E-14,
-1.)) ;
#40062 = DIRECTION('center_axis',(-0.0989489060816092,-0.995092515289535,
5.41347933480892E-14)) ;
#40063 = DIRECTION('ref_axis',(-8.53235295214711E-15,-5.35470637298399E-14,
-1.)) ;
#40064 = DIRECTION('center_axis',(0.0914824783325257,0.92000541566125,-0.381078720623585)) ;
#40065 = DIRECTION('ref_axis',(0.995806686138499,-0.0845187893148278,0.0350088288095558)) ;
#40066 = DIRECTION('',(-0.0914824783325257,-0.92000541566125,0.381078720623585)) ;
#40067 = DIRECTION('center_axis',(-0.0989489060816219,-0.703636665469235,
0.703636665469179)) ;
#40068 = DIRECTION('ref_axis',(4.37042514936123E-14,-0.707106781186522,-0.707106781186573)) ;
#40069 = DIRECTION('center_axis',(-0.0989489060816219,-0.703636665469235,
0.703636665469179)) ;
#40070 = DIRECTION('ref_axis',(4.37042514936123E-14,-0.707106781186522,-0.707106781186573)) ;
#40071 = DIRECTION('center_axis',(0.0914824783325312,0.381078720623585,-0.92000541566125)) ;
#40072 = DIRECTION('ref_axis',(0.995806686138498,-0.0350088288095579,0.0845187893148329)) ;
#40073 = DIRECTION('',(-0.0914824783325312,-0.381078720623585,0.92000541566125)) ;
#40074 = DIRECTION('center_axis',(-0.0989489060816132,-2.16674034761706E-15,
0.995092515289534)) ;
#40075 = DIRECTION('ref_axis',(4.81682331446411E-15,-1.,-1.67332485840984E-15)) ;
#40076 = DIRECTION('center_axis',(-0.0989489060816132,-2.16674034761706E-15,
0.995092515289534)) ;
#40077 = DIRECTION('ref_axis',(4.81682331446411E-15,-1.,-1.67332485840984E-15)) ;
#40078 = DIRECTION('center_axis',(0.0914824783325243,-0.381078720623586,-0.92000541566125)) ;
#40079 = DIRECTION('ref_axis',(0.995806686138499,0.0350088288095553,0.0845187893148265)) ;
#40080 = DIRECTION('',(-0.0914824783325243,0.381078720623586,0.92000541566125)) ;
#40081 = DIRECTION('center_axis',(-0.098948906081589,0.703636665469202,0.703636665469218)) ;
#40082 = DIRECTION('ref_axis',(-3.5150514198226E-14,-0.707106781186558,0.707106781186537)) ;
#40083 = DIRECTION('center_axis',(-0.098948906081589,0.703636665469202,0.703636665469218)) ;
#40084 = DIRECTION('ref_axis',(-3.5150514198226E-14,-0.707106781186558,0.707106781186537)) ;
#40085 = DIRECTION('center_axis',(0.0914824783325255,-0.920005415661251,-0.381078720623585)) ;
#40086 = DIRECTION('ref_axis',(0.995806686138499,0.0845187893148277,0.0350088288095557)) ;
#40087 = DIRECTION('',(-0.0914824783325255,0.920005415661251,0.381078720623585)) ;
#40088 = DIRECTION('center_axis',(-0.0989489060816082,0.995092515289535,-6.24763181092728E-14)) ;
#40089 = DIRECTION('ref_axis',(1.06387107611358E-15,6.29020456359414E-14,
1.)) ;
#40090 = DIRECTION('center_axis',(-0.0989489060816082,0.995092515289535,-6.24763181092728E-14)) ;
#40091 = DIRECTION('ref_axis',(1.06387107611358E-15,6.29020456359414E-14,
1.)) ;
#40092 = DIRECTION('center_axis',(0.0914824783325307,-0.920005415661247,0.381078720623594)) ;
#40093 = DIRECTION('ref_axis',(0.995806686138498,0.0845187893148321,-0.0350088288095585)) ;
#40094 = DIRECTION('',(-0.0914824783325307,0.920005415661247,-0.381078720623594)) ;
#40095 = DIRECTION('center_axis',(-0.098948906081595,0.703636665469237,-0.703636665469182)) ;
#40096 = DIRECTION('ref_axis',(-3.37712240593455E-14,0.707106781186517,0.707106781186578)) ;
#40097 = DIRECTION('center_axis',(-0.098948906081595,0.703636665469237,-0.703636665469182)) ;
#40098 = DIRECTION('ref_axis',(-3.37712240593455E-14,0.707106781186517,0.707106781186578)) ;
#40099 = DIRECTION('center_axis',(0.0914824783325255,-0.381078720623585,0.920005415661251)) ;
#40100 = DIRECTION('ref_axis',(0.995806686138499,0.0350088288095557,-0.0845187893148276)) ;
#40101 = DIRECTION('',(-0.0914824783325255,0.381078720623585,-0.92000541566125)) ;
#40102 = DIRECTION('center_axis',(-0.0989489060816132,0.,-0.995092515289534)) ;
#40103 = DIRECTION('ref_axis',(1.96468653503392E-14,1.,-1.9593404492243E-15)) ;
#40104 = DIRECTION('center_axis',(-0.0989489060816132,0.,-0.995092515289534)) ;
#40105 = DIRECTION('ref_axis',(1.96468653503392E-14,1.,-1.9593404492243E-15)) ;
#40106 = DIRECTION('center_axis',(0.0914824783325311,0.381078720623587,0.920005415661249)) ;
#40107 = DIRECTION('ref_axis',(0.995806686138498,-0.035008828809558,-0.0845187893148328)) ;
#40108 = DIRECTION('',(-0.0914824783325311,-0.381078720623587,-0.920005415661249)) ;
#40109 = DIRECTION('center_axis',(-0.09894890608162,-0.7036366654692,-0.703636665469215)) ;
#40110 = DIRECTION('ref_axis',(2.22022943673357E-14,0.707106781186553,-0.707106781186542)) ;
#40111 = DIRECTION('center_axis',(-0.09894890608162,-0.7036366654692,-0.703636665469215)) ;
#40112 = DIRECTION('ref_axis',(2.22022943673357E-14,0.707106781186553,-0.707106781186542)) ;
#40113 = DIRECTION('center_axis',(0.0914824783325253,0.920005415661251,0.381078720623584)) ;
#40114 = DIRECTION('ref_axis',(0.995806686138499,-0.0845187893148275,-0.0350088288095555)) ;
#40115 = DIRECTION('',(-0.0914824783325253,-0.920005415661251,-0.381078720623584)) ;
#40116 = DIRECTION('center_axis',(-0.0989489060816036,-0.995092515289535,
5.34538525512579E-14)) ;
#40117 = DIRECTION('ref_axis',(-8.23831823261823E-15,-5.28888269145309E-14,
-1.)) ;
#40118 = DIRECTION('center_axis',(-0.0989489060816036,-0.995092515289535,
5.34538525512579E-14)) ;
#40119 = DIRECTION('ref_axis',(-8.23831823261823E-15,-5.28888269145309E-14,
-1.)) ;
#40120 = DIRECTION('center_axis',(0.0914824783325253,0.920005415661251,-0.381078720623584)) ;
#40121 = DIRECTION('ref_axis',(0.995806686138499,-0.0845187893148275,0.0350088288095555)) ;
#40122 = DIRECTION('',(-0.0914824783325253,-0.920005415661251,0.381078720623584)) ;
#40123 = DIRECTION('center_axis',(-0.0989489060816199,-0.703636665469237,
0.703636665469178)) ;
#40124 = DIRECTION('ref_axis',(3.98336853674502E-14,-0.70710678118652,-0.707106781186575)) ;
#40125 = DIRECTION('center_axis',(-0.0989489060816199,-0.703636665469237,
0.703636665469178)) ;
#40126 = DIRECTION('ref_axis',(3.98336853674502E-14,-0.70710678118652,-0.707106781186575)) ;
#40127 = DIRECTION('center_axis',(0.0914824783325312,0.381078720623585,-0.92000541566125)) ;
#40128 = DIRECTION('ref_axis',(0.995806686138498,-0.0350088288095579,0.0845187893148329)) ;
#40129 = DIRECTION('',(-0.0914824783325312,-0.381078720623585,0.92000541566125)) ;
#40130 = DIRECTION('center_axis',(-0.0989489060816132,0.,0.995092515289534)) ;
#40131 = DIRECTION('ref_axis',(4.59228771046023E-15,-1.,4.67114247615206E-16)) ;
#40132 = DIRECTION('center_axis',(-0.0989489060816132,0.,0.995092515289534)) ;
#40133 = DIRECTION('ref_axis',(4.59228771046023E-15,-1.,4.67114247615206E-16)) ;
#40134 = DIRECTION('center_axis',(0.0914824783325254,-0.381078720623587,-0.92000541566125)) ;
#40135 = DIRECTION('ref_axis',(0.995806686138499,0.0350088288095559,0.0845187893148275)) ;
#40136 = DIRECTION('',(-0.0914824783325254,0.381078720623587,0.92000541566125)) ;
#40137 = DIRECTION('center_axis',(-0.098948906081595,0.703636665469222,0.703636665469197)) ;
#40138 = DIRECTION('ref_axis',(-2.62172048103571E-14,-0.707106781186537,0.707106781186558)) ;
#40139 = DIRECTION('center_axis',(-0.098948906081595,0.703636665469222,0.703636665469197)) ;
#40140 = DIRECTION('ref_axis',(-2.62172048103571E-14,-0.707106781186537,0.707106781186558)) ;
#40141 = DIRECTION('center_axis',(0.0914824783325306,-0.920005415661247,-0.381078720623593)) ;
#40142 = DIRECTION('ref_axis',(0.995806686138498,0.084518789314832,0.0350088288095584)) ;
#40143 = DIRECTION('',(-0.0914824783325306,0.920005415661247,0.381078720623593)) ;
#40144 = DIRECTION('center_axis',(-0.0989489060816068,0.995092515289535,-5.43976630314667E-14)) ;
#40145 = DIRECTION('ref_axis',(-1.57174922802709E-14,5.30879686109389E-14,
1.)) ;
#40146 = DIRECTION('center_axis',(-0.0989489060816068,0.995092515289535,-5.43976630314667E-14)) ;
#40147 = DIRECTION('ref_axis',(-1.57174922802709E-14,5.30879686109389E-14,
1.)) ;
#40148 = DIRECTION('center_axis',(0.0914824783325249,-0.920005415661247,0.381078720623594)) ;
#40149 = DIRECTION('ref_axis',(0.995806686138499,0.0845187893148268,-0.0350088288095563)) ;
#40150 = DIRECTION('',(-0.0914824783325249,0.920005415661247,-0.381078720623594)) ;
#40151 = DIRECTION('center_axis',(-0.0989489060815875,0.703636665469236,-0.703636665469183)) ;
#40152 = DIRECTION('ref_axis',(-3.72889485220729E-14,0.707106781186518,0.707106781186577)) ;
#40153 = DIRECTION('center_axis',(-0.0989489060815875,0.703636665469236,-0.703636665469183)) ;
#40154 = DIRECTION('ref_axis',(-3.72889485220729E-14,0.707106781186518,0.707106781186577)) ;
#40155 = DIRECTION('center_axis',(0.0914824783325255,-0.381078720623586,0.92000541566125)) ;
#40156 = DIRECTION('ref_axis',(0.995806686138499,0.0350088288095557,-0.0845187893148276)) ;
#40157 = DIRECTION('',(-0.0914824783325255,0.381078720623586,-0.92000541566125)) ;
#40158 = DIRECTION('center_axis',(-0.0989489060816132,0.,-0.995092515289534)) ;
#40159 = DIRECTION('ref_axis',(1.96094427496718E-14,1.,-1.9600087099505E-15)) ;
#40160 = DIRECTION('center_axis',(-0.0989489060816132,0.,-0.995092515289534)) ;
#40161 = DIRECTION('ref_axis',(1.96094427496718E-14,1.,-1.9600087099505E-15)) ;
#40162 = DIRECTION('center_axis',(0.0914824783325311,0.381078720623587,0.920005415661249)) ;
#40163 = DIRECTION('ref_axis',(0.995806686138498,-0.035008828809558,-0.0845187893148328)) ;
#40164 = DIRECTION('',(-0.0914824783325311,-0.381078720623587,-0.920005415661249)) ;
#40165 = DIRECTION('center_axis',(-0.0989489060816214,-0.7036366654692,-0.703636665469215)) ;
#40166 = DIRECTION('ref_axis',(2.56772501435862E-14,0.707106781186553,-0.707106781186542)) ;
#40167 = DIRECTION('center_axis',(-0.0989489060816214,-0.7036366654692,-0.703636665469215)) ;
#40168 = DIRECTION('ref_axis',(2.56772501435862E-14,0.707106781186553,-0.707106781186542)) ;
#40169 = DIRECTION('center_axis',(0.0914824783325253,0.920005415661251,0.381078720623584)) ;
#40170 = DIRECTION('ref_axis',(0.995806686138499,-0.0845187893148275,-0.0350088288095555)) ;
#40171 = DIRECTION('',(-0.0914824783325253,-0.920005415661251,-0.381078720623584)) ;
#40172 = DIRECTION('center_axis',(-0.0989489060816092,-0.995092515289535,
5.22158889147184E-14)) ;
#40173 = DIRECTION('ref_axis',(5.37281623866406E-15,-5.30144599310569E-14,
-1.)) ;
#40174 = DIRECTION('center_axis',(-0.0989489060816092,-0.995092515289535,
5.22158889147184E-14)) ;
#40175 = DIRECTION('ref_axis',(5.37281623866406E-15,-5.30144599310569E-14,
-1.)) ;
#40176 = DIRECTION('center_axis',(0.0914824783325311,0.920005415661251,-0.381078720623584)) ;
#40177 = DIRECTION('ref_axis',(0.995806686138498,-0.0845187893148328,0.0350088288095577)) ;
#40178 = DIRECTION('',(-0.0914824783325311,-0.920005415661251,0.381078720623584)) ;
#40179 = DIRECTION('center_axis',(-0.0989489060815955,-0.703636665469238,
0.70363666546918)) ;
#40180 = DIRECTION('ref_axis',(-3.43699856700224E-14,-0.707106781186516,-0.707106781186579)) ;
#40181 = DIRECTION('center_axis',(-0.0989489060815955,-0.703636665469238,
0.70363666546918)) ;
#40182 = DIRECTION('ref_axis',(-3.43699856700224E-14,-0.707106781186516,-0.707106781186579)) ;
#40183 = DIRECTION('center_axis',(0.0914824783325255,0.381078720623586,-0.92000541566125)) ;
#40184 = DIRECTION('ref_axis',(0.995806686138499,-0.0350088288095557,0.0845187893148276)) ;
#40185 = DIRECTION('',(-0.0914824783325255,-0.381078720623586,0.92000541566125)) ;
#40186 = DIRECTION('center_axis',(-0.0989489060816109,0.,0.995092515289535)) ;
#40187 = DIRECTION('ref_axis',(1.38944770191922E-14,-1.,1.3953283963098E-15)) ;
#40188 = DIRECTION('center_axis',(-0.0989489060816109,0.,0.995092515289535)) ;
#40189 = DIRECTION('ref_axis',(1.38944770191922E-14,-1.,1.3953283963098E-15)) ;
#40190 = DIRECTION('center_axis',(0.0914824783325254,-0.381078720623587,-0.92000541566125)) ;
#40191 = DIRECTION('ref_axis',(0.995806686138499,0.0350088288095558,0.0845187893148275)) ;
#40192 = DIRECTION('',(-0.0914824783325254,0.381078720623587,0.92000541566125)) ;
#40193 = DIRECTION('center_axis',(-0.0989489060815929,0.70363666546922,0.703636665469198)) ;
#40194 = DIRECTION('ref_axis',(-3.11569880984424E-14,-0.707106781186539,0.707106781186557)) ;
#40195 = DIRECTION('center_axis',(-0.0989489060815929,0.70363666546922,0.703636665469198)) ;
#40196 = DIRECTION('ref_axis',(-3.11569880984424E-14,-0.707106781186539,0.707106781186557)) ;
#40197 = DIRECTION('center_axis',(0.0914824783325306,-0.920005415661247,-0.381078720623593)) ;
#40198 = DIRECTION('ref_axis',(0.995806686138498,0.084518789314832,0.0350088288095584)) ;
#40199 = DIRECTION('',(-0.0914824783325306,0.920005415661247,0.381078720623593)) ;
#40200 = DIRECTION('center_axis',(-0.0989489060816092,0.995092515289535,-5.6858556535412E-14)) ;
#40201 = DIRECTION('ref_axis',(-1.00399491504588E-14,5.61579583871108E-14,
1.)) ;
#40202 = DIRECTION('center_axis',(-0.0989489060816092,0.995092515289535,-5.6858556535412E-14)) ;
#40203 = DIRECTION('ref_axis',(-1.00399491504588E-14,5.61579583871108E-14,
1.)) ;
#40204 = DIRECTION('center_axis',(0.0914824783325249,-0.920005415661247,0.381078720623594)) ;
#40205 = DIRECTION('ref_axis',(0.995806686138499,0.0845187893148267,-0.0350088288095562)) ;
#40206 = DIRECTION('',(-0.0914824783325249,0.920005415661247,-0.381078720623594)) ;
#40207 = DIRECTION('center_axis',(-0.0989489060816196,0.703636665469237,-0.703636665469178)) ;
#40208 = DIRECTION('ref_axis',(4.13680119948102E-14,0.707106781186521,0.707106781186574)) ;
#40209 = DIRECTION('center_axis',(-0.0989489060816196,0.703636665469237,-0.703636665469178)) ;
#40210 = DIRECTION('ref_axis',(4.13680119948102E-14,0.707106781186521,0.707106781186574)) ;
#40211 = DIRECTION('center_axis',(0.0914824783325312,-0.381078720623586,0.92000541566125)) ;
#40212 = DIRECTION('ref_axis',(0.995806686138498,0.0350088288095579,-0.0845187893148329)) ;
#40213 = DIRECTION('',(-0.0914824783325312,0.381078720623586,-0.92000541566125)) ;
#40214 = DIRECTION('center_axis',(-0.0989489060816121,2.16674034761703E-15,
-0.995092515289534)) ;
#40215 = DIRECTION('ref_axis',(1.91924480565218E-15,1.,1.95599914559329E-15)) ;
#40216 = DIRECTION('center_axis',(-0.0989489060816121,2.16674034761703E-15,
-0.995092515289534)) ;
#40217 = DIRECTION('ref_axis',(1.91924480565218E-15,1.,1.95599914559329E-15)) ;
#40218 = DIRECTION('center_axis',(0.0914824783325254,0.381078720623587,0.92000541566125)) ;
#40219 = DIRECTION('ref_axis',(0.995806686138499,-0.0350088288095558,-0.0845187893148275)) ;
#40220 = DIRECTION('',(-0.0914824783325254,-0.381078720623587,-0.92000541566125)) ;
#40221 = DIRECTION('center_axis',(-0.098948906081588,-0.703636665469202,-0.703636665469218)) ;
#40222 = DIRECTION('ref_axis',(-4.05554069517479E-14,0.707106781186558,-0.707106781186537)) ;
#40223 = DIRECTION('center_axis',(-0.098948906081588,-0.703636665469202,-0.703636665469218)) ;
#40224 = DIRECTION('ref_axis',(-4.05554069517479E-14,0.707106781186558,-0.707106781186537)) ;
#40225 = DIRECTION('center_axis',(0.0914824783325253,0.920005415661251,0.381078720623584)) ;
#40226 = DIRECTION('ref_axis',(0.995806686138499,-0.0845187893148275,-0.0350088288095555)) ;
#40227 = DIRECTION('',(-0.0914824783325253,-0.920005415661251,-0.381078720623584)) ;
#40228 = DIRECTION('center_axis',(-0.0989489060816078,-0.995092515289535,
5.47694169028358E-14)) ;
#40229 = DIRECTION('ref_axis',(1.61451791450403E-15,-5.51883120733919E-14,
-1.)) ;
#40230 = DIRECTION('center_axis',(-0.0989489060816078,-0.995092515289535,
5.47694169028358E-14)) ;
#40231 = DIRECTION('ref_axis',(1.61451791450403E-15,-5.51883120733919E-14,
-1.)) ;
#40232 = DIRECTION('center_axis',(0.091482478332531,0.920005415661251,-0.381078720623584)) ;
#40233 = DIRECTION('ref_axis',(0.995806686138498,-0.0845187893148328,0.0350088288095577)) ;
#40234 = DIRECTION('',(-0.091482478332531,-0.920005415661251,0.381078720623584)) ;
#40235 = DIRECTION('center_axis',(-0.098948906081596,-0.703636665469235,0.703636665469183)) ;
#40236 = DIRECTION('ref_axis',(-3.3343537194576E-14,-0.707106781186519,-0.707106781186576)) ;
#40237 = DIRECTION('center_axis',(-0.098948906081596,-0.703636665469235,0.703636665469183)) ;
#40238 = DIRECTION('ref_axis',(-3.3343537194576E-14,-0.707106781186519,-0.707106781186576)) ;
#40239 = DIRECTION('center_axis',(0.0914824783325255,0.381078720623586,-0.92000541566125)) ;
#40240 = DIRECTION('ref_axis',(0.995806686138499,-0.0350088288095557,0.0845187893148276)) ;
#40241 = DIRECTION('',(-0.0914824783325255,-0.381078720623586,0.92000541566125)) ;
#40242 = DIRECTION('center_axis',(-0.0989489060816109,0.,0.995092515289535)) ;
#40243 = DIRECTION('ref_axis',(1.3883784847573E-14,-1.,1.3953283963098E-15)) ;
#40244 = DIRECTION('center_axis',(-0.0989489060816109,0.,0.995092515289535)) ;
#40245 = DIRECTION('ref_axis',(1.3883784847573E-14,-1.,1.3953283963098E-15)) ;
#40246 = DIRECTION('center_axis',(0.0914824783325311,-0.381078720623587,-0.920005415661249)) ;
#40247 = DIRECTION('ref_axis',(0.995806686138498,0.035008828809558,0.0845187893148328)) ;
#40248 = DIRECTION('',(-0.0914824783325311,0.381078720623587,0.920005415661249)) ;
#40249 = DIRECTION('center_axis',(-0.0989489060816206,0.703636665469221,0.703636665469194)) ;
#40250 = DIRECTION('ref_axis',(2.08016198852161E-14,-0.707106781186532,0.707106781186563)) ;
#40251 = DIRECTION('center_axis',(-0.0989489060816206,0.703636665469221,0.703636665469194)) ;
#40252 = DIRECTION('ref_axis',(2.08016198852161E-14,-0.707106781186532,0.707106781186563)) ;
#40253 = DIRECTION('center_axis',(0.0914824783325249,-0.920005415661247,-0.381078720623594)) ;
#40254 = DIRECTION('ref_axis',(0.995806686138499,0.0845187893148267,0.0350088288095562)) ;
#40255 = DIRECTION('',(-0.0914824783325249,0.920005415661247,0.381078720623593)) ;
#40256 = DIRECTION('center_axis',(-0.0989489060816038,0.995092515289535,-5.70287917346198E-14)) ;
#40257 = DIRECTION('ref_axis',(-8.29712517652396E-15,5.64834013607711E-14,
1.)) ;
#40258 = DIRECTION('center_axis',(-0.0989489060816038,0.995092515289535,-5.70287917346198E-14)) ;
#40259 = DIRECTION('ref_axis',(-8.29712517652396E-15,5.64834013607711E-14,
1.)) ;
#40260 = DIRECTION('center_axis',(0.0914824783325249,-0.920005415661247,0.381078720623594)) ;
#40261 = DIRECTION('ref_axis',(0.995806686138499,0.0845187893148268,-0.0350088288095563)) ;
#40262 = DIRECTION('',(-0.0914824783325249,0.920005415661247,-0.381078720623594)) ;
#40263 = DIRECTION('center_axis',(-0.0989489060816196,0.703636665469236,-0.703636665469179)) ;
#40264 = DIRECTION('ref_axis',(4.1063285103662E-14,0.707106781186522,0.707106781186573)) ;
#40265 = DIRECTION('center_axis',(-0.0989489060816196,0.703636665469236,-0.703636665469179)) ;
#40266 = DIRECTION('ref_axis',(4.1063285103662E-14,0.707106781186522,0.707106781186573)) ;
#40267 = DIRECTION('center_axis',(0.0914824783325312,-0.381078720623586,0.92000541566125)) ;
#40268 = DIRECTION('ref_axis',(0.995806686138498,0.035008828809558,-0.0845187893148329)) ;
#40269 = DIRECTION('',(-0.0914824783325312,0.381078720623586,-0.92000541566125)) ;
#40270 = DIRECTION('center_axis',(-0.0989489060816132,0.,-0.995092515289534)) ;
#40271 = DIRECTION('ref_axis',(4.52813468074483E-15,1.,-4.24345561138278E-16)) ;
#40272 = DIRECTION('center_axis',(-0.0989489060816132,0.,-0.995092515289534)) ;
#40273 = DIRECTION('ref_axis',(4.52813468074483E-15,1.,-4.24345561138278E-16)) ;
#40274 = DIRECTION('center_axis',(0.0914824783325254,0.381078720623587,0.92000541566125)) ;
#40275 = DIRECTION('ref_axis',(0.995806686138499,-0.0350088288095558,-0.0845187893148275)) ;
#40276 = DIRECTION('',(-0.0914824783325254,-0.381078720623587,-0.92000541566125)) ;
#40277 = DIRECTION('center_axis',(-0.098948906081596,-0.7036366654692,-0.703636665469218)) ;
#40278 = DIRECTION('ref_axis',(-2.08123120568356E-14,0.707106781186558,-0.707106781186537)) ;
#40279 = DIRECTION('center_axis',(-0.098948906081596,-0.7036366654692,-0.703636665469218)) ;
#40280 = DIRECTION('ref_axis',(-2.08123120568356E-14,0.707106781186558,-0.707106781186537)) ;
#40281 = DIRECTION('center_axis',(0.091482478332531,0.920005415661251,0.381078720623584)) ;
#40282 = DIRECTION('ref_axis',(0.995806686138498,-0.0845187893148328,-0.0350088288095577)) ;
#40283 = DIRECTION('',(-0.091482478332531,-0.920005415661251,-0.381078720623583)) ;
#40284 = DIRECTION('center_axis',(-0.098948906081607,-0.995092515289535,4.92442898131471E-14)) ;
#40285 = DIRECTION('ref_axis',(-1.47070820622536E-14,-4.8002504484542E-14,
-1.)) ;
#40286 = DIRECTION('center_axis',(-0.098948906081607,-0.995092515289535,4.92442898131471E-14)) ;
#40287 = DIRECTION('ref_axis',(-1.47070820622536E-14,-4.8002504484542E-14,
-1.)) ;
#40288 = DIRECTION('center_axis',(0.0914824783325253,0.920005415661251,-0.381078720623584)) ;
#40289 = DIRECTION('ref_axis',(0.995806686138499,-0.0845187893148275,0.0350088288095555)) ;
#40290 = DIRECTION('',(-0.0914824783325253,-0.920005415661251,0.381078720623584)) ;
#40291 = DIRECTION('center_axis',(-0.098948906081588,-0.703636665469236,0.703636665469184)) ;
#40292 = DIRECTION('ref_axis',(-3.79197866476075E-14,-0.707106781186519,-0.707106781186576)) ;
#40293 = DIRECTION('center_axis',(-0.098948906081588,-0.703636665469236,0.703636665469184)) ;
#40294 = DIRECTION('ref_axis',(-3.79197866476075E-14,-0.707106781186519,-0.707106781186576)) ;
#40295 = DIRECTION('center_axis',(0.0914824783325255,0.381078720623586,-0.92000541566125)) ;
#40296 = DIRECTION('ref_axis',(0.995806686138499,-0.0350088288095558,0.0845187893148276)) ;
#40297 = DIRECTION('',(-0.0914824783325255,-0.381078720623586,0.92000541566125)) ;
#40298 = DIRECTION('center_axis',(-0.0989489060816109,0.,0.995092515289535)) ;
#40299 = DIRECTION('ref_axis',(1.38624005043345E-14,-1.,1.3953283963098E-15)) ;
#40300 = DIRECTION('center_axis',(-0.0989489060816109,0.,0.995092515289535)) ;
#40301 = DIRECTION('ref_axis',(1.38624005043345E-14,-1.,1.3953283963098E-15)) ;
#40302 = DIRECTION('center_axis',(0.0914824783325311,-0.381078720623587,-0.920005415661249)) ;
#40303 = DIRECTION('ref_axis',(0.995806686138498,0.035008828809558,0.0845187893148328)) ;
#40304 = DIRECTION('',(-0.0914824783325311,0.381078720623587,0.920005415661249)) ;
#40305 = DIRECTION('center_axis',(-0.0989489060816206,0.703636665469222,0.703636665469193)) ;
#40306 = DIRECTION('ref_axis',(2.07588511987391E-14,-0.707106781186531,0.707106781186564)) ;
#40307 = DIRECTION('center_axis',(-0.0989489060816206,0.703636665469222,0.703636665469193)) ;
#40308 = DIRECTION('ref_axis',(2.07588511987391E-14,-0.707106781186531,0.707106781186564)) ;
#40309 = DIRECTION('center_axis',(0.091482478332525,-0.920005415661247,-0.381078720623594)) ;
#40310 = DIRECTION('ref_axis',(0.995806686138499,0.0845187893148268,0.0350088288095563)) ;
#40311 = DIRECTION('',(-0.0914824783325249,0.920005415661247,0.381078720623594)) ;
#40312 = DIRECTION('center_axis',(-0.0989489060816092,0.995092515289535,-5.69824744925375E-14)) ;
#40313 = DIRECTION('ref_axis',(4.72059376989088E-15,5.77611158692693E-14,
1.)) ;
#40314 = DIRECTION('center_axis',(-0.0989489060816092,0.995092515289535,-5.69824744925375E-14)) ;
#40315 = DIRECTION('ref_axis',(4.72059376989088E-15,5.77611158692693E-14,
1.)) ;
#40316 = DIRECTION('center_axis',(0.0914824783325307,-0.920005415661246,0.381078720623594)) ;
#40317 = DIRECTION('ref_axis',(0.995806686138498,0.0845187893148321,-0.0350088288095585)) ;
#40318 = DIRECTION('',(-0.0914824783325307,0.920005415661246,-0.381078720623594)) ;
#40319 = DIRECTION('center_axis',(-0.0989489060815939,0.703636665469237,-0.703636665469181)) ;
#40320 = DIRECTION('ref_axis',(-3.61716165878632E-14,0.707106781186517,0.707106781186578)) ;
#40321 = DIRECTION('center_axis',(-0.0989489060815939,0.703636665469237,-0.703636665469181)) ;
#40322 = DIRECTION('ref_axis',(-3.61716165878632E-14,0.707106781186517,0.707106781186578)) ;
#40323 = DIRECTION('center_axis',(0.0914824783325254,-0.381078720623587,0.92000541566125)) ;
#40324 = DIRECTION('ref_axis',(0.995806686138499,0.0350088288095558,-0.0845187893148275)) ;
#40325 = DIRECTION('',(-0.0914824783325254,0.381078720623587,-0.92000541566125)) ;
#40326 = DIRECTION('center_axis',(-0.0989489060816109,0.,-0.995092515289535)) ;
#40327 = DIRECTION('ref_axis',(1.39800143921461E-14,1.,-1.41604447882206E-15)) ;
#40328 = DIRECTION('center_axis',(-0.0989489060816109,0.,-0.995092515289535)) ;
#40329 = DIRECTION('ref_axis',(1.39800143921461E-14,1.,-1.41604447882206E-15)) ;
#40330 = DIRECTION('center_axis',(0.0914824783325254,0.381078720623587,0.92000541566125)) ;
#40331 = DIRECTION('ref_axis',(0.995806686138499,-0.0350088288095559,-0.0845187893148275)) ;
#40332 = DIRECTION('',(-0.0914824783325254,-0.381078720623587,-0.92000541566125)) ;
#40333 = DIRECTION('center_axis',(-0.0989489060815942,-0.7036366654692,-0.703636665469218)) ;
#40334 = DIRECTION('ref_axis',(-2.50624502754804E-14,0.707106781186558,-0.707106781186537)) ;
#40335 = DIRECTION('center_axis',(-0.0989489060815942,-0.7036366654692,-0.703636665469218)) ;
#40336 = DIRECTION('ref_axis',(-2.50624502754804E-14,0.707106781186558,-0.707106781186537)) ;
#40337 = DIRECTION('center_axis',(0.0914824783325311,0.920005415661251,0.381078720623584)) ;
#40338 = DIRECTION('ref_axis',(0.995806686138498,-0.0845187893148328,-0.0350088288095577)) ;
#40339 = DIRECTION('',(-0.0914824783325311,-0.920005415661251,-0.381078720623584)) ;
#40340 = DIRECTION('center_axis',(-0.0989489060816092,-0.995092515289535,
5.34538525512579E-14)) ;
#40341 = DIRECTION('ref_axis',(-9.87956657617033E-15,-5.27197569508018E-14,
-1.)) ;
#40342 = DIRECTION('center_axis',(-0.0989489060816092,-0.995092515289535,
5.34538525512579E-14)) ;
#40343 = DIRECTION('ref_axis',(-9.87956657617033E-15,-5.27197569508018E-14,
-1.)) ;
#40344 = DIRECTION('center_axis',(0.0914824783325254,0.920005415661251,-0.381078720623584)) ;
#40345 = DIRECTION('ref_axis',(0.995806686138499,-0.0845187893148275,0.0350088288095555)) ;
#40346 = DIRECTION('',(-0.0914824783325254,-0.920005415661251,0.381078720623584)) ;
#40347 = DIRECTION('center_axis',(-0.0989489060816209,-0.703636665469237,
0.703636665469178)) ;
#40348 = DIRECTION('ref_axis',(4.24104987276851E-14,-0.707106781186521,-0.707106781186574)) ;
#40349 = DIRECTION('center_axis',(-0.0989489060816209,-0.703636665469237,
0.703636665469178)) ;
#40350 = DIRECTION('ref_axis',(4.24104987276851E-14,-0.707106781186521,-0.707106781186574)) ;
#40351 = DIRECTION('center_axis',(0.0914824783325311,0.381078720623587,-0.920005415661249)) ;
#40352 = DIRECTION('ref_axis',(0.995806686138498,-0.035008828809558,0.0845187893148328)) ;
#40353 = DIRECTION('',(-0.0914824783325311,-0.381078720623587,0.920005415661249)) ;
#40354 = DIRECTION('center_axis',(-0.0989489060816121,-2.16674034761703E-15,
0.995092515289534)) ;
#40355 = DIRECTION('ref_axis',(2.00478217860604E-15,-1.,-1.93595132380723E-15)) ;
#40356 = DIRECTION('center_axis',(-0.0989489060816121,-2.16674034761703E-15,
0.995092515289534)) ;
#40357 = DIRECTION('ref_axis',(2.00478217860604E-15,-1.,-1.93595132380723E-15)) ;
#40358 = DIRECTION('center_axis',(0.0914824783325254,-0.381078720623587,-0.92000541566125)) ;
#40359 = DIRECTION('ref_axis',(0.995806686138499,0.0350088288095559,0.0845187893148275)) ;
#40360 = DIRECTION('',(-0.0914824783325254,0.381078720623587,0.92000541566125)) ;
#40361 = DIRECTION('center_axis',(-0.0989489060815875,0.703636665469224,0.703636665469196)) ;
#40362 = DIRECTION('ref_axis',(-4.46184321670556E-14,-0.707106781186537,0.707106781186558)) ;
#40363 = DIRECTION('center_axis',(-0.0989489060815875,0.703636665469224,0.703636665469196)) ;
#40364 = DIRECTION('ref_axis',(-4.46184321670556E-14,-0.707106781186537,0.707106781186558)) ;
#40365 = DIRECTION('center_axis',(0.091482478332525,-0.920005415661247,-0.381078720623594)) ;
#40366 = DIRECTION('ref_axis',(0.995806686138499,0.0845187893148268,0.0350088288095563)) ;
#40367 = DIRECTION('',(-0.0914824783325249,0.920005415661247,0.381078720623594)) ;
#40368 = DIRECTION('center_axis',(-0.091482478332525,0.920005415661247,0.381078720623594)) ;
#40369 = DIRECTION('ref_axis',(0.995806686138499,0.0845187893148268,0.0350088288095563)) ;
#40370 = DIRECTION('center_axis',(-0.091482478332525,0.920005415661247,0.381078720623594)) ;
#40371 = DIRECTION('ref_axis',(-0.995806686138499,-0.0845187893148268,-0.0350088288095563)) ;
#40372 = DIRECTION('center_axis',(0.,0.,1.)) ;
#40373 = DIRECTION('ref_axis',(1.,0.,0.)) ;
#40374 = DIRECTION('center_axis',(0.,0.,1.)) ;
#40375 = DIRECTION('ref_axis',(1.,0.,0.)) ;
#40376 = DIRECTION('',(0.,0.,-1.)) ;
#40377 = DIRECTION('',(0.,0.,-1.)) ;
#40378 = DIRECTION('center_axis',(0.,0.,-1.)) ;
#40379 = DIRECTION('ref_axis',(1.,0.,0.)) ;
#40380 = DIRECTION('center_axis',(0.,0.,1.)) ;
#40381 = DIRECTION('ref_axis',(1.,0.,0.)) ;
#40382 = DIRECTION('center_axis',(0.,0.,1.)) ;
#40383 = DIRECTION('ref_axis',(1.,0.,0.)) ;
#40384 = DIRECTION('',(0.,0.,1.)) ;
#40385 = DIRECTION('center_axis',(0.,0.,-1.)) ;
#40386 = DIRECTION('ref_axis',(1.,0.,0.)) ;
#40387 = DIRECTION('center_axis',(0.,0.,-1.)) ;
#40388 = DIRECTION('ref_axis',(-1.,0.,0.)) ;
#40389 = DIRECTION('center_axis',(0.,0.,1.)) ;
#40390 = DIRECTION('ref_axis',(1.,0.,0.)) ;
#40391 = DIRECTION('center_axis',(0.948683298050515,0.,-0.316227766016835)) ;
#40392 = DIRECTION('ref_axis',(0.316227766016835,0.,0.948683298050515)) ;
#40393 = DIRECTION('',(-0.948683298050515,0.,0.316227766016834)) ;
#40394 = DIRECTION('center_axis',(-0.948683298050515,0.,0.316227766016835)) ;
#40395 = DIRECTION('ref_axis',(0.316227766016835,0.,0.948683298050515)) ;
#40396 = DIRECTION('center_axis',(-0.948683298050515,0.,0.316227766016835)) ;
#40397 = DIRECTION('ref_axis',(-0.316227766016835,0.,-0.948683298050515)) ;
#40398 = DIRECTION('',(0.,0.,1.)) ;
#40399 = DIRECTION('',(1.,0.,0.)) ;
#40400 = DIRECTION('',(0.,0.,1.)) ;
#40401 = DIRECTION('',(1.,0.,0.)) ;
#40402 = DIRECTION('',(0.,0.,1.)) ;
#40403 = DIRECTION('',(1.,0.,0.)) ;
#40404 = DIRECTION('',(0.,0.,1.)) ;
#40405 = DIRECTION('',(1.,0.,0.)) ;
#40406 = DIRECTION('',(0.,0.,1.)) ;
#40407 = DIRECTION('',(1.,0.,0.)) ;
#40408 = DIRECTION('',(0.,0.,1.)) ;
#40409 = DIRECTION('',(1.,0.,0.)) ;
#40410 = DIRECTION('',(0.,0.,1.)) ;
#40411 = DIRECTION('',(1.,0.,0.)) ;
#40412 = DIRECTION('',(0.,0.,1.)) ;
#40413 = DIRECTION('',(1.,0.,0.)) ;
#40414 = DIRECTION('',(0.,0.,1.)) ;
#40415 = DIRECTION('',(1.,0.,0.)) ;
#40416 = DIRECTION('',(0.,0.,1.)) ;
#40417 = DIRECTION('',(1.,0.,0.)) ;
#40418 = DIRECTION('',(0.,0.,1.)) ;
#40419 = DIRECTION('',(1.,0.,0.)) ;
#40420 = DIRECTION('',(0.,0.,1.)) ;
#40421 = DIRECTION('',(1.,0.,0.)) ;
#40422 = DIRECTION('',(0.,0.,1.)) ;
#40423 = DIRECTION('',(1.,0.,0.)) ;
#40424 = DIRECTION('',(0.,0.,1.)) ;
#40425 = DIRECTION('',(1.,0.,0.)) ;
#40426 = DIRECTION('axis',(0.,0.,1.)) ;
#40427 = DIRECTION('refdir',(1.,0.,0.)) ;
#40428 = DIRECTION('axis',(0.,0.,1.)) ;
#40429 = DIRECTION('refdir',(1.,0.,0.)) ;
#40430 = DIRECTION('center_axis',(6.12323399573676E-17,0.,1.)) ;
#40431 = DIRECTION('ref_axis',(1.,0.,0.)) ;
#40432 = DIRECTION('center_axis',(-1.22464679914735E-16,1.,0.)) ;
#40433 = DIRECTION('ref_axis',(-1.,-1.22464679914735E-16,0.)) ;
#40434 = DIRECTION('center_axis',(6.12323399573677E-17,0.,1.)) ;
#40435 = DIRECTION('ref_axis',(1.,0.,0.)) ;
#40436 = DIRECTION('center_axis',(-0.998052578482889,0.,0.0623782861551806)) ;
#40437 = DIRECTION('ref_axis',(0.0623782861551814,0.,0.998052578482889)) ;
#40438 = DIRECTION('center_axis',(0.,0.,-1.)) ;
#40439 = DIRECTION('ref_axis',(1.,0.,0.)) ;
#40440 = DIRECTION('center_axis',(0.,0.,-1.)) ;
#40441 = DIRECTION('ref_axis',(1.,0.,0.)) ;
#40442 = DIRECTION('center_axis',(-0.68469763905129,0.,0.728827238155648)) ;
#40443 = DIRECTION('ref_axis',(0.728827238155648,0.,0.68469763905129)) ;
#40444 = DIRECTION('center_axis',(0.998052578482889,0.,-0.0623782861551806)) ;
#40445 = DIRECTION('ref_axis',(0.0623782861551806,0.,0.998052578482889)) ;
#40446 = DIRECTION('center_axis',(0.,0.,1.)) ;
#40447 = DIRECTION('ref_axis',(-1.,0.,0.)) ;
#40448 = DIRECTION('center_axis',(0.,0.,1.)) ;
#40449 = DIRECTION('ref_axis',(1.,0.,0.)) ;
#40450 = DIRECTION('center_axis',(0.,0.,-1.)) ;
#40451 = DIRECTION('ref_axis',(1.,0.,0.)) ;
#40452 = DIRECTION('center_axis',(0.,0.,-1.)) ;
#40453 = DIRECTION('ref_axis',(1.,0.,0.)) ;
#40454 = DIRECTION('center_axis',(0.,0.,-1.)) ;
#40455 = DIRECTION('ref_axis',(1.,0.,0.)) ;
#40456 = DIRECTION('center_axis',(0.,0.,-1.)) ;
#40457 = DIRECTION('ref_axis',(1.,0.,0.)) ;
#40458 = DIRECTION('center_axis',(-0.68469763905129,0.,0.728827238155648)) ;
#40459 = DIRECTION('ref_axis',(0.728827238155648,0.,0.68469763905129)) ;
#40460 = DIRECTION('center_axis',(0.,0.,-1.)) ;
#40461 = DIRECTION('ref_axis',(1.,0.,0.)) ;
#40462 = DIRECTION('',(0.,0.,1.)) ;
#40463 = DIRECTION('center_axis',(0.,0.,-1.)) ;
#40464 = DIRECTION('ref_axis',(1.,0.,0.)) ;
#40465 = DIRECTION('center_axis',(0.998052578482889,0.,-0.0623782861551805)) ;
#40466 = DIRECTION('ref_axis',(0.0623782861551805,0.,0.998052578482889)) ;
#40467 = DIRECTION('center_axis',(0.998052578482889,0.,-0.0623782861551805)) ;
#40468 = DIRECTION('ref_axis',(0.0623782861551805,0.,0.998052578482889)) ;
#40469 = DIRECTION('center_axis',(-0.998052578482889,0.,0.0623782861551805)) ;
#40470 = DIRECTION('ref_axis',(0.0623782861551806,0.,0.998052578482889)) ;
#40471 = DIRECTION('center_axis',(0.998052578482889,0.,-0.0623782861551805)) ;
#40472 = DIRECTION('ref_axis',(0.0623782861551805,0.,0.998052578482889)) ;
#40473 = DIRECTION('center_axis',(-0.998052578482889,0.,0.0623782861551805)) ;
#40474 = DIRECTION('ref_axis',(0.0623782861551805,0.,0.998052578482889)) ;
#40475 = DIRECTION('center_axis',(0.998052578482889,0.,-0.0623782861551805)) ;
#40476 = DIRECTION('ref_axis',(0.0623782861551805,0.,0.998052578482889)) ;
#40477 = DIRECTION('',(-0.998052578482889,0.,0.0623782861551805)) ;
#40478 = DIRECTION('center_axis',(-0.998052578482889,0.,0.0623782861551805)) ;
#40479 = DIRECTION('ref_axis',(0.0623782861551805,0.,0.998052578482889)) ;
#40480 = DIRECTION('center_axis',(-0.998052578482889,0.,0.0623782861551805)) ;
#40481 = DIRECTION('ref_axis',(0.0623782861551805,0.,0.998052578482889)) ;
#40482 = DIRECTION('center_axis',(0.998052578482889,0.,-0.0623782861551806)) ;
#40483 = DIRECTION('ref_axis',(0.0623782861551806,0.,0.998052578482889)) ;
#40484 = DIRECTION('center_axis',(-0.998052578482889,0.,0.0623782861551806)) ;
#40485 = DIRECTION('ref_axis',(0.0623782861551814,0.,0.998052578482889)) ;
#40486 = DIRECTION('',(0.998052578482889,0.,-0.0623782861551806)) ;
#40487 = DIRECTION('center_axis',(-0.998052578482889,0.,0.0623782861551806)) ;
#40488 = DIRECTION('ref_axis',(0.0623782861551814,0.,0.998052578482889)) ;
#40489 = DIRECTION('center_axis',(0.,0.,-1.)) ;
#40490 = DIRECTION('ref_axis',(1.,0.,0.)) ;
#40491 = DIRECTION('',(0.,0.,-1.)) ;
#40492 = DIRECTION('center_axis',(0.,0.,-1.)) ;
#40493 = DIRECTION('ref_axis',(1.,0.,0.)) ;
#40494 = DIRECTION('center_axis',(0.,0.,-1.)) ;
#40495 = DIRECTION('ref_axis',(1.,0.,0.)) ;
#40496 = DIRECTION('center_axis',(6.12323399573677E-17,0.,1.)) ;
#40497 = DIRECTION('ref_axis',(1.,0.,0.)) ;
#40498 = DIRECTION('center_axis',(-6.12323399573677E-17,7.49879891330929E-33,
1.)) ;
#40499 = DIRECTION('ref_axis',(-1.,1.22464679914735E-16,0.)) ;
#40500 = DIRECTION('center_axis',(6.12323399573677E-17,0.,1.)) ;
#40501 = DIRECTION('ref_axis',(1.,0.,0.)) ;
#40502 = DIRECTION('center_axis',(1.22464679914735E-16,-1.,0.)) ;
#40503 = DIRECTION('ref_axis',(-1.,-1.22464679914735E-16,0.)) ;
#40504 = DIRECTION('axis',(0.,0.,1.)) ;
#40505 = DIRECTION('refdir',(1.,0.,0.)) ;
#40506 = DIRECTION('center_axis',(0.,1.,0.)) ;
#40507 = DIRECTION('ref_axis',(1.,0.,0.)) ;
#40508 = DIRECTION('center_axis',(0.,1.,0.)) ;
#40509 = DIRECTION('ref_axis',(1.,0.,0.)) ;
#40510 = DIRECTION('',(0.,-1.,0.)) ;
#40511 = DIRECTION('center_axis',(0.,-1.,0.)) ;
#40512 = DIRECTION('ref_axis',(1.,0.,0.)) ;
#40513 = DIRECTION('center_axis',(0.,-1.,0.)) ;
#40514 = DIRECTION('ref_axis',(-1.,0.,0.)) ;
#40515 = DIRECTION('center_axis',(0.,-1.,0.)) ;
#40516 = DIRECTION('ref_axis',(0.,0.,-1.)) ;
#40517 = DIRECTION('',(0.,0.,1.)) ;
#40518 = DIRECTION('',(1.,0.,0.)) ;
#40519 = DIRECTION('',(0.,0.,-1.)) ;
#40520 = DIRECTION('',(-1.,0.,0.)) ;
#40521 = DIRECTION('center_axis',(0.,0.,1.)) ;
#40522 = DIRECTION('ref_axis',(1.,0.,0.)) ;
#40523 = DIRECTION('',(0.,1.,0.)) ;
#40524 = DIRECTION('',(-1.,0.,0.)) ;
#40525 = DIRECTION('',(0.,-1.,0.)) ;
#40526 = DIRECTION('',(1.,0.,0.)) ;
#40527 = DIRECTION('center_axis',(0.,0.,1.)) ;
#40528 = DIRECTION('ref_axis',(1.,0.,0.)) ;
#40529 = DIRECTION('',(0.,-1.,0.)) ;
#40530 = DIRECTION('',(-1.,0.,0.)) ;
#40531 = DIRECTION('',(0.,1.,0.)) ;
#40532 = DIRECTION('',(1.,0.,0.)) ;
#40533 = DIRECTION('center_axis',(0.,1.,0.)) ;
#40534 = DIRECTION('ref_axis',(0.,0.,1.)) ;
#40535 = DIRECTION('',(0.,0.,-1.)) ;
#40536 = DIRECTION('',(0.,0.,-1.)) ;
#40537 = DIRECTION('center_axis',(1.,0.,0.)) ;
#40538 = DIRECTION('ref_axis',(0.,0.,-1.)) ;
#40539 = DIRECTION('center_axis',(0.,-1.,0.)) ;
#40540 = DIRECTION('ref_axis',(0.,0.,-1.)) ;
#40541 = DIRECTION('',(0.,0.,-1.)) ;
#40542 = DIRECTION('center_axis',(-1.,0.,0.)) ;
#40543 = DIRECTION('ref_axis',(0.,0.,1.)) ;
#40544 = DIRECTION('center_axis',(1.,0.,0.)) ;
#40545 = DIRECTION('ref_axis',(0.,0.,-1.)) ;
#40546 = DIRECTION('center_axis',(1.,0.,0.)) ;
#40547 = DIRECTION('ref_axis',(0.,0.,-1.)) ;
#40548 = DIRECTION('center_axis',(-1.,0.,0.)) ;
#40549 = DIRECTION('ref_axis',(0.,0.,1.)) ;
#40550 = DIRECTION('',(0.,0.,1.)) ;
#40551 = DIRECTION('center_axis',(-1.,0.,0.)) ;
#40552 = DIRECTION('ref_axis',(0.,0.,-1.)) ;
#40553 = DIRECTION('center_axis',(1.,0.,0.)) ;
#40554 = DIRECTION('ref_axis',(0.,0.,-1.)) ;
#40555 = DIRECTION('',(-1.,0.,0.)) ;
#40556 = DIRECTION('',(-1.,0.,0.)) ;
#40557 = DIRECTION('center_axis',(-1.,0.,0.)) ;
#40558 = DIRECTION('ref_axis',(0.,0.,-1.)) ;
#40559 = DIRECTION('center_axis',(-1.,0.,0.)) ;
#40560 = DIRECTION('ref_axis',(0.,0.,1.)) ;
#40561 = DIRECTION('center_axis',(0.,0.,1.)) ;
#40562 = DIRECTION('ref_axis',(1.,0.,0.)) ;
#40563 = DIRECTION('',(0.,0.,1.)) ;
#40564 = DIRECTION('center_axis',(0.,0.,1.)) ;
#40565 = DIRECTION('ref_axis',(1.,0.,0.)) ;
#40566 = DIRECTION('',(0.,0.,1.)) ;
#40567 = DIRECTION('center_axis',(1.,0.,0.)) ;
#40568 = DIRECTION('ref_axis',(0.,0.,-1.)) ;
#40569 = DIRECTION('',(0.,0.,1.)) ;
#40570 = DIRECTION('center_axis',(1.,0.,0.)) ;
#40571 = DIRECTION('ref_axis',(0.,0.,-1.)) ;
#40572 = DIRECTION('center_axis',(1.,0.,0.)) ;
#40573 = DIRECTION('ref_axis',(0.,0.,-1.)) ;
#40574 = DIRECTION('center_axis',(1.,0.,0.)) ;
#40575 = DIRECTION('ref_axis',(0.,0.,-1.)) ;
#40576 = DIRECTION('',(-1.,0.,0.)) ;
#40577 = DIRECTION('',(-1.,0.,0.)) ;
#40578 = DIRECTION('center_axis',(-1.,0.,0.)) ;
#40579 = DIRECTION('ref_axis',(0.,0.,-1.)) ;
#40580 = DIRECTION('center_axis',(-1.,0.,0.)) ;
#40581 = DIRECTION('ref_axis',(0.,0.,1.)) ;
#40582 = DIRECTION('center_axis',(1.,0.,0.)) ;
#40583 = DIRECTION('ref_axis',(0.,0.,-1.)) ;
#40584 = DIRECTION('center_axis',(0.,0.,1.)) ;
#40585 = DIRECTION('ref_axis',(6.12323399573677E-17,1.,0.)) ;
#40586 = DIRECTION('',(0.,0.,1.)) ;
#40587 = DIRECTION('',(0.,0.,1.)) ;
#40588 = DIRECTION('',(0.,0.,1.)) ;
#40589 = DIRECTION('center_axis',(0.,0.,-1.)) ;
#40590 = DIRECTION('ref_axis',(1.,0.,0.)) ;
#40591 = DIRECTION('',(0.,0.,-1.)) ;
#40592 = DIRECTION('',(0.,0.,1.)) ;
#40593 = DIRECTION('',(0.,0.,-1.)) ;
#40594 = DIRECTION('center_axis',(0.,0.,1.)) ;
#40595 = DIRECTION('ref_axis',(1.,0.,0.)) ;
#40596 = DIRECTION('',(0.,0.,1.)) ;
#40597 = DIRECTION('center_axis',(0.,0.,1.)) ;
#40598 = DIRECTION('ref_axis',(1.,0.,0.)) ;
#40599 = DIRECTION('center_axis',(0.,0.,1.)) ;
#40600 = DIRECTION('ref_axis',(1.,0.,0.)) ;
#40601 = DIRECTION('center_axis',(0.,0.,-1.)) ;
#40602 = DIRECTION('ref_axis',(1.,0.,0.)) ;
#40603 = DIRECTION('center_axis',(0.,0.,-1.)) ;
#40604 = DIRECTION('ref_axis',(-1.,0.,0.)) ;
#40605 = DIRECTION('center_axis',(0.,0.,-1.)) ;
#40606 = DIRECTION('ref_axis',(1.,0.,0.)) ;
#40607 = DIRECTION('center_axis',(0.,0.,1.)) ;
#40608 = DIRECTION('ref_axis',(1.,0.,0.)) ;
#40609 = DIRECTION('center_axis',(0.,0.,1.)) ;
#40610 = DIRECTION('ref_axis',(6.12323399573677E-17,1.,0.)) ;
#40611 = DIRECTION('center_axis',(0.,0.,1.)) ;
#40612 = DIRECTION('ref_axis',(1.,0.,0.)) ;
#40613 = DIRECTION('',(0.,0.,1.)) ;
#40614 = DIRECTION('axis',(0.,0.,1.)) ;
#40615 = DIRECTION('refdir',(1.,0.,0.)) ;
#40616 = DIRECTION('center_axis',(1.,0.,0.)) ;
#40617 = DIRECTION('ref_axis',(0.,0.,-1.)) ;
#40618 = DIRECTION('center_axis',(1.,0.,0.)) ;
#40619 = DIRECTION('ref_axis',(0.,0.,-1.)) ;
#40620 = DIRECTION('',(1.,0.,0.)) ;
#40621 = DIRECTION('center_axis',(-1.,0.,0.)) ;
#40622 = DIRECTION('ref_axis',(0.,0.,-1.)) ;
#40623 = DIRECTION('center_axis',(1.,0.,0.)) ;
#40624 = DIRECTION('ref_axis',(0.,0.,-1.)) ;
#40625 = DIRECTION('center_axis',(1.,0.,0.)) ;
#40626 = DIRECTION('ref_axis',(0.,0.,-1.)) ;
#40627 = DIRECTION('',(-1.,0.,0.)) ;
#40628 = DIRECTION('center_axis',(-1.,0.,0.)) ;
#40629 = DIRECTION('ref_axis',(0.,0.,-1.)) ;
#40630 = DIRECTION('center_axis',(-1.,0.,0.)) ;
#40631 = DIRECTION('ref_axis',(0.,0.,1.)) ;
#40632 = DIRECTION('center_axis',(1.,0.,0.)) ;
#40633 = DIRECTION('ref_axis',(0.,0.,-1.)) ;
#40634 = DIRECTION('axis',(0.,0.,1.)) ;
#40635 = DIRECTION('refdir',(1.,0.,0.)) ;
#40636 = DIRECTION('center_axis',(0.998052578482889,0.,-0.0623782861551805)) ;
#40637 = DIRECTION('ref_axis',(-0.0623782861551805,1.22464679914735E-16,-0.998052578482889)) ;
#40638 = DIRECTION('',(0.998052578482889,0.,-0.0623782861551805)) ;
#40639 = DIRECTION('center_axis',(0.998052578482889,0.,-0.0623782861551805)) ;
#40640 = DIRECTION('ref_axis',(0.0623782861551805,0.,0.998052578482889)) ;
#40641 = DIRECTION('',(-0.998052578482889,0.,0.0623782861551805)) ;
#40642 = DIRECTION('center_axis',(-0.998052578482889,0.,0.0623782861551805)) ;
#40643 = DIRECTION('ref_axis',(0.0623782861551805,0.,0.998052578482889)) ;
#40644 = DIRECTION('center_axis',(0.998052578482889,0.,-0.0623782861551805)) ;
#40645 = DIRECTION('ref_axis',(-0.0623782861551805,0.,-0.998052578482889)) ;
#40646 = DIRECTION('',(0.,-1.,0.)) ;
#40647 = DIRECTION('',(-0.0623782861551805,0.,-0.998052578482889)) ;
#40648 = DIRECTION('',(0.,1.,0.)) ;
#40649 = DIRECTION('',(-0.0623782861551805,0.,-0.998052578482889)) ;
#40650 = DIRECTION('',(0.,-1.,0.)) ;
#40651 = DIRECTION('center_axis',(0.0623782861551805,0.,0.998052578482889)) ;
#40652 = DIRECTION('ref_axis',(0.998052578482889,0.,-0.0623782861551805)) ;
#40653 = DIRECTION('',(0.,1.,0.)) ;
#40654 = DIRECTION('',(-0.998052578482889,0.,0.0623782861551805)) ;
#40655 = DIRECTION('center_axis',(0.0623782861551805,0.,0.998052578482889)) ;
#40656 = DIRECTION('ref_axis',(0.998052578482889,0.,-0.0623782861551805)) ;
#40657 = DIRECTION('',(0.998052578482889,0.,-0.0623782861551805)) ;
#40658 = DIRECTION('',(0.,1.,0.)) ;
#40659 = DIRECTION('center_axis',(0.0623782861551805,0.,0.998052578482889)) ;
#40660 = DIRECTION('ref_axis',(0.998052578482889,0.,-0.0623782861551805)) ;
#40661 = DIRECTION('',(0.,-1.,0.)) ;
#40662 = DIRECTION('',(-0.998052578482889,0.,0.0623782861551805)) ;
#40663 = DIRECTION('',(0.998052578482889,0.,-0.0623782861551805)) ;
#40664 = DIRECTION('center_axis',(0.,1.,0.)) ;
#40665 = DIRECTION('ref_axis',(0.0623782861551805,0.,0.998052578482889)) ;
#40666 = DIRECTION('',(-0.0623782861551805,0.,-0.998052578482889)) ;
#40667 = DIRECTION('center_axis',(0.,-1.,0.)) ;
#40668 = DIRECTION('ref_axis',(-0.0623782861551805,0.,-0.998052578482889)) ;
#40669 = DIRECTION('',(-0.0623782861551805,0.,-0.998052578482889)) ;
#40670 = DIRECTION('center_axis',(-0.998052578482889,0.,0.0623782861551805)) ;
#40671 = DIRECTION('ref_axis',(0.0623782861551805,0.,0.998052578482889)) ;
#40672 = DIRECTION('center_axis',(0.0623782861551805,0.,0.998052578482889)) ;
#40673 = DIRECTION('ref_axis',(0.998052578482889,0.,-0.0623782861551805)) ;
#40674 = DIRECTION('',(0.,1.,0.)) ;
#40675 = DIRECTION('',(-0.998052578482889,0.,0.0623782861551805)) ;
#40676 = DIRECTION('',(0.,-1.,0.)) ;
#40677 = DIRECTION('',(0.998052578482889,0.,-0.0623782861551805)) ;
#40678 = DIRECTION('center_axis',(0.0623782861551805,0.,0.998052578482889)) ;
#40679 = DIRECTION('ref_axis',(0.998052578482889,0.,-0.0623782861551805)) ;
#40680 = DIRECTION('',(0.,-1.,0.)) ;
#40681 = DIRECTION('',(-0.998052578482889,0.,0.0623782861551805)) ;
#40682 = DIRECTION('',(0.,1.,0.)) ;
#40683 = DIRECTION('',(0.998052578482889,0.,-0.0623782861551805)) ;
#40684 = DIRECTION('center_axis',(0.,1.,0.)) ;
#40685 = DIRECTION('ref_axis',(0.0623782861551805,0.,0.998052578482889)) ;
#40686 = DIRECTION('',(-0.0623782861551805,0.,-0.998052578482889)) ;
#40687 = DIRECTION('',(-0.0623782861551805,0.,-0.998052578482889)) ;
#40688 = DIRECTION('center_axis',(0.998052578482889,0.,-0.0623782861551805)) ;
#40689 = DIRECTION('ref_axis',(-0.0623782861551805,0.,-0.998052578482889)) ;
#40690 = DIRECTION('',(-0.0623782861551805,0.,-0.998052578482889)) ;
#40691 = DIRECTION('center_axis',(0.,-1.,0.)) ;
#40692 = DIRECTION('ref_axis',(-0.0623782861551805,0.,-0.998052578482889)) ;
#40693 = DIRECTION('',(-0.0623782861551805,0.,-0.998052578482889)) ;
#40694 = DIRECTION('center_axis',(-0.998052578482889,0.,0.0623782861551805)) ;
#40695 = DIRECTION('ref_axis',(0.0623782861551805,0.,0.998052578482889)) ;
#40696 = DIRECTION('axis',(0.,0.,1.)) ;
#40697 = DIRECTION('refdir',(1.,0.,0.)) ;
#40698 = DIRECTION('center_axis',(0.,1.,0.)) ;
#40699 = DIRECTION('ref_axis',(0.,0.,1.)) ;
#40700 = DIRECTION('',(-0.0623782861551789,0.,-0.998052578482889)) ;
#40701 = DIRECTION('',(-0.998052578482889,0.,0.0623782861551789)) ;
#40702 = DIRECTION('',(0.,0.,-1.)) ;
#40703 = DIRECTION('',(1.,0.,0.)) ;
#40704 = DIRECTION('',(0.,0.,-1.)) ;
#40705 = DIRECTION('',(-1.,0.,0.)) ;
#40706 = DIRECTION('center_axis',(-1.,0.,0.)) ;
#40707 = DIRECTION('ref_axis',(0.,0.,1.)) ;
#40708 = DIRECTION('center_axis',(1.,0.,0.)) ;
#40709 = DIRECTION('ref_axis',(0.,0.,1.)) ;
#40710 = DIRECTION('',(0.,0.,-1.)) ;
#40711 = DIRECTION('',(0.,1.,0.)) ;
#40712 = DIRECTION('center_axis',(0.,0.,1.)) ;
#40713 = DIRECTION('ref_axis',(1.,0.,0.)) ;
#40714 = DIRECTION('',(-1.,0.,0.)) ;
#40715 = DIRECTION('',(0.,-1.,0.)) ;
#40716 = DIRECTION('center_axis',(0.,0.,1.)) ;
#40717 = DIRECTION('ref_axis',(1.,0.,0.)) ;
#40718 = DIRECTION('',(0.,1.,0.)) ;
#40719 = DIRECTION('',(0.,1.,0.)) ;
#40720 = DIRECTION('',(1.,0.,0.)) ;
#40721 = DIRECTION('center_axis',(1.,0.,0.)) ;
#40722 = DIRECTION('ref_axis',(0.,0.,-1.)) ;
#40723 = DIRECTION('',(0.,0.,-1.)) ;
#40724 = DIRECTION('center_axis',(0.,-1.,0.)) ;
#40725 = DIRECTION('ref_axis',(0.,0.,-1.)) ;
#40726 = DIRECTION('',(0.0623782861551789,0.,0.998052578482889)) ;
#40727 = DIRECTION('',(0.998052578482889,0.,-0.0623782861551789)) ;
#40728 = DIRECTION('center_axis',(-0.998052578482889,0.,0.0623782861551789)) ;
#40729 = DIRECTION('ref_axis',(-0.0623782861551789,0.,-0.998052578482889)) ;
#40730 = DIRECTION('center_axis',(-0.998052578482889,0.,0.0623782861551789)) ;
#40731 = DIRECTION('ref_axis',(0.0623782861551789,0.,0.998052578482889)) ;
#40732 = DIRECTION('center_axis',(-0.998052578482889,0.,0.0623782861551789)) ;
#40733 = DIRECTION('ref_axis',(0.0623782861551789,0.,0.998052578482889)) ;
#40734 = DIRECTION('center_axis',(0.998052578482889,0.,-0.0623782861551789)) ;
#40735 = DIRECTION('ref_axis',(0.0623782861551792,0.,0.998052578482889)) ;
#40736 = DIRECTION('center_axis',(0.998052578482889,0.,-0.0623782861551792)) ;
#40737 = DIRECTION('ref_axis',(0.0623782861551792,0.,0.998052578482889)) ;
#40738 = DIRECTION('',(0.998052578482889,0.,-0.0623782861551792)) ;
#40739 = DIRECTION('center_axis',(-0.998052578482889,0.,0.0623782861551789)) ;
#40740 = DIRECTION('ref_axis',(0.0623782861551792,0.,0.998052578482889)) ;
#40741 = DIRECTION('center_axis',(0.998052578482889,0.,-0.0623782861551789)) ;
#40742 = DIRECTION('ref_axis',(0.0623782861551789,0.,0.998052578482889)) ;
#40743 = DIRECTION('center_axis',(0.998052578482889,0.,-0.0623782861551789)) ;
#40744 = DIRECTION('ref_axis',(0.0623782861551789,0.,0.998052578482889)) ;
#40745 = DIRECTION('',(-0.998052578482889,0.,0.0623782861551789)) ;
#40746 = DIRECTION('center_axis',(0.998052578482889,0.,-0.0623782861551789)) ;
#40747 = DIRECTION('ref_axis',(0.0623782861551789,0.,0.998052578482889)) ;
#40748 = DIRECTION('',(0.,0.,1.)) ;
#40749 = DIRECTION('',(1.,0.,0.)) ;
#40750 = DIRECTION('',(0.,0.,1.)) ;
#40751 = DIRECTION('',(1.,0.,0.)) ;
#40752 = DIRECTION('',(0.,0.,1.)) ;
#40753 = DIRECTION('',(1.,0.,0.)) ;
#40754 = DIRECTION('',(0.,0.,1.)) ;
#40755 = DIRECTION('',(1.,0.,0.)) ;
#40756 = DIRECTION('',(0.,0.,1.)) ;
#40757 = DIRECTION('',(1.,0.,0.)) ;
#40758 = DIRECTION('',(0.,0.,1.)) ;
#40759 = DIRECTION('',(1.,0.,0.)) ;
#40760 = DIRECTION('axis',(0.,0.,1.)) ;
#40761 = DIRECTION('refdir',(1.,0.,0.)) ;
#40762 = DIRECTION('axis',(0.,0.,1.)) ;
#40763 = DIRECTION('refdir',(1.,0.,0.)) ;
#40764 = DIRECTION('center_axis',(0.,0.,-1.)) ;
#40765 = DIRECTION('ref_axis',(1.,0.,0.)) ;
#40766 = DIRECTION('center_axis',(0.,0.,-1.)) ;
#40767 = DIRECTION('ref_axis',(1.,0.,0.)) ;
#40768 = DIRECTION('',(0.,0.,1.)) ;
#40769 = DIRECTION('center_axis',(0.,0.,1.)) ;
#40770 = DIRECTION('ref_axis',(1.,0.,0.)) ;
#40771 = DIRECTION('center_axis',(0.,0.,-1.)) ;
#40772 = DIRECTION('ref_axis',(1.,0.,0.)) ;
#40773 = DIRECTION('center_axis',(-0.5,-0.866025403784439,0.)) ;
#40774 = DIRECTION('ref_axis',(-0.866025403784439,0.5,0.)) ;
#40775 = DIRECTION('',(0.,0.,-1.)) ;
#40776 = DIRECTION('',(0.866025403784439,-0.5,0.)) ;
#40777 = DIRECTION('',(0.,0.,1.)) ;
#40778 = DIRECTION('',(-0.866025403784439,0.5,0.)) ;
#40779 = DIRECTION('center_axis',(0.5,0.866025403784439,0.)) ;
#40780 = DIRECTION('ref_axis',(0.866025403784439,-0.5,0.)) ;
#40781 = DIRECTION('',(0.,0.,-1.)) ;
#40782 = DIRECTION('',(-0.866025403784439,0.5,0.)) ;
#40783 = DIRECTION('',(0.,0.,1.)) ;
#40784 = DIRECTION('',(0.866025403784439,-0.5,0.)) ;
#40785 = DIRECTION('center_axis',(0.,0.,1.)) ;
#40786 = DIRECTION('ref_axis',(-1.,0.,0.)) ;
#40787 = DIRECTION('',(0.866025403784439,0.5,0.)) ;
#40788 = DIRECTION('',(0.,1.,0.)) ;
#40789 = DIRECTION('',(-0.866025403784439,-0.5,0.)) ;
#40790 = DIRECTION('',(0.,-1.,0.)) ;
#40791 = DIRECTION('center_axis',(0.5,-0.866025403784439,0.)) ;
#40792 = DIRECTION('ref_axis',(-0.866025403784439,-0.5,0.)) ;
#40793 = DIRECTION('',(0.,0.,-1.)) ;
#40794 = DIRECTION('',(-0.866025403784439,-0.5,0.)) ;
#40795 = DIRECTION('center_axis',(-0.5,0.866025403784439,0.)) ;
#40796 = DIRECTION('ref_axis',(0.866025403784439,0.5,0.)) ;
#40797 = DIRECTION('',(0.,0.,-1.)) ;
#40798 = DIRECTION('',(0.866025403784439,0.5,0.)) ;
#40799 = DIRECTION('center_axis',(1.,0.,0.)) ;
#40800 = DIRECTION('ref_axis',(0.,-1.,0.)) ;
#40801 = DIRECTION('',(0.,-1.,0.)) ;
#40802 = DIRECTION('center_axis',(-1.,0.,0.)) ;
#40803 = DIRECTION('ref_axis',(0.,1.,0.)) ;
#40804 = DIRECTION('',(0.,1.,0.)) ;
#40805 = DIRECTION('center_axis',(0.,0.,-1.)) ;
#40806 = DIRECTION('ref_axis',(1.,0.,0.)) ;
#40807 = DIRECTION('axis',(0.,0.,1.)) ;
#40808 = DIRECTION('refdir',(1.,0.,0.)) ;
#40809 = DIRECTION('center_axis',(0.,0.,1.)) ;
#40810 = DIRECTION('ref_axis',(1.,0.,0.)) ;
#40811 = DIRECTION('center_axis',(0.,0.,1.)) ;
#40812 = DIRECTION('ref_axis',(1.,0.,0.)) ;
#40813 = DIRECTION('',(0.,0.,1.)) ;
#40814 = DIRECTION('center_axis',(0.,0.,-1.)) ;
#40815 = DIRECTION('ref_axis',(1.,0.,0.)) ;
#40816 = DIRECTION('center_axis',(-0.5,0.866025403784439,0.)) ;
#40817 = DIRECTION('ref_axis',(-0.866025403784439,-0.5,0.)) ;
#40818 = DIRECTION('',(0.,0.,1.)) ;
#40819 = DIRECTION('',(0.866025403784439,0.5,0.)) ;
#40820 = DIRECTION('',(0.,0.,-1.)) ;
#40821 = DIRECTION('',(-0.866025403784439,-0.5,0.)) ;
#40822 = DIRECTION('center_axis',(0.5,-0.866025403784439,0.)) ;
#40823 = DIRECTION('ref_axis',(0.866025403784439,0.5,0.)) ;
#40824 = DIRECTION('',(0.,0.,1.)) ;
#40825 = DIRECTION('',(-0.866025403784439,-0.5,0.)) ;
#40826 = DIRECTION('',(0.,0.,-1.)) ;
#40827 = DIRECTION('',(0.866025403784439,0.5,0.)) ;
#40828 = DIRECTION('center_axis',(0.,0.,-1.)) ;
#40829 = DIRECTION('ref_axis',(-1.,0.,0.)) ;
#40830 = DIRECTION('',(0.866025403784439,-0.5,0.)) ;
#40831 = DIRECTION('',(0.,-1.,0.)) ;
#40832 = DIRECTION('',(-0.866025403784439,0.5,0.)) ;
#40833 = DIRECTION('',(0.,1.,0.)) ;
#40834 = DIRECTION('center_axis',(0.5,0.866025403784439,0.)) ;
#40835 = DIRECTION('ref_axis',(-0.866025403784439,0.5,0.)) ;
#40836 = DIRECTION('',(0.,0.,1.)) ;
#40837 = DIRECTION('',(-0.866025403784439,0.5,0.)) ;
#40838 = DIRECTION('center_axis',(-0.5,-0.866025403784439,0.)) ;
#40839 = DIRECTION('ref_axis',(0.866025403784439,-0.5,0.)) ;
#40840 = DIRECTION('',(0.,0.,1.)) ;
#40841 = DIRECTION('',(0.866025403784439,-0.5,0.)) ;
#40842 = DIRECTION('center_axis',(1.,0.,0.)) ;
#40843 = DIRECTION('ref_axis',(0.,1.,0.)) ;
#40844 = DIRECTION('',(0.,1.,0.)) ;
#40845 = DIRECTION('center_axis',(-1.,0.,0.)) ;
#40846 = DIRECTION('ref_axis',(0.,-1.,0.)) ;
#40847 = DIRECTION('',(0.,-1.,0.)) ;
#40848 = DIRECTION('center_axis',(0.,0.,1.)) ;
#40849 = DIRECTION('ref_axis',(1.,0.,0.)) ;
#40850 = DIRECTION('axis',(0.,0.,1.)) ;
#40851 = DIRECTION('refdir',(1.,0.,0.)) ;
#40852 = DIRECTION('center_axis',(0.,0.,-1.)) ;
#40853 = DIRECTION('ref_axis',(1.,0.,0.)) ;
#40854 = DIRECTION('center_axis',(0.,0.,-1.)) ;
#40855 = DIRECTION('ref_axis',(1.,0.,0.)) ;
#40856 = DIRECTION('',(0.,0.,1.)) ;
#40857 = DIRECTION('center_axis',(0.,0.,1.)) ;
#40858 = DIRECTION('ref_axis',(1.,0.,0.)) ;
#40859 = DIRECTION('center_axis',(0.,0.,-1.)) ;
#40860 = DIRECTION('ref_axis',(1.,0.,0.)) ;
#40861 = DIRECTION('center_axis',(-0.5,-0.866025403784439,0.)) ;
#40862 = DIRECTION('ref_axis',(-0.866025403784439,0.5,0.)) ;
#40863 = DIRECTION('',(0.,0.,-1.)) ;
#40864 = DIRECTION('',(0.866025403784439,-0.5,0.)) ;
#40865 = DIRECTION('',(0.,0.,1.)) ;
#40866 = DIRECTION('',(-0.866025403784439,0.5,0.)) ;
#40867 = DIRECTION('center_axis',(0.5,0.866025403784439,0.)) ;
#40868 = DIRECTION('ref_axis',(0.866025403784439,-0.5,0.)) ;
#40869 = DIRECTION('',(0.,0.,-1.)) ;
#40870 = DIRECTION('',(-0.866025403784439,0.5,0.)) ;
#40871 = DIRECTION('',(0.,0.,1.)) ;
#40872 = DIRECTION('',(0.866025403784439,-0.5,0.)) ;
#40873 = DIRECTION('center_axis',(0.,0.,1.)) ;
#40874 = DIRECTION('ref_axis',(-1.,0.,0.)) ;
#40875 = DIRECTION('',(0.866025403784439,0.5,0.)) ;
#40876 = DIRECTION('',(0.,1.,0.)) ;
#40877 = DIRECTION('',(-0.866025403784439,-0.5,0.)) ;
#40878 = DIRECTION('',(0.,-1.,0.)) ;
#40879 = DIRECTION('center_axis',(0.5,-0.866025403784439,0.)) ;
#40880 = DIRECTION('ref_axis',(-0.866025403784439,-0.5,0.)) ;
#40881 = DIRECTION('',(0.,0.,-1.)) ;
#40882 = DIRECTION('',(-0.866025403784439,-0.5,0.)) ;
#40883 = DIRECTION('center_axis',(-0.5,0.866025403784439,0.)) ;
#40884 = DIRECTION('ref_axis',(0.866025403784439,0.5,0.)) ;
#40885 = DIRECTION('',(0.,0.,-1.)) ;
#40886 = DIRECTION('',(0.866025403784439,0.5,0.)) ;
#40887 = DIRECTION('center_axis',(1.,0.,0.)) ;
#40888 = DIRECTION('ref_axis',(0.,-1.,0.)) ;
#40889 = DIRECTION('',(0.,-1.,0.)) ;
#40890 = DIRECTION('center_axis',(-1.,0.,0.)) ;
#40891 = DIRECTION('ref_axis',(0.,1.,0.)) ;
#40892 = DIRECTION('',(0.,1.,0.)) ;
#40893 = DIRECTION('center_axis',(0.,0.,-1.)) ;
#40894 = DIRECTION('ref_axis',(1.,0.,0.)) ;
#40895 = DIRECTION('axis',(0.,0.,1.)) ;
#40896 = DIRECTION('refdir',(1.,0.,0.)) ;
#40897 = DIRECTION('center_axis',(0.,1.,0.)) ;
#40898 = DIRECTION('ref_axis',(1.,0.,0.)) ;
#40899 = DIRECTION('center_axis',(0.,1.,0.)) ;
#40900 = DIRECTION('ref_axis',(1.,0.,0.)) ;
#40901 = DIRECTION('',(0.,1.,0.)) ;
#40902 = DIRECTION('center_axis',(0.,-1.,0.)) ;
#40903 = DIRECTION('ref_axis',(1.,0.,0.)) ;
#40904 = DIRECTION('center_axis',(-0.5,0.,-0.866025403784439)) ;
#40905 = DIRECTION('ref_axis',(-0.866025403784439,0.,0.5)) ;
#40906 = DIRECTION('',(0.,1.,0.)) ;
#40907 = DIRECTION('',(0.866025403784439,0.,-0.5)) ;
#40908 = DIRECTION('',(0.,-1.,0.)) ;
#40909 = DIRECTION('',(-0.866025403784439,0.,0.5)) ;
#40910 = DIRECTION('center_axis',(0.5,0.,0.866025403784439)) ;
#40911 = DIRECTION('ref_axis',(0.866025403784439,0.,-0.5)) ;
#40912 = DIRECTION('',(0.,1.,0.)) ;
#40913 = DIRECTION('',(-0.866025403784439,0.,0.5)) ;
#40914 = DIRECTION('',(0.,-1.,0.)) ;
#40915 = DIRECTION('',(0.866025403784439,0.,-0.5)) ;
#40916 = DIRECTION('center_axis',(0.,-1.,0.)) ;
#40917 = DIRECTION('ref_axis',(-1.,0.,0.)) ;
#40918 = DIRECTION('',(0.866025403784439,0.,0.5)) ;
#40919 = DIRECTION('',(0.,0.,1.)) ;
#40920 = DIRECTION('',(-0.866025403784439,0.,-0.5)) ;
#40921 = DIRECTION('',(0.,0.,-1.)) ;
#40922 = DIRECTION('center_axis',(0.5,0.,-0.866025403784439)) ;
#40923 = DIRECTION('ref_axis',(-0.866025403784439,0.,-0.5)) ;
#40924 = DIRECTION('',(0.,1.,0.)) ;
#40925 = DIRECTION('',(-0.866025403784439,0.,-0.5)) ;
#40926 = DIRECTION('center_axis',(-0.5,0.,0.866025403784439)) ;
#40927 = DIRECTION('ref_axis',(0.866025403784439,0.,0.5)) ;
#40928 = DIRECTION('',(0.,1.,0.)) ;
#40929 = DIRECTION('',(0.866025403784439,0.,0.5)) ;
#40930 = DIRECTION('center_axis',(1.,0.,0.)) ;
#40931 = DIRECTION('ref_axis',(0.,0.,-1.)) ;
#40932 = DIRECTION('',(0.,0.,-1.)) ;
#40933 = DIRECTION('center_axis',(-1.,0.,0.)) ;
#40934 = DIRECTION('ref_axis',(0.,0.,1.)) ;
#40935 = DIRECTION('',(0.,0.,1.)) ;
#40936 = DIRECTION('center_axis',(0.,1.,0.)) ;
#40937 = DIRECTION('ref_axis',(1.,0.,0.)) ;
#40938 = DIRECTION('axis',(0.,0.,1.)) ;
#40939 = DIRECTION('refdir',(1.,0.,0.)) ;
#40940 = DIRECTION('center_axis',(0.,0.,-1.)) ;
#40941 = DIRECTION('ref_axis',(-1.,0.,0.)) ;
#40942 = DIRECTION('center_axis',(0.,0.,-1.)) ;
#40943 = DIRECTION('ref_axis',(1.,0.,0.)) ;
#40944 = DIRECTION('center_axis',(0.,0.,1.)) ;
#40945 = DIRECTION('ref_axis',(1.,0.,0.)) ;
#40946 = DIRECTION('center_axis',(0.,0.,1.)) ;
#40947 = DIRECTION('ref_axis',(1.,0.,0.)) ;
#40948 = DIRECTION('center_axis',(0.,0.,1.)) ;
#40949 = DIRECTION('ref_axis',(1.,0.,0.)) ;
#40950 = DIRECTION('',(0.,0.,-1.)) ;
#40951 = DIRECTION('center_axis',(0.,0.,1.)) ;
#40952 = DIRECTION('ref_axis',(1.,0.,0.)) ;
#40953 = DIRECTION('center_axis',(0.,0.,1.)) ;
#40954 = DIRECTION('ref_axis',(1.,0.,0.)) ;
#40955 = DIRECTION('',(0.,0.,-1.)) ;
#40956 = DIRECTION('center_axis',(0.,0.,-1.)) ;
#40957 = DIRECTION('ref_axis',(1.,0.,0.)) ;
#40958 = DIRECTION('center_axis',(0.,0.,-1.)) ;
#40959 = DIRECTION('ref_axis',(-1.,0.,0.)) ;
#40960 = DIRECTION('axis',(0.,0.,1.)) ;
#40961 = DIRECTION('refdir',(1.,0.,0.)) ;
#40962 = DIRECTION('center_axis',(0.,0.,-1.)) ;
#40963 = DIRECTION('ref_axis',(-1.,0.,0.)) ;
#40964 = DIRECTION('center_axis',(0.,0.,-1.)) ;
#40965 = DIRECTION('ref_axis',(1.,0.,0.)) ;
#40966 = DIRECTION('center_axis',(0.,0.,1.)) ;
#40967 = DIRECTION('ref_axis',(1.,0.,0.)) ;
#40968 = DIRECTION('center_axis',(0.,0.,1.)) ;
#40969 = DIRECTION('ref_axis',(1.,0.,0.)) ;
#40970 = DIRECTION('center_axis',(0.,0.,1.)) ;
#40971 = DIRECTION('ref_axis',(1.,0.,0.)) ;
#40972 = DIRECTION('',(0.,0.,-1.)) ;
#40973 = DIRECTION('center_axis',(0.,0.,1.)) ;
#40974 = DIRECTION('ref_axis',(1.,0.,0.)) ;
#40975 = DIRECTION('center_axis',(0.,0.,1.)) ;
#40976 = DIRECTION('ref_axis',(1.,0.,0.)) ;
#40977 = DIRECTION('',(0.,0.,-1.)) ;
#40978 = DIRECTION('center_axis',(0.,0.,-1.)) ;
#40979 = DIRECTION('ref_axis',(1.,0.,0.)) ;
#40980 = DIRECTION('center_axis',(0.,0.,-1.)) ;
#40981 = DIRECTION('ref_axis',(-1.,0.,0.)) ;
#40982 = DIRECTION('axis',(0.,0.,1.)) ;
#40983 = DIRECTION('refdir',(1.,0.,0.)) ;
#40984 = DIRECTION('center_axis',(-0.965925826289068,0.,-0.258819045102521)) ;
#40985 = DIRECTION('ref_axis',(0.258819045102521,0.,-0.965925826289068)) ;
#40986 = DIRECTION('center_axis',(0.,0.,-1.)) ;
#40987 = DIRECTION('ref_axis',(1.,0.,0.)) ;
#40988 = DIRECTION('center_axis',(0.,0.,-1.)) ;
#40989 = DIRECTION('ref_axis',(1.,0.,0.)) ;
#40990 = DIRECTION('center_axis',(1.,0.,-2.14478618485241E-16)) ;
#40991 = DIRECTION('ref_axis',(2.14478618485241E-16,0.,1.)) ;
#40992 = DIRECTION('',(0.965925826289068,0.,0.258819045102521)) ;
#40993 = DIRECTION('center_axis',(0.866025403784437,0.,0.500000000000003)) ;
#40994 = DIRECTION('ref_axis',(0.500000000000003,0.,-0.866025403784437)) ;
#40995 = DIRECTION('center_axis',(0.965925826289068,0.,0.258819045102521)) ;
#40996 = DIRECTION('ref_axis',(0.258819045102521,0.,-0.965925826289068)) ;
#40997 = DIRECTION('center_axis',(0.866025403784437,0.,0.500000000000003)) ;
#40998 = DIRECTION('ref_axis',(0.500000000000003,0.,-0.866025403784437)) ;
#40999 = DIRECTION('center_axis',(1.,0.,-2.14478618485241E-16)) ;
#41000 = DIRECTION('ref_axis',(2.14478618485241E-16,0.,1.)) ;
#41001 = DIRECTION('center_axis',(0.,0.,1.)) ;
#41002 = DIRECTION('ref_axis',(1.,0.,0.)) ;
#41003 = DIRECTION('center_axis',(0.258819045102521,0.,-0.965925826289068)) ;
#41004 = DIRECTION('ref_axis',(0.965925826289068,0.,0.258819045102521)) ;
#41005 = DIRECTION('center_axis',(0.25881904510252,0.,0.965925826289068)) ;
#41006 = DIRECTION('ref_axis',(0.965925826289068,0.,-0.25881904510252)) ;
#41007 = DIRECTION('center_axis',(0.,0.,1.)) ;
#41008 = DIRECTION('ref_axis',(1.,0.,0.)) ;
#41009 = DIRECTION('center_axis',(-0.258819045102521,0.,0.965925826289068)) ;
#41010 = DIRECTION('ref_axis',(0.965925826289068,0.,0.258819045102521)) ;
#41011 = DIRECTION('center_axis',(0.707106781186548,0.,-0.707106781186547)) ;
#41012 = DIRECTION('ref_axis',(0.707106781186547,0.,0.707106781186548)) ;
#41013 = DIRECTION('center_axis',(0.,0.,1.)) ;
#41014 = DIRECTION('ref_axis',(1.,0.,0.)) ;
#41015 = DIRECTION('center_axis',(-0.707106781186548,0.,0.707106781186547)) ;
#41016 = DIRECTION('ref_axis',(0.707106781186547,0.,0.707106781186548)) ;
#41017 = DIRECTION('center_axis',(0.965925826289068,0.,-0.258819045102522)) ;
#41018 = DIRECTION('ref_axis',(0.258819045102522,0.,0.965925826289068)) ;
#41019 = DIRECTION('center_axis',(6.12323399573676E-17,0.,1.)) ;
#41020 = DIRECTION('ref_axis',(1.,0.,0.)) ;
#41021 = DIRECTION('center_axis',(-0.965925826289068,0.,0.258819045102522)) ;
#41022 = DIRECTION('ref_axis',(0.258819045102522,0.,0.965925826289068)) ;
#41023 = DIRECTION('center_axis',(0.965925826289068,0.,0.258819045102522)) ;
#41024 = DIRECTION('ref_axis',(0.258819045102522,0.,-0.965925826289068)) ;
#41025 = DIRECTION('center_axis',(1.22464679914735E-16,-1.,0.)) ;
#41026 = DIRECTION('ref_axis',(-1.,-1.22464679914735E-16,0.)) ;
#41027 = DIRECTION('center_axis',(0.965925826289068,0.,0.258819045102522)) ;
#41028 = DIRECTION('ref_axis',(0.258819045102522,0.,-0.965925826289068)) ;
#41029 = DIRECTION('center_axis',(0.,-7.49879891330929E-33,1.)) ;
#41030 = DIRECTION('ref_axis',(-1.,-1.22464679914735E-16,0.)) ;
#41031 = DIRECTION('center_axis',(-0.965925826289068,0.,-0.258819045102522)) ;
#41032 = DIRECTION('ref_axis',(0.258819045102522,0.,-0.965925826289068)) ;
#41033 = DIRECTION('center_axis',(-0.965925826289068,0.,-0.258819045102522)) ;
#41034 = DIRECTION('ref_axis',(0.258819045102522,0.,-0.965925826289068)) ;
#41035 = DIRECTION('center_axis',(0.707106781186548,0.,0.707106781186547)) ;
#41036 = DIRECTION('ref_axis',(0.707106781186547,0.,-0.707106781186548)) ;
#41037 = DIRECTION('center_axis',(0.707106781186548,0.,0.707106781186547)) ;
#41038 = DIRECTION('ref_axis',(0.707106781186547,0.,-0.707106781186548)) ;
#41039 = DIRECTION('center_axis',(0.,-7.49879891330929E-33,1.)) ;
#41040 = DIRECTION('ref_axis',(-1.,-1.22464679914735E-16,0.)) ;
#41041 = DIRECTION('center_axis',(-0.707106781186548,0.,-0.707106781186547)) ;
#41042 = DIRECTION('ref_axis',(0.707106781186547,0.,-0.707106781186548)) ;
#41043 = DIRECTION('center_axis',(-0.707106781186548,0.,-0.707106781186547)) ;
#41044 = DIRECTION('ref_axis',(0.707106781186547,0.,-0.707106781186548)) ;
#41045 = DIRECTION('center_axis',(0.25881904510252,0.,0.965925826289068)) ;
#41046 = DIRECTION('ref_axis',(0.965925826289068,0.,-0.25881904510252)) ;
#41047 = DIRECTION('center_axis',(0.25881904510252,0.,0.965925826289068)) ;
#41048 = DIRECTION('ref_axis',(0.965925826289068,0.,-0.25881904510252)) ;
#41049 = DIRECTION('center_axis',(0.,-7.49879891330929E-33,1.)) ;
#41050 = DIRECTION('ref_axis',(-1.,-1.22464679914735E-16,0.)) ;
#41051 = DIRECTION('center_axis',(-0.25881904510252,0.,-0.965925826289068)) ;
#41052 = DIRECTION('ref_axis',(0.965925826289068,0.,-0.25881904510252)) ;
#41053 = DIRECTION('center_axis',(-0.25881904510252,0.,-0.965925826289068)) ;
#41054 = DIRECTION('ref_axis',(0.965925826289068,0.,-0.25881904510252)) ;
#41055 = DIRECTION('center_axis',(-0.25881904510252,0.,0.965925826289068)) ;
#41056 = DIRECTION('ref_axis',(0.965925826289068,0.,0.25881904510252)) ;
#41057 = DIRECTION('center_axis',(-0.25881904510252,0.,0.965925826289068)) ;
#41058 = DIRECTION('ref_axis',(0.965925826289068,0.,0.25881904510252)) ;
#41059 = DIRECTION('center_axis',(0.,-7.49879891330929E-33,1.)) ;
#41060 = DIRECTION('ref_axis',(-1.,-1.22464679914735E-16,0.)) ;
#41061 = DIRECTION('center_axis',(0.25881904510252,0.,-0.965925826289068)) ;
#41062 = DIRECTION('ref_axis',(0.965925826289068,0.,0.25881904510252)) ;
#41063 = DIRECTION('center_axis',(0.25881904510252,0.,-0.965925826289068)) ;
#41064 = DIRECTION('ref_axis',(0.965925826289068,0.,0.25881904510252)) ;
#41065 = DIRECTION('center_axis',(-0.707106781186547,0.,0.707106781186548)) ;
#41066 = DIRECTION('ref_axis',(0.707106781186548,0.,0.707106781186547)) ;
#41067 = DIRECTION('center_axis',(-0.707106781186547,0.,0.707106781186548)) ;
#41068 = DIRECTION('ref_axis',(0.707106781186548,0.,0.707106781186547)) ;
#41069 = DIRECTION('center_axis',(0.,-7.49879891330928E-33,1.)) ;
#41070 = DIRECTION('ref_axis',(-1.,-1.22464679914735E-16,0.)) ;
#41071 = DIRECTION('center_axis',(0.707106781186547,0.,-0.707106781186548)) ;
#41072 = DIRECTION('ref_axis',(0.707106781186548,0.,0.707106781186547)) ;
#41073 = DIRECTION('center_axis',(0.707106781186547,0.,-0.707106781186548)) ;
#41074 = DIRECTION('ref_axis',(0.707106781186548,0.,0.707106781186547)) ;
#41075 = DIRECTION('center_axis',(-0.965925826289068,0.,0.258819045102521)) ;
#41076 = DIRECTION('ref_axis',(0.258819045102521,0.,0.965925826289068)) ;
#41077 = DIRECTION('center_axis',(-0.965925826289068,0.,0.258819045102521)) ;
#41078 = DIRECTION('ref_axis',(0.258819045102521,0.,0.965925826289068)) ;
#41079 = DIRECTION('center_axis',(0.,0.,1.)) ;
#41080 = DIRECTION('ref_axis',(1.,0.,0.)) ;
#41081 = DIRECTION('center_axis',(-0.707106781186547,0.,-0.707106781186548)) ;
#41082 = DIRECTION('ref_axis',(0.707106781186548,0.,-0.707106781186547)) ;
#41083 = DIRECTION('center_axis',(0.,0.,1.)) ;
#41084 = DIRECTION('ref_axis',(1.,0.,0.)) ;
#41085 = DIRECTION('center_axis',(0.707106781186547,0.,0.707106781186548)) ;
#41086 = DIRECTION('ref_axis',(0.707106781186548,0.,-0.707106781186547)) ;
#41087 = DIRECTION('center_axis',(-0.25881904510252,0.,-0.965925826289068)) ;
#41088 = DIRECTION('ref_axis',(0.965925826289068,0.,-0.25881904510252)) ;
#41089 = DIRECTION('center_axis',(0.258819045102521,0.,-0.965925826289068)) ;
#41090 = DIRECTION('ref_axis',(0.965925826289068,0.,0.258819045102521)) ;
#41091 = DIRECTION('center_axis',(1.71582894788192E-15,0.,-1.)) ;
#41092 = DIRECTION('ref_axis',(1.,0.,1.71582894788193E-15)) ;
#41093 = DIRECTION('center_axis',(1.71582894788192E-15,0.,-1.)) ;
#41094 = DIRECTION('ref_axis',(1.,0.,1.71582894788193E-15)) ;
#41095 = DIRECTION('',(-0.258819045102521,0.,0.965925826289068)) ;
#41096 = DIRECTION('center_axis',(-0.500000000000002,0.,0.866025403784438)) ;
#41097 = DIRECTION('ref_axis',(0.866025403784438,0.,0.500000000000002)) ;
#41098 = DIRECTION('center_axis',(-0.500000000000002,0.,0.866025403784438)) ;
#41099 = DIRECTION('ref_axis',(0.866025403784438,0.,0.500000000000002)) ;
#41100 = DIRECTION('center_axis',(0.707106781186548,0.,-0.707106781186547)) ;
#41101 = DIRECTION('ref_axis',(0.707106781186547,0.,0.707106781186548)) ;
#41102 = DIRECTION('',(-0.707106781186548,0.,0.707106781186547)) ;
#41103 = DIRECTION('center_axis',(-0.866025403784438,0.,0.500000000000001)) ;
#41104 = DIRECTION('ref_axis',(0.500000000000001,0.,0.866025403784438)) ;
#41105 = DIRECTION('center_axis',(-0.866025403784438,0.,0.500000000000001)) ;
#41106 = DIRECTION('ref_axis',(0.500000000000001,0.,0.866025403784438)) ;
#41107 = DIRECTION('center_axis',(0.965925826289068,0.,-0.258819045102522)) ;
#41108 = DIRECTION('ref_axis',(0.258819045102522,0.,0.965925826289068)) ;
#41109 = DIRECTION('',(-0.965925826289068,0.,0.258819045102522)) ;
#41110 = DIRECTION('center_axis',(-1.,0.,3.21717927727861E-16)) ;
#41111 = DIRECTION('ref_axis',(3.75337582349171E-16,0.,1.)) ;
#41112 = DIRECTION('center_axis',(-1.,0.,3.21717927727861E-16)) ;
#41113 = DIRECTION('ref_axis',(3.75337582349171E-16,0.,1.)) ;
#41114 = DIRECTION('center_axis',(0.965925826289068,0.,0.258819045102522)) ;
#41115 = DIRECTION('ref_axis',(0.258819045102522,0.,-0.965925826289068)) ;
#41116 = DIRECTION('',(-0.965925826289068,0.,-0.258819045102522)) ;
#41117 = DIRECTION('center_axis',(-0.866025403784437,0.,-0.500000000000002)) ;
#41118 = DIRECTION('ref_axis',(0.500000000000002,0.,-0.866025403784437)) ;
#41119 = DIRECTION('center_axis',(0.707106781186548,0.,0.707106781186547)) ;
#41120 = DIRECTION('ref_axis',(0.707106781186547,0.,-0.707106781186548)) ;
#41121 = DIRECTION('',(-0.707106781186548,0.,-0.707106781186547)) ;
#41122 = DIRECTION('center_axis',(-0.500000000000002,0.,-0.866025403784438)) ;
#41123 = DIRECTION('ref_axis',(0.866025403784438,0.,-0.500000000000002)) ;
#41124 = DIRECTION('center_axis',(0.25881904510252,0.,0.965925826289068)) ;
#41125 = DIRECTION('ref_axis',(0.965925826289068,0.,-0.25881904510252)) ;
#41126 = DIRECTION('',(-0.25881904510252,0.,-0.965925826289068)) ;
#41127 = DIRECTION('center_axis',(0.,0.,-1.)) ;
#41128 = DIRECTION('ref_axis',(1.,0.,0.)) ;
#41129 = DIRECTION('center_axis',(-0.25881904510252,0.,0.965925826289068)) ;
#41130 = DIRECTION('ref_axis',(0.965925826289068,0.,0.25881904510252)) ;
#41131 = DIRECTION('',(0.25881904510252,0.,-0.965925826289068)) ;
#41132 = DIRECTION('center_axis',(0.5,0.,-0.866025403784439)) ;
#41133 = DIRECTION('ref_axis',(0.866025403784439,0.,0.5)) ;
#41134 = DIRECTION('center_axis',(-0.707106781186547,0.,0.707106781186548)) ;
#41135 = DIRECTION('ref_axis',(0.707106781186548,0.,0.707106781186547)) ;
#41136 = DIRECTION('',(0.707106781186547,0.,-0.707106781186548)) ;
#41137 = DIRECTION('center_axis',(0.866025403784439,0.,-0.499999999999999)) ;
#41138 = DIRECTION('ref_axis',(0.499999999999999,0.,0.866025403784439)) ;
#41139 = DIRECTION('center_axis',(-0.965925826289068,0.,0.258819045102521)) ;
#41140 = DIRECTION('ref_axis',(0.258819045102521,0.,0.965925826289068)) ;
#41141 = DIRECTION('',(0.965925826289068,0.,-0.258819045102521)) ;
#41142 = DIRECTION('center_axis',(0.,0.,-1.)) ;
#41143 = DIRECTION('ref_axis',(1.,0.,0.)) ;
#41144 = DIRECTION('center_axis',(0.,0.,-1.)) ;
#41145 = DIRECTION('ref_axis',(1.,0.,0.)) ;
#41146 = DIRECTION('center_axis',(-0.707106781186547,0.,-0.707106781186548)) ;
#41147 = DIRECTION('ref_axis',(0.707106781186548,0.,-0.707106781186547)) ;
#41148 = DIRECTION('',(0.707106781186547,0.,0.707106781186548)) ;
#41149 = DIRECTION('center_axis',(0.500000000000001,0.,0.866025403784438)) ;
#41150 = DIRECTION('ref_axis',(0.866025403784438,0.,-0.500000000000001)) ;
#41151 = DIRECTION('center_axis',(0.500000000000001,0.,0.866025403784438)) ;
#41152 = DIRECTION('ref_axis',(0.866025403784438,0.,-0.500000000000001)) ;
#41153 = DIRECTION('center_axis',(-0.25881904510252,0.,-0.965925826289068)) ;
#41154 = DIRECTION('ref_axis',(0.965925826289068,0.,-0.25881904510252)) ;
#41155 = DIRECTION('',(0.25881904510252,0.,0.965925826289068)) ;
#41156 = DIRECTION('center_axis',(0.,0.,1.)) ;
#41157 = DIRECTION('ref_axis',(1.,0.,0.)) ;
#41158 = DIRECTION('center_axis',(0.,0.,1.)) ;
#41159 = DIRECTION('ref_axis',(1.,0.,0.)) ;
#41160 = DIRECTION('center_axis',(0.,0.,1.)) ;
#41161 = DIRECTION('ref_axis',(1.,0.,0.)) ;
#41162 = DIRECTION('',(0.,0.,-1.)) ;
#41163 = DIRECTION('center_axis',(0.,0.,-1.)) ;
#41164 = DIRECTION('ref_axis',(1.,0.,0.)) ;
#41165 = DIRECTION('center_axis',(0.,0.,1.)) ;
#41166 = DIRECTION('ref_axis',(1.,0.,0.)) ;
#41167 = DIRECTION('center_axis',(0.,0.,-1.)) ;
#41168 = DIRECTION('ref_axis',(-1.,0.,0.)) ;
#41169 = DIRECTION('center_axis',(0.,0.,1.)) ;
#41170 = DIRECTION('ref_axis',(1.,0.,0.)) ;
#41171 = DIRECTION('',(0.,0.,1.)) ;
#41172 = DIRECTION('',(1.,0.,0.)) ;
#41173 = DIRECTION('',(0.,0.,1.)) ;
#41174 = DIRECTION('',(1.,0.,0.)) ;
#41175 = DIRECTION('',(0.,0.,1.)) ;
#41176 = DIRECTION('',(1.,0.,0.)) ;
#41177 = DIRECTION('',(0.,0.,1.)) ;
#41178 = DIRECTION('',(1.,0.,0.)) ;
#41179 = DIRECTION('',(0.,0.,1.)) ;
#41180 = DIRECTION('',(1.,0.,0.)) ;
#41181 = DIRECTION('',(0.,0.,1.)) ;
#41182 = DIRECTION('',(1.,0.,0.)) ;
#41183 = DIRECTION('',(0.,0.,1.)) ;
#41184 = DIRECTION('',(1.,0.,0.)) ;
#41185 = DIRECTION('',(0.,0.,1.)) ;
#41186 = DIRECTION('',(1.,0.,0.)) ;
#41187 = DIRECTION('',(0.,0.,1.)) ;
#41188 = DIRECTION('',(1.,0.,0.)) ;
#41189 = DIRECTION('',(0.,0.,1.)) ;
#41190 = DIRECTION('',(1.,0.,0.)) ;
#41191 = DIRECTION('',(0.,0.,1.)) ;
#41192 = DIRECTION('',(1.,0.,0.)) ;
#41193 = DIRECTION('',(0.,0.,1.)) ;
#41194 = DIRECTION('',(1.,0.,0.)) ;
#41195 = DIRECTION('',(0.,0.,1.)) ;
#41196 = DIRECTION('',(1.,0.,0.)) ;
#41197 = DIRECTION('',(0.,0.,1.)) ;
#41198 = DIRECTION('',(1.,0.,0.)) ;
#41199 = DIRECTION('',(0.,0.,1.)) ;
#41200 = DIRECTION('',(1.,0.,0.)) ;
#41201 = DIRECTION('',(0.,0.,1.)) ;
#41202 = DIRECTION('',(1.,0.,0.)) ;
#41203 = DIRECTION('',(0.,0.,1.)) ;
#41204 = DIRECTION('',(1.,0.,0.)) ;
#41205 = DIRECTION('',(0.,0.,1.)) ;
#41206 = DIRECTION('',(1.,0.,0.)) ;
#41207 = DIRECTION('',(0.,0.,1.)) ;
#41208 = DIRECTION('',(2.22044604925031E-16,1.,0.)) ;
#41209 = DIRECTION('',(0.,0.,1.)) ;
#41210 = DIRECTION('',(2.22044604925031E-16,1.,0.)) ;
#41211 = DIRECTION('',(0.,0.,1.)) ;
#41212 = DIRECTION('',(1.,0.,0.)) ;
#41213 = DIRECTION('',(0.,0.,1.)) ;
#41214 = DIRECTION('',(1.,0.,0.)) ;
#41215 = DIRECTION('',(0.,0.,1.)) ;
#41216 = DIRECTION('',(1.,0.,0.)) ;
#41217 = DIRECTION('',(0.,0.,1.)) ;
#41218 = DIRECTION('',(1.,0.,0.)) ;
#41219 = DIRECTION('',(0.,0.,1.)) ;
#41220 = DIRECTION('',(1.,0.,0.)) ;
#41221 = DIRECTION('',(0.,0.,1.)) ;
#41222 = DIRECTION('',(1.,0.,0.)) ;
#41223 = CARTESIAN_POINT('',(0.,0.,0.)) ;
#41224 = CARTESIAN_POINT('',(0.,0.,0.)) ;
#41225 = CARTESIAN_POINT('',(0.,0.,0.)) ;
#41226 = CARTESIAN_POINT('Origin',(-4.9,56.8,112.3)) ;
#41227 = CARTESIAN_POINT('',(-4.2,56.8,111.68)) ;
#41228 = CARTESIAN_POINT('Origin',(-4.2,56.8,112.3)) ;
#41229 = CARTESIAN_POINT('',(-5.6,56.8,111.68)) ;
#41230 = CARTESIAN_POINT('',(-4.9,56.8,111.68)) ;
#41231 = CARTESIAN_POINT('Origin',(-5.6,56.8,112.3)) ;
#41232 = CARTESIAN_POINT('Origin',(-4.2,56.25,108.5)) ;
#41233 = CARTESIAN_POINT('',(-4.2,54.8394018931644,109.)) ;
#41234 = CARTESIAN_POINT('',(-4.2,54.8394018931644,110.)) ;
#41235 = CARTESIAN_POINT('',(-4.2,54.8394018931644,110.)) ;
#41236 = CARTESIAN_POINT('',(-4.2,54.5,109.)) ;
#41237 = CARTESIAN_POINT('',(-4.2,28.125,109.)) ;
#41238 = CARTESIAN_POINT('',(-4.2,54.5,107.)) ;
#41239 = CARTESIAN_POINT('',(-4.2,54.5,108.5)) ;
#41240 = CARTESIAN_POINT('',(-4.2,58.,107.)) ;
#41241 = CARTESIAN_POINT('',(-4.2,56.25,107.)) ;
#41242 = CARTESIAN_POINT('',(-4.2,58.,113.2)) ;
#41243 = CARTESIAN_POINT('',(-4.2,58.,111.6)) ;
#41244 = CARTESIAN_POINT('',(-4.2,55.6,113.2)) ;
#41245 = CARTESIAN_POINT('',(-4.2,56.8,113.2)) ;
#41246 = CARTESIAN_POINT('',(-4.2,55.6,110.)) ;
#41247 = CARTESIAN_POINT('',(-4.2,55.6,111.6)) ;
#41248 = CARTESIAN_POINT('',(-4.2,56.25,110.)) ;
#41249 = CARTESIAN_POINT('Origin',(-4.9,54.5,108.5)) ;
#41250 = CARTESIAN_POINT('',(-5.6,54.5,109.)) ;
#41251 = CARTESIAN_POINT('',(-2.45,54.5,109.)) ;
#41252 = CARTESIAN_POINT('',(-5.6,54.5,107.)) ;
#41253 = CARTESIAN_POINT('',(-5.6,54.5,108.5)) ;
#41254 = CARTESIAN_POINT('',(-4.9,54.5,107.)) ;
#41255 = CARTESIAN_POINT('Origin',(-4.9,56.8,113.2)) ;
#41256 = CARTESIAN_POINT('',(-5.6,58.,113.2)) ;
#41257 = CARTESIAN_POINT('',(-4.9,58.,113.2)) ;
#41258 = CARTESIAN_POINT('',(-5.6,55.6,113.2)) ;
#41259 = CARTESIAN_POINT('',(-5.6,56.8,113.2)) ;
#41260 = CARTESIAN_POINT('',(-4.9,55.6,113.2)) ;
#41261 = CARTESIAN_POINT('Origin',(-4.9,55.6,111.6)) ;
#41262 = CARTESIAN_POINT('',(-5.6,55.6,110.)) ;
#41263 = CARTESIAN_POINT('',(-5.6,55.6,111.6)) ;
#41264 = CARTESIAN_POINT('',(-4.9,55.6,110.)) ;
#41265 = CARTESIAN_POINT('Origin',(-4.9,56.25,110.)) ;
#41266 = CARTESIAN_POINT('',(-5.6,54.7141663557072,110.)) ;
#41267 = CARTESIAN_POINT('Origin',(0.,0.,110.)) ;
#41268 = CARTESIAN_POINT('',(-5.6,56.25,110.)) ;
#41269 = CARTESIAN_POINT('Origin',(-4.9,56.25,107.)) ;
#41270 = CARTESIAN_POINT('',(-5.6,58.,107.)) ;
#41271 = CARTESIAN_POINT('',(-5.6,56.25,107.)) ;
#41272 = CARTESIAN_POINT('',(-4.9,58.,107.)) ;
#41273 = CARTESIAN_POINT('Origin',(-5.6,56.25,108.5)) ;
#41274 = CARTESIAN_POINT('',(-5.6,54.7141663557072,109.)) ;
#41275 = CARTESIAN_POINT('',(-5.6,54.7141663557072,110.)) ;
#41276 = CARTESIAN_POINT('',(-5.6,58.,111.6)) ;
#41277 = CARTESIAN_POINT('',(-5.6,28.125,109.)) ;
#41278 = CARTESIAN_POINT('Origin',(-4.9,58.,108.5)) ;
#41279 = CARTESIAN_POINT('Origin',(0.,0.,110.)) ;
#41280 = CARTESIAN_POINT('',(-55.,-6.73555739531044E-15,111.)) ;
#41281 = CARTESIAN_POINT('Origin',(0.,0.,111.)) ;
#41282 = CARTESIAN_POINT('',(-55.,-6.73555739531044E-15,109.)) ;
#41283 = CARTESIAN_POINT('',(-55.,-6.73555739531044E-15,110.)) ;
#41284 = CARTESIAN_POINT('',(5.6,54.7141663557072,109.)) ;
#41285 = CARTESIAN_POINT('Origin',(0.,0.,109.)) ;
#41286 = CARTESIAN_POINT('',(5.6,54.7141663557072,110.)) ;
#41287 = CARTESIAN_POINT('',(5.6,54.7141663557072,110.)) ;
#41288 = CARTESIAN_POINT('',(4.2,54.8394018931644,110.)) ;
#41289 = CARTESIAN_POINT('Origin',(0.,0.,110.)) ;
#41290 = CARTESIAN_POINT('',(4.2,54.8394018931644,109.)) ;
#41291 = CARTESIAN_POINT('',(4.2,54.8394018931644,110.)) ;
#41292 = CARTESIAN_POINT('Origin',(0.,0.,109.)) ;
#41293 = CARTESIAN_POINT('Origin',(0.,0.,109.)) ;
#41294 = CARTESIAN_POINT('Origin',(4.9,56.8,112.3)) ;
#41295 = CARTESIAN_POINT('',(4.2,56.8,112.92)) ;
#41296 = CARTESIAN_POINT('Origin',(4.2,56.8,112.3)) ;
#41297 = CARTESIAN_POINT('',(5.6,56.8,112.92)) ;
#41298 = CARTESIAN_POINT('',(4.9,56.8,112.92)) ;
#41299 = CARTESIAN_POINT('Origin',(5.6,56.8,112.3)) ;
#41300 = CARTESIAN_POINT('Origin',(5.6,56.25,108.5)) ;
#41301 = CARTESIAN_POINT('',(5.6,54.5,109.)) ;
#41302 = CARTESIAN_POINT('',(5.6,28.125,109.)) ;
#41303 = CARTESIAN_POINT('',(5.6,54.5,107.)) ;
#41304 = CARTESIAN_POINT('',(5.6,54.5,108.5)) ;
#41305 = CARTESIAN_POINT('',(5.6,58.,107.)) ;
#41306 = CARTESIAN_POINT('',(5.6,56.25,107.)) ;
#41307 = CARTESIAN_POINT('',(5.6,58.,113.2)) ;
#41308 = CARTESIAN_POINT('',(5.6,58.,111.6)) ;
#41309 = CARTESIAN_POINT('',(5.6,55.6,113.2)) ;
#41310 = CARTESIAN_POINT('',(5.6,56.8,113.2)) ;
#41311 = CARTESIAN_POINT('',(5.6,55.6,110.)) ;
#41312 = CARTESIAN_POINT('',(5.6,55.6,111.6)) ;
#41313 = CARTESIAN_POINT('',(5.6,56.25,110.)) ;
#41314 = CARTESIAN_POINT('Origin',(4.9,54.5,108.5)) ;
#41315 = CARTESIAN_POINT('',(4.2,54.5,109.)) ;
#41316 = CARTESIAN_POINT('',(2.45,54.5,109.)) ;
#41317 = CARTESIAN_POINT('',(4.2,54.5,107.)) ;
#41318 = CARTESIAN_POINT('',(4.2,54.5,108.5)) ;
#41319 = CARTESIAN_POINT('',(4.9,54.5,107.)) ;
#41320 = CARTESIAN_POINT('Origin',(4.9,56.8,113.2)) ;
#41321 = CARTESIAN_POINT('',(4.2,58.,113.2)) ;
#41322 = CARTESIAN_POINT('',(4.9,58.,113.2)) ;
#41323 = CARTESIAN_POINT('',(4.2,55.6,113.2)) ;
#41324 = CARTESIAN_POINT('',(4.2,56.8,113.2)) ;
#41325 = CARTESIAN_POINT('',(4.9,55.6,113.2)) ;
#41326 = CARTESIAN_POINT('Origin',(4.9,55.6,111.6)) ;
#41327 = CARTESIAN_POINT('',(4.2,55.6,110.)) ;
#41328 = CARTESIAN_POINT('',(4.2,55.6,111.6)) ;
#41329 = CARTESIAN_POINT('',(4.9,55.6,110.)) ;
#41330 = CARTESIAN_POINT('Origin',(4.9,56.25,110.)) ;
#41331 = CARTESIAN_POINT('',(4.2,56.25,110.)) ;
#41332 = CARTESIAN_POINT('Origin',(4.9,56.25,107.)) ;
#41333 = CARTESIAN_POINT('',(4.2,58.,107.)) ;
#41334 = CARTESIAN_POINT('',(4.2,56.25,107.)) ;
#41335 = CARTESIAN_POINT('',(4.9,58.,107.)) ;
#41336 = CARTESIAN_POINT('Origin',(4.2,56.25,108.5)) ;
#41337 = CARTESIAN_POINT('',(4.2,58.,111.6)) ;
#41338 = CARTESIAN_POINT('',(4.2,28.125,109.)) ;
#41339 = CARTESIAN_POINT('Origin',(4.9,58.,108.5)) ;
#41340 = CARTESIAN_POINT('Origin',(20.7889393668845,-20.7889393668845,73.2)) ;
#41341 = CARTESIAN_POINT('',(18.5017201441464,-22.0372540500791,73.2)) ;
#41342 = CARTESIAN_POINT('',(22.0372540500791,-18.5017201441464,73.2)) ;
#41343 = CARTESIAN_POINT('Origin',(0.,0.,73.2)) ;
#41344 = CARTESIAN_POINT('',(20.8596500450031,-24.3951839509359,73.2)) ;
#41345 = CARTESIAN_POINT('',(19.0211724139181,-22.5567063198509,73.2)) ;
#41346 = CARTESIAN_POINT('',(24.3951839509359,-20.8596500450032,73.2)) ;
#41347 = CARTESIAN_POINT('',(22.6274169979695,-22.6274169979695,73.2)) ;
#41348 = CARTESIAN_POINT('',(22.5567063198509,-19.0211724139181,73.2)) ;
#41349 = CARTESIAN_POINT('Origin',(19.0211724139181,-22.5567063198509,72.6)) ;
#41350 = CARTESIAN_POINT('',(17.9177945565738,-21.4533284625066,72.)) ;
#41351 = CARTESIAN_POINT('Ctrl Pts',(17.9177945565738,-21.4533284625066,72.)) ;
#41352 = CARTESIAN_POINT('Ctrl Pts',(18.2055235988788,-21.7410575048115,72.5912312611487)) ;
#41353 = CARTESIAN_POINT('Ctrl Pts',(18.5017201441464,-22.0372540500791,73.2)) ;
#41354 = CARTESIAN_POINT('',(20.8596500450031,-24.3951839509359,72.)) ;
#41355 = CARTESIAN_POINT('',(19.0211724139181,-22.5567063198509,72.)) ;
#41356 = CARTESIAN_POINT('',(20.8596500450031,-24.3951839509359,72.6)) ;
#41357 = CARTESIAN_POINT('Origin',(22.5567063198509,-19.0211724139181,72.6)) ;
#41358 = CARTESIAN_POINT('',(21.4533284625065,-17.9177945565738,72.)) ;
#41359 = CARTESIAN_POINT('Ctrl Pts',(22.0372540500791,-18.5017201441464,73.2)) ;
#41360 = CARTESIAN_POINT('Ctrl Pts',(21.7410575071122,-18.2055236011795,72.5912312658768)) ;
#41361 = CARTESIAN_POINT('Ctrl Pts',(21.4533284625065,-17.9177945565738,72.)) ;
#41362 = CARTESIAN_POINT('',(24.3951839509359,-20.8596500450032,72.)) ;
#41363 = CARTESIAN_POINT('',(24.3951839509359,-20.8596500450032,72.6)) ;
#41364 = CARTESIAN_POINT('',(22.5567063198509,-19.0211724139181,72.)) ;
#41365 = CARTESIAN_POINT('Origin',(22.5567063198509,-19.0211724139181,72.6)) ;
#41366 = CARTESIAN_POINT('',(21.0273194971963,-17.4917855912636,72.)) ;
#41367 = CARTESIAN_POINT('',(21.6113450338214,-18.0758111278886,73.2)) ;
#41368 = CARTESIAN_POINT('Ctrl Pts',(21.0273194971963,-17.4917855912636,72.)) ;
#41369 = CARTESIAN_POINT('Ctrl Pts',(21.3150062821372,-17.7794723762045,72.5910387012431)) ;
#41370 = CARTESIAN_POINT('Ctrl Pts',(21.6113450338214,-18.0758111278886,73.2)) ;
#41371 = CARTESIAN_POINT('',(20.7182286887658,-17.1826947828331,72.)) ;
#41372 = CARTESIAN_POINT('',(22.5567063198509,-19.0211724139181,72.)) ;
#41373 = CARTESIAN_POINT('',(20.7182286887658,-17.1826947828331,73.2)) ;
#41374 = CARTESIAN_POINT('',(20.7182286887658,-17.1826947828331,72.6)) ;
#41375 = CARTESIAN_POINT('',(22.5567063198509,-19.0211724139181,73.2)) ;
#41376 = CARTESIAN_POINT('Origin',(20.7889393668845,-20.7889393668845,72.)) ;
#41377 = CARTESIAN_POINT('Origin',(0.,0.,72.)) ;
#41378 = CARTESIAN_POINT('',(22.6274169979695,-22.6274169979695,72.)) ;
#41379 = CARTESIAN_POINT('Origin',(20.7889393668845,-20.7889393668845,72.)) ;
#41380 = CARTESIAN_POINT('',(17.4917855912636,-21.0273194971963,72.)) ;
#41381 = CARTESIAN_POINT('Origin',(0.,0.,72.)) ;
#41382 = CARTESIAN_POINT('',(17.1826947828331,-20.7182286887659,72.)) ;
#41383 = CARTESIAN_POINT('',(19.0211724139181,-22.5567063198509,72.)) ;
#41384 = CARTESIAN_POINT('',(18.9504617357995,-18.9504617357995,72.)) ;
#41385 = CARTESIAN_POINT('Origin',(20.7889393668845,-20.7889393668845,73.2)) ;
#41386 = CARTESIAN_POINT('',(18.0758111278886,-21.6113450338214,73.2)) ;
#41387 = CARTESIAN_POINT('Origin',(0.,0.,73.2)) ;
#41388 = CARTESIAN_POINT('',(17.1826947828331,-20.7182286887659,73.2)) ;
#41389 = CARTESIAN_POINT('',(18.9504617357995,-18.9504617357995,73.2)) ;
#41390 = CARTESIAN_POINT('',(19.0211724139181,-22.5567063198509,73.2)) ;
#41391 = CARTESIAN_POINT('Origin',(19.0211724139181,-22.5567063198509,72.6)) ;
#41392 = CARTESIAN_POINT('Ctrl Pts',(18.0758111278886,-21.6113450338214,73.2)) ;
#41393 = CARTESIAN_POINT('Ctrl Pts',(17.7794723670287,-21.3150062729614,72.5910386823896)) ;
#41394 = CARTESIAN_POINT('Ctrl Pts',(17.4917855912636,-21.0273194971963,72.)) ;
#41395 = CARTESIAN_POINT('',(17.1826947828331,-20.7182286887659,72.6)) ;
#41396 = CARTESIAN_POINT('Origin',(18.9504617357995,-18.9504617357995,72.6)) ;
#41397 = CARTESIAN_POINT('Origin',(22.6274169979695,-22.6274169979695,72.6)) ;
#41398 = CARTESIAN_POINT('Origin',(-20.7889393668845,-20.7889393668845,73.2)) ;
#41399 = CARTESIAN_POINT('',(-22.0372540500791,-18.5017201441464,73.2)) ;
#41400 = CARTESIAN_POINT('',(-18.5017201441464,-22.0372540500791,73.2)) ;
#41401 = CARTESIAN_POINT('Origin',(0.,0.,73.2)) ;
#41402 = CARTESIAN_POINT('',(-24.3951839509359,-20.8596500450031,73.2)) ;
#41403 = CARTESIAN_POINT('',(-22.5567063198509,-19.0211724139181,73.2)) ;
#41404 = CARTESIAN_POINT('',(-20.8596500450032,-24.3951839509359,73.2)) ;
#41405 = CARTESIAN_POINT('',(-22.6274169979695,-22.6274169979695,73.2)) ;
#41406 = CARTESIAN_POINT('',(-19.0211724139181,-22.5567063198509,73.2)) ;
#41407 = CARTESIAN_POINT('Origin',(-22.5567063198509,-19.0211724139181,72.6)) ;
#41408 = CARTESIAN_POINT('',(-21.4533284625066,-17.9177945565738,72.)) ;
#41409 = CARTESIAN_POINT('Ctrl Pts',(-21.4533284625066,-17.9177945565738,
72.)) ;
#41410 = CARTESIAN_POINT('Ctrl Pts',(-21.7410575024954,-18.2055235965626,
72.591231256389)) ;
#41411 = CARTESIAN_POINT('Ctrl Pts',(-22.0372540500791,-18.5017201441464,
73.2)) ;
#41412 = CARTESIAN_POINT('',(-24.3951839509359,-20.8596500450031,72.)) ;
#41413 = CARTESIAN_POINT('',(-22.5567063198509,-19.0211724139181,72.)) ;
#41414 = CARTESIAN_POINT('',(-24.3951839509359,-20.8596500450031,72.6)) ;
#41415 = CARTESIAN_POINT('Origin',(-19.0211724139181,-22.5567063198509,72.6)) ;
#41416 = CARTESIAN_POINT('',(-17.9177945565738,-21.4533284625065,72.)) ;
#41417 = CARTESIAN_POINT('Ctrl Pts',(-18.5017201441464,-22.0372540500791,
73.2)) ;
#41418 = CARTESIAN_POINT('Ctrl Pts',(-18.2055235965626,-21.7410575024954,
72.591231256389)) ;
#41419 = CARTESIAN_POINT('Ctrl Pts',(-17.9177945565738,-21.4533284625066,
72.)) ;
#41420 = CARTESIAN_POINT('',(-20.8596500450032,-24.3951839509359,72.)) ;
#41421 = CARTESIAN_POINT('',(-20.8596500450032,-24.3951839509359,72.6)) ;
#41422 = CARTESIAN_POINT('',(-19.0211724139181,-22.5567063198509,72.)) ;
#41423 = CARTESIAN_POINT('Origin',(-19.0211724139181,-22.5567063198509,72.6)) ;
#41424 = CARTESIAN_POINT('',(-17.4917855912636,-21.0273194971963,72.)) ;
#41425 = CARTESIAN_POINT('',(-18.0758111278886,-21.6113450338214,73.2)) ;
#41426 = CARTESIAN_POINT('Ctrl Pts',(-17.4917855912636,-21.0273194971963,
72.)) ;
#41427 = CARTESIAN_POINT('Ctrl Pts',(-17.7794723741827,-21.3150062801154,
72.5910386970889)) ;
#41428 = CARTESIAN_POINT('Ctrl Pts',(-18.0758111278886,-21.6113450338214,
73.2)) ;
#41429 = CARTESIAN_POINT('',(-17.1826947828331,-20.7182286887658,72.)) ;
#41430 = CARTESIAN_POINT('',(-19.0211724139181,-22.5567063198509,72.)) ;
#41431 = CARTESIAN_POINT('',(-17.1826947828331,-20.7182286887658,73.2)) ;
#41432 = CARTESIAN_POINT('',(-17.1826947828331,-20.7182286887658,72.6)) ;
#41433 = CARTESIAN_POINT('',(-19.0211724139181,-22.5567063198509,73.2)) ;
#41434 = CARTESIAN_POINT('Origin',(-20.7889393668845,-20.7889393668845,72.)) ;
#41435 = CARTESIAN_POINT('Origin',(0.,0.,72.)) ;
#41436 = CARTESIAN_POINT('',(-22.6274169979695,-22.6274169979695,72.)) ;
#41437 = CARTESIAN_POINT('Origin',(-20.7889393668845,-20.7889393668845,72.)) ;
#41438 = CARTESIAN_POINT('',(-21.0273194971963,-17.4917855912636,72.)) ;
#41439 = CARTESIAN_POINT('Origin',(0.,0.,72.)) ;
#41440 = CARTESIAN_POINT('',(-20.7182286887659,-17.1826947828331,72.)) ;
#41441 = CARTESIAN_POINT('',(-22.5567063198509,-19.0211724139181,72.)) ;
#41442 = CARTESIAN_POINT('',(-18.9504617357995,-18.9504617357995,72.)) ;
#41443 = CARTESIAN_POINT('Origin',(-20.7889393668845,-20.7889393668845,73.2)) ;
#41444 = CARTESIAN_POINT('',(-21.6113450338214,-18.0758111278886,73.2)) ;
#41445 = CARTESIAN_POINT('Origin',(0.,0.,73.2)) ;
#41446 = CARTESIAN_POINT('',(-20.7182286887659,-17.1826947828331,73.2)) ;
#41447 = CARTESIAN_POINT('',(-18.9504617357995,-18.9504617357995,73.2)) ;
#41448 = CARTESIAN_POINT('',(-22.5567063198509,-19.0211724139181,73.2)) ;
#41449 = CARTESIAN_POINT('Origin',(-22.5567063198509,-19.0211724139181,72.6)) ;
#41450 = CARTESIAN_POINT('Ctrl Pts',(-21.6113450338214,-18.0758111278886,
73.2)) ;
#41451 = CARTESIAN_POINT('Ctrl Pts',(-21.3150062739694,-17.7794723680366,
72.5910386844606)) ;
#41452 = CARTESIAN_POINT('Ctrl Pts',(-21.0273194971963,-17.4917855912636,
72.)) ;
#41453 = CARTESIAN_POINT('',(-20.7182286887659,-17.1826947828331,72.6)) ;
#41454 = CARTESIAN_POINT('Origin',(-18.9504617357995,-18.9504617357995,72.6)) ;
#41455 = CARTESIAN_POINT('Origin',(-22.6274169979695,-22.6274169979695,72.6)) ;
#41456 = CARTESIAN_POINT('Origin',(-20.7889393668845,20.7889393668845,73.2)) ;
#41457 = CARTESIAN_POINT('',(-18.5017201441464,22.0372540500791,73.2)) ;
#41458 = CARTESIAN_POINT('',(-22.0372540500791,18.5017201441464,73.2)) ;
#41459 = CARTESIAN_POINT('Origin',(0.,0.,73.2)) ;
#41460 = CARTESIAN_POINT('',(-20.8596500450031,24.3951839509359,73.2)) ;
#41461 = CARTESIAN_POINT('',(-19.0211724139181,22.5567063198509,73.2)) ;
#41462 = CARTESIAN_POINT('',(-24.3951839509359,20.8596500450032,73.2)) ;
#41463 = CARTESIAN_POINT('',(-22.6274169979695,22.6274169979695,73.2)) ;
#41464 = CARTESIAN_POINT('',(-22.5567063198509,19.0211724139181,73.2)) ;
#41465 = CARTESIAN_POINT('Origin',(-19.0211724139181,22.5567063198509,72.6)) ;
#41466 = CARTESIAN_POINT('',(-17.9177945565738,21.4533284625066,72.)) ;
#41467 = CARTESIAN_POINT('Ctrl Pts',(-17.9177945565738,21.4533284625066,72.)) ;
#41468 = CARTESIAN_POINT('Ctrl Pts',(-18.2055235965626,21.7410575024954,72.591231256389)) ;
#41469 = CARTESIAN_POINT('Ctrl Pts',(-18.5017201441464,22.0372540500791,73.2)) ;
#41470 = CARTESIAN_POINT('',(-20.8596500450031,24.3951839509359,72.)) ;
#41471 = CARTESIAN_POINT('',(-19.0211724139181,22.5567063198509,72.)) ;
#41472 = CARTESIAN_POINT('',(-20.8596500450031,24.3951839509359,72.6)) ;
#41473 = CARTESIAN_POINT('Origin',(-22.5567063198509,19.0211724139181,72.6)) ;
#41474 = CARTESIAN_POINT('',(-21.4533284625066,17.9177945565738,72.)) ;
#41475 = CARTESIAN_POINT('Ctrl Pts',(-22.0372540500791,18.5017201441464,73.2)) ;
#41476 = CARTESIAN_POINT('Ctrl Pts',(-21.7410575025031,18.2055235965704,72.5912312564048)) ;
#41477 = CARTESIAN_POINT('Ctrl Pts',(-21.4533284625066,17.9177945565738,72.)) ;
#41478 = CARTESIAN_POINT('',(-24.3951839509359,20.8596500450032,72.)) ;
#41479 = CARTESIAN_POINT('',(-24.3951839509359,20.8596500450032,72.6)) ;
#41480 = CARTESIAN_POINT('',(-22.5567063198509,19.0211724139181,72.)) ;
#41481 = CARTESIAN_POINT('Origin',(-22.5567063198509,19.0211724139181,72.6)) ;
#41482 = CARTESIAN_POINT('',(-21.0273194971963,17.4917855912636,72.)) ;
#41483 = CARTESIAN_POINT('',(-21.6113450338214,18.0758111278886,73.2)) ;
#41484 = CARTESIAN_POINT('Ctrl Pts',(-21.0273194971963,17.4917855912636,72.)) ;
#41485 = CARTESIAN_POINT('Ctrl Pts',(-21.315006276006,17.7794723700733,72.5910386886453)) ;
#41486 = CARTESIAN_POINT('Ctrl Pts',(-21.6113450338214,18.0758111278886,73.2)) ;
#41487 = CARTESIAN_POINT('',(-20.7182286887658,17.1826947828331,72.)) ;
#41488 = CARTESIAN_POINT('',(-22.5567063198509,19.0211724139181,72.)) ;
#41489 = CARTESIAN_POINT('',(-20.7182286887658,17.1826947828331,73.2)) ;
#41490 = CARTESIAN_POINT('',(-20.7182286887658,17.1826947828331,72.6)) ;
#41491 = CARTESIAN_POINT('',(-22.5567063198509,19.0211724139181,73.2)) ;
#41492 = CARTESIAN_POINT('Origin',(-20.7889393668845,20.7889393668845,72.)) ;
#41493 = CARTESIAN_POINT('Origin',(0.,0.,72.)) ;
#41494 = CARTESIAN_POINT('',(-22.6274169979695,22.6274169979695,72.)) ;
#41495 = CARTESIAN_POINT('Origin',(-20.7889393668845,20.7889393668845,72.)) ;
#41496 = CARTESIAN_POINT('',(-17.4917855912636,21.0273194971963,72.)) ;
#41497 = CARTESIAN_POINT('Origin',(0.,0.,72.)) ;
#41498 = CARTESIAN_POINT('',(-17.1826947828331,20.7182286887658,72.)) ;
#41499 = CARTESIAN_POINT('',(-19.0211724139181,22.5567063198509,72.)) ;
#41500 = CARTESIAN_POINT('',(-18.9504617357995,18.9504617357995,72.)) ;
#41501 = CARTESIAN_POINT('Origin',(-20.7889393668845,20.7889393668845,73.2)) ;
#41502 = CARTESIAN_POINT('',(-18.0758111278886,21.6113450338214,73.2)) ;
#41503 = CARTESIAN_POINT('Origin',(0.,0.,73.2)) ;
#41504 = CARTESIAN_POINT('',(-17.1826947828331,20.7182286887658,73.2)) ;
#41505 = CARTESIAN_POINT('',(-18.9504617357995,18.9504617357995,73.2)) ;
#41506 = CARTESIAN_POINT('',(-19.0211724139181,22.5567063198509,73.2)) ;
#41507 = CARTESIAN_POINT('Origin',(-19.0211724139181,22.5567063198509,72.6)) ;
#41508 = CARTESIAN_POINT('Ctrl Pts',(-18.0758111278886,21.6113450338214,73.2)) ;
#41509 = CARTESIAN_POINT('Ctrl Pts',(-17.7794723700881,21.3150062760208,72.5910386886758)) ;
#41510 = CARTESIAN_POINT('Ctrl Pts',(-17.4917855912636,21.0273194971963,72.)) ;
#41511 = CARTESIAN_POINT('',(-17.1826947828331,20.7182286887658,72.6)) ;
#41512 = CARTESIAN_POINT('Origin',(-18.9504617357995,18.9504617357995,72.6)) ;
#41513 = CARTESIAN_POINT('Origin',(-22.6274169979695,22.6274169979695,72.6)) ;
#41514 = CARTESIAN_POINT('Origin',(20.7889393668845,20.7889393668845,73.2)) ;
#41515 = CARTESIAN_POINT('',(22.0372540500791,18.5017201441464,73.2)) ;
#41516 = CARTESIAN_POINT('',(18.5017201441464,22.0372540500791,73.2)) ;
#41517 = CARTESIAN_POINT('Origin',(0.,0.,73.2)) ;
#41518 = CARTESIAN_POINT('',(24.3951839509359,20.8596500450031,73.2)) ;
#41519 = CARTESIAN_POINT('',(22.5567063198509,19.0211724139181,73.2)) ;
#41520 = CARTESIAN_POINT('',(20.8596500450032,24.3951839509359,73.2)) ;
#41521 = CARTESIAN_POINT('',(22.6274169979695,22.6274169979695,73.2)) ;
#41522 = CARTESIAN_POINT('',(19.0211724139181,22.5567063198509,73.2)) ;
#41523 = CARTESIAN_POINT('Origin',(22.5567063198509,19.0211724139181,72.6)) ;
#41524 = CARTESIAN_POINT('',(21.4533284625066,17.9177945565738,72.)) ;
#41525 = CARTESIAN_POINT('Ctrl Pts',(21.4533284625066,17.9177945565738,72.)) ;
#41526 = CARTESIAN_POINT('Ctrl Pts',(21.7410575024954,18.2055235965626,72.591231256389)) ;
#41527 = CARTESIAN_POINT('Ctrl Pts',(22.0372540500791,18.5017201441464,73.2)) ;
#41528 = CARTESIAN_POINT('',(24.3951839509359,20.8596500450031,72.)) ;
#41529 = CARTESIAN_POINT('',(22.5567063198509,19.0211724139181,72.)) ;
#41530 = CARTESIAN_POINT('',(24.3951839509359,20.8596500450031,72.6)) ;
#41531 = CARTESIAN_POINT('Origin',(19.0211724139181,22.5567063198509,72.6)) ;
#41532 = CARTESIAN_POINT('',(17.9177945565738,21.4533284625066,72.)) ;
#41533 = CARTESIAN_POINT('Ctrl Pts',(18.5017201441464,22.0372540500791,73.2)) ;
#41534 = CARTESIAN_POINT('Ctrl Pts',(18.2055235965704,21.7410575025031,72.5912312564048)) ;
#41535 = CARTESIAN_POINT('Ctrl Pts',(17.9177945565738,21.4533284625066,72.)) ;
#41536 = CARTESIAN_POINT('',(20.8596500450032,24.3951839509359,72.)) ;
#41537 = CARTESIAN_POINT('',(20.8596500450032,24.3951839509359,72.6)) ;
#41538 = CARTESIAN_POINT('',(19.0211724139181,22.5567063198509,72.)) ;
#41539 = CARTESIAN_POINT('Origin',(19.0211724139181,22.5567063198509,72.6)) ;
#41540 = CARTESIAN_POINT('',(17.4917855912636,21.0273194971963,72.)) ;
#41541 = CARTESIAN_POINT('',(18.0758111278886,21.6113450338214,73.2)) ;
#41542 = CARTESIAN_POINT('Ctrl Pts',(17.4917855912636,21.0273194971963,72.)) ;
#41543 = CARTESIAN_POINT('Ctrl Pts',(17.7794723700733,21.315006276006,72.5910386886453)) ;
#41544 = CARTESIAN_POINT('Ctrl Pts',(18.0758111278886,21.6113450338214,73.2)) ;
#41545 = CARTESIAN_POINT('',(17.1826947828331,20.7182286887658,72.)) ;
#41546 = CARTESIAN_POINT('',(19.0211724139181,22.5567063198509,72.)) ;
#41547 = CARTESIAN_POINT('',(17.1826947828331,20.7182286887658,73.2)) ;
#41548 = CARTESIAN_POINT('',(17.1826947828331,20.7182286887658,72.6)) ;
#41549 = CARTESIAN_POINT('',(19.0211724139181,22.5567063198509,73.2)) ;
#41550 = CARTESIAN_POINT('Origin',(20.7889393668845,20.7889393668845,72.)) ;
#41551 = CARTESIAN_POINT('Origin',(0.,0.,72.)) ;
#41552 = CARTESIAN_POINT('',(22.6274169979695,22.6274169979695,72.)) ;
#41553 = CARTESIAN_POINT('Origin',(20.7889393668845,20.7889393668845,72.)) ;
#41554 = CARTESIAN_POINT('',(21.0273194971963,17.4917855912636,72.)) ;
#41555 = CARTESIAN_POINT('Origin',(0.,0.,72.)) ;
#41556 = CARTESIAN_POINT('',(20.7182286887658,17.1826947828331,72.)) ;
#41557 = CARTESIAN_POINT('',(22.5567063198509,19.0211724139181,72.)) ;
#41558 = CARTESIAN_POINT('',(18.9504617357995,18.9504617357995,72.)) ;
#41559 = CARTESIAN_POINT('Origin',(20.7889393668845,20.7889393668845,73.2)) ;
#41560 = CARTESIAN_POINT('',(21.6113450338214,18.0758111278886,73.2)) ;
#41561 = CARTESIAN_POINT('Origin',(0.,0.,73.2)) ;
#41562 = CARTESIAN_POINT('',(20.7182286887658,17.1826947828331,73.2)) ;
#41563 = CARTESIAN_POINT('',(18.9504617357995,18.9504617357995,73.2)) ;
#41564 = CARTESIAN_POINT('',(22.5567063198509,19.0211724139181,73.2)) ;
#41565 = CARTESIAN_POINT('Origin',(22.5567063198509,19.0211724139181,72.6)) ;
#41566 = CARTESIAN_POINT('Ctrl Pts',(21.6113450338214,18.0758111278886,73.2)) ;
#41567 = CARTESIAN_POINT('Ctrl Pts',(21.3150062760208,17.7794723700881,72.5910386886758)) ;
#41568 = CARTESIAN_POINT('Ctrl Pts',(21.0273194971963,17.4917855912636,72.)) ;
#41569 = CARTESIAN_POINT('',(20.7182286887658,17.1826947828331,72.6)) ;
#41570 = CARTESIAN_POINT('Origin',(18.9504617357995,18.9504617357995,72.6)) ;
#41571 = CARTESIAN_POINT('Origin',(22.6274169979695,22.6274169979695,72.6)) ;
#41572 = CARTESIAN_POINT('Origin',(0.,0.,110.)) ;
#41573 = CARTESIAN_POINT('',(-53.4,-6.53961390744687E-15,109.)) ;
#41574 = CARTESIAN_POINT('Origin',(0.,0.,109.)) ;
#41575 = CARTESIAN_POINT('',(-53.4,6.53961390744687E-15,109.124705882353)) ;
#41576 = CARTESIAN_POINT('',(-53.4,-6.53961390744687E-15,110.)) ;
#41577 = CARTESIAN_POINT('Origin',(0.,0.,109.124705882353)) ;
#41578 = CARTESIAN_POINT('Origin',(0.,0.,110.)) ;
#41579 = CARTESIAN_POINT('',(-53.4,6.53961390744687E-15,110.)) ;
#41580 = CARTESIAN_POINT('Origin',(0.,0.,110.)) ;
#41581 = CARTESIAN_POINT('',(-53.4,6.53961390744687E-15,111.)) ;
#41582 = CARTESIAN_POINT('',(-53.4,-6.53961390744687E-15,110.)) ;
#41583 = CARTESIAN_POINT('Origin',(0.,0.,111.)) ;
#41584 = CARTESIAN_POINT('Origin',(0.,0.,109.)) ;
#41585 = CARTESIAN_POINT('Origin',(0.,0.,111.)) ;
#41586 = CARTESIAN_POINT('Origin',(0.,0.,79.)) ;
#41587 = CARTESIAN_POINT('',(-10.9,-1.33486501107062E-15,48.)) ;
#41588 = CARTESIAN_POINT('Origin',(0.,0.,48.)) ;
#41589 = CARTESIAN_POINT('',(-32.15,-3.93723945925874E-15,79.)) ;
#41590 = CARTESIAN_POINT('Origin',(0.,0.,79.)) ;
#41591 = CARTESIAN_POINT('',(-11.5,-1.40834381901946E-15,48.)) ;
#41592 = CARTESIAN_POINT('',(-32.75,-4.01071826720758E-15,79.)) ;
#41593 = CARTESIAN_POINT('Origin',(0.,0.,48.)) ;
#41594 = CARTESIAN_POINT('Origin',(0.,0.,48.)) ;
#41595 = CARTESIAN_POINT('',(0.,0.,0.)) ;
#41596 = CARTESIAN_POINT('Origin',(0.,0.,113.4)) ;
#41597 = CARTESIAN_POINT('',(5.,2.,113.4)) ;
#41598 = CARTESIAN_POINT('',(-5.,2.,113.4)) ;
#41599 = CARTESIAN_POINT('',(0.,2.,113.4)) ;
#41600 = CARTESIAN_POINT('',(5.,-2.,113.4)) ;
#41601 = CARTESIAN_POINT('',(5.,0.,113.4)) ;
#41602 = CARTESIAN_POINT('',(-5.,-2.,113.4)) ;
#41603 = CARTESIAN_POINT('',(0.,-2.,113.4)) ;
#41604 = CARTESIAN_POINT('',(-5.,0.,113.4)) ;
#41605 = CARTESIAN_POINT('Origin',(-5.,0.,112.7)) ;
#41606 = CARTESIAN_POINT('',(-5.,2.,112.)) ;
#41607 = CARTESIAN_POINT('',(-5.,2.,112.85)) ;
#41608 = CARTESIAN_POINT('',(-5.,-2.,112.)) ;
#41609 = CARTESIAN_POINT('',(-5.,-2.,112.85)) ;
#41610 = CARTESIAN_POINT('',(-5.,0.,112.)) ;
#41611 = CARTESIAN_POINT('Origin',(5.,0.,112.7)) ;
#41612 = CARTESIAN_POINT('',(5.,2.,112.)) ;
#41613 = CARTESIAN_POINT('',(5.,2.,112.85)) ;
#41614 = CARTESIAN_POINT('',(5.,-2.,112.)) ;
#41615 = CARTESIAN_POINT('',(5.,0.,112.)) ;
#41616 = CARTESIAN_POINT('',(5.,-2.,112.85)) ;
#41617 = CARTESIAN_POINT('Origin',(0.,2.,113.)) ;
#41618 = CARTESIAN_POINT('',(-6.,2.,112.)) ;
#41619 = CARTESIAN_POINT('',(0.,2.,112.)) ;
#41620 = CARTESIAN_POINT('',(-6.,2.,114.)) ;
#41621 = CARTESIAN_POINT('',(-6.,2.,113.)) ;
#41622 = CARTESIAN_POINT('',(6.,2.,114.)) ;
#41623 = CARTESIAN_POINT('',(0.,2.,114.)) ;
#41624 = CARTESIAN_POINT('',(6.,2.,112.)) ;
#41625 = CARTESIAN_POINT('',(6.,2.,113.)) ;
#41626 = CARTESIAN_POINT('',(0.,2.,112.)) ;
#41627 = CARTESIAN_POINT('Origin',(0.,-2.,113.)) ;
#41628 = CARTESIAN_POINT('',(6.,-2.,112.)) ;
#41629 = CARTESIAN_POINT('',(0.,-2.,112.)) ;
#41630 = CARTESIAN_POINT('',(6.,-2.,114.)) ;
#41631 = CARTESIAN_POINT('',(6.,-2.,113.)) ;
#41632 = CARTESIAN_POINT('',(-6.,-2.,114.)) ;
#41633 = CARTESIAN_POINT('',(0.,-2.,114.)) ;
#41634 = CARTESIAN_POINT('',(-6.,-2.,112.)) ;
#41635 = CARTESIAN_POINT('',(-6.,-2.,113.)) ;
#41636 = CARTESIAN_POINT('',(0.,-2.,112.)) ;
#41637 = CARTESIAN_POINT('Origin',(0.,0.,114.)) ;
#41638 = CARTESIAN_POINT('',(6.,0.,114.)) ;
#41639 = CARTESIAN_POINT('',(-6.,0.,114.)) ;
#41640 = CARTESIAN_POINT('Origin',(-6.,0.,113.)) ;
#41641 = CARTESIAN_POINT('',(-6.,0.,112.)) ;
#41642 = CARTESIAN_POINT('Origin',(6.,0.,113.)) ;
#41643 = CARTESIAN_POINT('',(6.,0.,112.)) ;
#41644 = CARTESIAN_POINT('Origin',(0.,0.,110.6)) ;
#41645 = CARTESIAN_POINT('',(-55.05,-6.74168062930618E-15,110.)) ;
#41646 = CARTESIAN_POINT('Origin',(0.,0.,110.)) ;
#41647 = CARTESIAN_POINT('',(-55.05,6.74168062930618E-15,111.2)) ;
#41648 = CARTESIAN_POINT('',(-55.05,-6.74168062930618E-15,110.6)) ;
#41649 = CARTESIAN_POINT('Origin',(0.,0.,111.2)) ;
#41650 = CARTESIAN_POINT('Origin',(0.,0.,110.)) ;
#41651 = CARTESIAN_POINT('',(-55.5,-6.79678973526781E-15,110.)) ;
#41652 = CARTESIAN_POINT('Origin',(0.,0.,110.)) ;
#41653 = CARTESIAN_POINT('Origin',(0.,0.,111.6)) ;
#41654 = CARTESIAN_POINT('',(-55.5,-6.79678973526781E-15,112.)) ;
#41655 = CARTESIAN_POINT('Origin',(0.,0.,112.)) ;
#41656 = CARTESIAN_POINT('',(-55.5,-6.79678973526781E-15,111.6)) ;
#41657 = CARTESIAN_POINT('Origin',(0.,0.,111.2)) ;
#41658 = CARTESIAN_POINT('Origin',(0.,0.,112.)) ;
#41659 = CARTESIAN_POINT('',(0.,0.,0.)) ;
#41660 = CARTESIAN_POINT('Origin',(0.,53.4,112.6)) ;
#41661 = CARTESIAN_POINT('',(-4.,56.2803847577293,112.6)) ;
#41662 = CARTESIAN_POINT('',(4.,56.2803847577293,112.6)) ;
#41663 = CARTESIAN_POINT('',(0.,56.2803847577293,112.6)) ;
#41664 = CARTESIAN_POINT('',(-4.,50.,112.6)) ;
#41665 = CARTESIAN_POINT('',(-4.,53.4,112.6)) ;
#41666 = CARTESIAN_POINT('',(4.,50.,112.6)) ;
#41667 = CARTESIAN_POINT('',(0.,50.,112.6)) ;
#41668 = CARTESIAN_POINT('',(4.,53.4,112.6)) ;
#41669 = CARTESIAN_POINT('Origin',(0.,53.4,112.)) ;
#41670 = CARTESIAN_POINT('',(4.,56.2803847577293,112.)) ;
#41671 = CARTESIAN_POINT('',(-4.,56.2803847577293,112.)) ;
#41672 = CARTESIAN_POINT('',(0.,56.2803847577293,112.)) ;
#41673 = CARTESIAN_POINT('',(4.,50.,112.)) ;
#41674 = CARTESIAN_POINT('',(4.,53.4,112.)) ;
#41675 = CARTESIAN_POINT('',(-4.,50.,112.)) ;
#41676 = CARTESIAN_POINT('',(0.,50.,112.)) ;
#41677 = CARTESIAN_POINT('',(-4.,53.4,112.)) ;
#41678 = CARTESIAN_POINT('Origin',(0.,50.,112.3)) ;
#41679 = CARTESIAN_POINT('',(-4.,50.,112.3)) ;
#41680 = CARTESIAN_POINT('',(4.,50.,112.3)) ;
#41681 = CARTESIAN_POINT('Origin',(4.,56.8,112.3)) ;
#41682 = CARTESIAN_POINT('Origin',(4.,56.8,112.3)) ;
#41683 = CARTESIAN_POINT('Origin',(0.,56.8,112.3)) ;
#41684 = CARTESIAN_POINT('Origin',(-4.,56.8,112.3)) ;
#41685 = CARTESIAN_POINT('Origin',(-4.,56.8,112.3)) ;
#41686 = CARTESIAN_POINT('',(0.,0.,0.)) ;
#41687 = CARTESIAN_POINT('Origin',(41.6,0.,108.3)) ;
#41688 = CARTESIAN_POINT('',(41.6,-28.4,108.)) ;
#41689 = CARTESIAN_POINT('',(41.6,-28.4,108.6)) ;
#41690 = CARTESIAN_POINT('',(41.6,-28.4,108.3)) ;
#41691 = CARTESIAN_POINT('',(41.6,-28.6302287800849,108.)) ;
#41692 = CARTESIAN_POINT('',(41.6,0.,108.)) ;
#41693 = CARTESIAN_POINT('',(41.6,-28.6302287800849,108.6)) ;
#41694 = CARTESIAN_POINT('',(41.6,-28.6302287800849,108.3)) ;
#41695 = CARTESIAN_POINT('',(41.6,0.,108.6)) ;
#41696 = CARTESIAN_POINT('Origin',(41.6,0.,108.3)) ;
#41697 = CARTESIAN_POINT('',(41.6,-14.4,108.)) ;
#41698 = CARTESIAN_POINT('',(41.6,-14.4,108.6)) ;
#41699 = CARTESIAN_POINT('',(41.6,-14.4,108.3)) ;
#41700 = CARTESIAN_POINT('',(41.6,-27.6,108.)) ;
#41701 = CARTESIAN_POINT('',(41.6,0.,108.)) ;
#41702 = CARTESIAN_POINT('',(41.6,-27.6,108.6)) ;
#41703 = CARTESIAN_POINT('',(41.6,-27.6,108.3)) ;
#41704 = CARTESIAN_POINT('',(41.6,0.,108.6)) ;
#41705 = CARTESIAN_POINT('Origin',(41.6,0.,108.3)) ;
#41706 = CARTESIAN_POINT('',(41.6,-0.4,108.)) ;
#41707 = CARTESIAN_POINT('',(41.6,-0.4,108.6)) ;
#41708 = CARTESIAN_POINT('',(41.6,-0.4,108.3)) ;
#41709 = CARTESIAN_POINT('',(41.6,-13.6,108.)) ;
#41710 = CARTESIAN_POINT('',(41.6,0.,108.)) ;
#41711 = CARTESIAN_POINT('',(41.6,-13.6,108.6)) ;
#41712 = CARTESIAN_POINT('',(41.6,-13.6,108.3)) ;
#41713 = CARTESIAN_POINT('',(41.6,0.,108.6)) ;
#41714 = CARTESIAN_POINT('Origin',(41.6,0.,108.3)) ;
#41715 = CARTESIAN_POINT('',(41.6,13.6,108.)) ;
#41716 = CARTESIAN_POINT('',(41.6,13.6,108.6)) ;
#41717 = CARTESIAN_POINT('',(41.6,13.6,108.3)) ;
#41718 = CARTESIAN_POINT('',(41.6,0.4,108.)) ;
#41719 = CARTESIAN_POINT('',(41.6,0.,108.)) ;
#41720 = CARTESIAN_POINT('',(41.6,0.4,108.6)) ;
#41721 = CARTESIAN_POINT('',(41.6,0.4,108.3)) ;
#41722 = CARTESIAN_POINT('',(41.6,0.,108.6)) ;
#41723 = CARTESIAN_POINT('Origin',(41.6,0.,108.3)) ;
#41724 = CARTESIAN_POINT('',(41.6,27.6,108.)) ;
#41725 = CARTESIAN_POINT('',(41.6,27.6,108.6)) ;
#41726 = CARTESIAN_POINT('',(41.6,27.6,108.3)) ;
#41727 = CARTESIAN_POINT('',(41.6,14.4,108.)) ;
#41728 = CARTESIAN_POINT('',(41.6,0.,108.)) ;
#41729 = CARTESIAN_POINT('',(41.6,14.4,108.6)) ;
#41730 = CARTESIAN_POINT('',(41.6,14.4,108.3)) ;
#41731 = CARTESIAN_POINT('',(41.6,0.,108.6)) ;
#41732 = CARTESIAN_POINT('Origin',(41.6,0.,108.3)) ;
#41733 = CARTESIAN_POINT('',(41.6,28.6302287800849,108.)) ;
#41734 = CARTESIAN_POINT('',(41.6,28.6302287800849,108.6)) ;
#41735 = CARTESIAN_POINT('',(41.6,28.6302287800849,108.3)) ;
#41736 = CARTESIAN_POINT('',(41.6,28.4,108.)) ;
#41737 = CARTESIAN_POINT('',(41.6,0.,108.)) ;
#41738 = CARTESIAN_POINT('',(41.6,28.4,108.6)) ;
#41739 = CARTESIAN_POINT('',(41.6,28.4,108.3)) ;
#41740 = CARTESIAN_POINT('',(41.6,0.,108.6)) ;
#41741 = CARTESIAN_POINT('Origin',(42.4,0.,108.3)) ;
#41742 = CARTESIAN_POINT('',(42.4,29.2316609175736,108.)) ;
#41743 = CARTESIAN_POINT('',(42.4,29.2316609175736,108.6)) ;
#41744 = CARTESIAN_POINT('',(42.4,29.2316609175736,108.3)) ;
#41745 = CARTESIAN_POINT('',(42.4,29.8035232816525,108.)) ;
#41746 = CARTESIAN_POINT('',(42.4,0.,108.)) ;
#41747 = CARTESIAN_POINT('',(42.4,29.8035232816525,108.6)) ;
#41748 = CARTESIAN_POINT('',(42.4,29.8035232816525,108.3)) ;
#41749 = CARTESIAN_POINT('',(42.4,0.,108.6)) ;
#41750 = CARTESIAN_POINT('Origin',(42.4,0.,108.3)) ;
#41751 = CARTESIAN_POINT('',(42.4,-29.2316609175736,108.6)) ;
#41752 = CARTESIAN_POINT('',(42.4,-29.2316609175736,108.)) ;
#41753 = CARTESIAN_POINT('',(42.4,-29.2316609175736,108.3)) ;
#41754 = CARTESIAN_POINT('',(42.4,-29.8035232816525,108.6)) ;
#41755 = CARTESIAN_POINT('',(42.4,0.,108.6)) ;
#41756 = CARTESIAN_POINT('',(42.4,-29.8035232816525,108.)) ;
#41757 = CARTESIAN_POINT('',(42.4,-29.8035232816525,108.3)) ;
#41758 = CARTESIAN_POINT('',(42.4,0.,108.)) ;
#41759 = CARTESIAN_POINT('Origin',(42.4,0.,108.3)) ;
#41760 = CARTESIAN_POINT('',(42.4,-14.4,108.6)) ;
#41761 = CARTESIAN_POINT('',(42.4,-14.4,108.)) ;
#41762 = CARTESIAN_POINT('',(42.4,-14.4,108.3)) ;
#41763 = CARTESIAN_POINT('',(42.4,-27.4315511774307,108.6)) ;
#41764 = CARTESIAN_POINT('',(42.4,0.,108.6)) ;
#41765 = CARTESIAN_POINT('',(42.4,-27.4315511774307,108.)) ;
#41766 = CARTESIAN_POINT('',(42.4,-27.4315511774307,108.3)) ;
#41767 = CARTESIAN_POINT('',(42.4,0.,108.)) ;
#41768 = CARTESIAN_POINT('Origin',(42.4,0.,108.3)) ;
#41769 = CARTESIAN_POINT('',(42.4,-0.4,108.6)) ;
#41770 = CARTESIAN_POINT('',(42.4,-0.4,108.)) ;
#41771 = CARTESIAN_POINT('',(42.4,-0.4,108.3)) ;
#41772 = CARTESIAN_POINT('',(42.4,-13.6,108.6)) ;
#41773 = CARTESIAN_POINT('',(42.4,0.,108.6)) ;
#41774 = CARTESIAN_POINT('',(42.4,-13.6,108.)) ;
#41775 = CARTESIAN_POINT('',(42.4,-13.6,108.3)) ;
#41776 = CARTESIAN_POINT('',(42.4,0.,108.)) ;
#41777 = CARTESIAN_POINT('Origin',(42.4,0.,108.3)) ;
#41778 = CARTESIAN_POINT('',(42.4,13.6,108.6)) ;
#41779 = CARTESIAN_POINT('',(42.4,13.6,108.)) ;
#41780 = CARTESIAN_POINT('',(42.4,13.6,108.3)) ;
#41781 = CARTESIAN_POINT('',(42.4,0.4,108.6)) ;
#41782 = CARTESIAN_POINT('',(42.4,0.,108.6)) ;
#41783 = CARTESIAN_POINT('',(42.4,0.4,108.)) ;
#41784 = CARTESIAN_POINT('',(42.4,0.4,108.3)) ;
#41785 = CARTESIAN_POINT('',(42.4,0.,108.)) ;
#41786 = CARTESIAN_POINT('Origin',(42.4,0.,108.3)) ;
#41787 = CARTESIAN_POINT('',(42.4,27.4315511774307,108.6)) ;
#41788 = CARTESIAN_POINT('',(42.4,27.4315511774307,108.)) ;
#41789 = CARTESIAN_POINT('',(42.4,27.4315511774307,108.3)) ;
#41790 = CARTESIAN_POINT('',(42.4,14.4,108.6)) ;
#41791 = CARTESIAN_POINT('',(42.4,0.,108.6)) ;
#41792 = CARTESIAN_POINT('',(42.4,14.4,108.)) ;
#41793 = CARTESIAN_POINT('',(42.4,14.4,108.3)) ;
#41794 = CARTESIAN_POINT('',(42.4,0.,108.)) ;
#41795 = CARTESIAN_POINT('Origin',(42.,-29.8035232816525,108.3)) ;
#41796 = CARTESIAN_POINT('',(42.,-29.8035232816525,108.)) ;
#41797 = CARTESIAN_POINT('',(42.,-29.8035232816525,108.6)) ;
#41798 = CARTESIAN_POINT('',(42.,-29.8035232816525,108.3)) ;
#41799 = CARTESIAN_POINT('',(42.,-29.8035232816525,108.)) ;
#41800 = CARTESIAN_POINT('',(42.,-29.8035232816525,108.6)) ;
#41801 = CARTESIAN_POINT('Origin',(42.,29.8035232816525,108.3)) ;
#41802 = CARTESIAN_POINT('',(42.,29.8035232816525,108.6)) ;
#41803 = CARTESIAN_POINT('',(42.,29.8035232816525,108.)) ;
#41804 = CARTESIAN_POINT('',(42.,29.8035232816525,108.3)) ;
#41805 = CARTESIAN_POINT('',(42.,29.8035232816525,108.6)) ;
#41806 = CARTESIAN_POINT('',(42.,29.8035232816525,108.)) ;
#41807 = CARTESIAN_POINT('Origin',(0.,0.,108.3)) ;
#41808 = CARTESIAN_POINT('',(42.9614943874163,28.4,108.6)) ;
#41809 = CARTESIAN_POINT('Origin',(0.,0.,108.6)) ;
#41810 = CARTESIAN_POINT('',(42.9614943874163,28.4,108.)) ;
#41811 = CARTESIAN_POINT('',(42.9614943874163,28.4,108.3)) ;
#41812 = CARTESIAN_POINT('Origin',(0.,0.,108.)) ;
#41813 = CARTESIAN_POINT('Origin',(0.,0.,108.3)) ;
#41814 = CARTESIAN_POINT('',(29.8035232816525,42.,108.)) ;
#41815 = CARTESIAN_POINT('Origin',(0.,0.,108.)) ;
#41816 = CARTESIAN_POINT('',(29.8035232816525,42.,108.6)) ;
#41817 = CARTESIAN_POINT('',(29.8035232816525,42.,108.3)) ;
#41818 = CARTESIAN_POINT('Origin',(0.,0.,108.6)) ;
#41819 = CARTESIAN_POINT('Origin',(0.,0.,108.3)) ;
#41820 = CARTESIAN_POINT('',(48.4034089708566,14.4,108.)) ;
#41821 = CARTESIAN_POINT('Origin',(0.,0.,108.)) ;
#41822 = CARTESIAN_POINT('',(48.4034089708566,14.4,108.6)) ;
#41823 = CARTESIAN_POINT('',(48.4034089708566,14.4,108.3)) ;
#41824 = CARTESIAN_POINT('Origin',(0.,0.,108.6)) ;
#41825 = CARTESIAN_POINT('Origin',(0.,28.4,108.3)) ;
#41826 = CARTESIAN_POINT('',(28.4,28.4,108.)) ;
#41827 = CARTESIAN_POINT('',(0.,28.4,108.)) ;
#41828 = CARTESIAN_POINT('',(28.4,28.4,108.6)) ;
#41829 = CARTESIAN_POINT('',(28.4,28.4,108.3)) ;
#41830 = CARTESIAN_POINT('',(0.,28.4,108.6)) ;
#41831 = CARTESIAN_POINT('Origin',(0.,13.6,108.3)) ;
#41832 = CARTESIAN_POINT('',(48.6342471926933,13.6,108.)) ;
#41833 = CARTESIAN_POINT('',(0.,13.6,108.)) ;
#41834 = CARTESIAN_POINT('',(48.6342471926933,13.6,108.6)) ;
#41835 = CARTESIAN_POINT('',(48.6342471926933,13.6,108.3)) ;
#41836 = CARTESIAN_POINT('',(0.,13.6,108.6)) ;
#41837 = CARTESIAN_POINT('Origin',(0.,14.4,108.3)) ;
#41838 = CARTESIAN_POINT('',(28.4,14.4,108.)) ;
#41839 = CARTESIAN_POINT('',(0.,14.4,108.)) ;
#41840 = CARTESIAN_POINT('',(28.4,14.4,108.6)) ;
#41841 = CARTESIAN_POINT('',(28.4,14.4,108.3)) ;
#41842 = CARTESIAN_POINT('',(0.,14.4,108.6)) ;
#41843 = CARTESIAN_POINT('Origin',(0.,-0.4,108.3)) ;
#41844 = CARTESIAN_POINT('',(50.4984158167363,-0.4,108.)) ;
#41845 = CARTESIAN_POINT('',(0.,-0.4,108.)) ;
#41846 = CARTESIAN_POINT('',(50.4984158167363,-0.4,108.6)) ;
#41847 = CARTESIAN_POINT('',(50.4984158167363,-0.4,108.3)) ;
#41848 = CARTESIAN_POINT('',(0.,-0.4,108.6)) ;
#41849 = CARTESIAN_POINT('Origin',(0.,0.4,108.3)) ;
#41850 = CARTESIAN_POINT('',(28.4,0.4,108.)) ;
#41851 = CARTESIAN_POINT('',(0.,0.4,108.)) ;
#41852 = CARTESIAN_POINT('',(28.4,0.4,108.6)) ;
#41853 = CARTESIAN_POINT('',(28.4,0.4,108.3)) ;
#41854 = CARTESIAN_POINT('',(0.,0.4,108.6)) ;
#41855 = CARTESIAN_POINT('Origin',(0.,-14.4,108.3)) ;
#41856 = CARTESIAN_POINT('',(48.4034089708566,-14.4,108.)) ;
#41857 = CARTESIAN_POINT('',(0.,-14.4,108.)) ;
#41858 = CARTESIAN_POINT('',(48.4034089708566,-14.4,108.6)) ;
#41859 = CARTESIAN_POINT('',(48.4034089708566,-14.4,108.3)) ;
#41860 = CARTESIAN_POINT('',(0.,-14.4,108.6)) ;
#41861 = CARTESIAN_POINT('Origin',(0.,-13.6,108.3)) ;
#41862 = CARTESIAN_POINT('',(28.4,-13.6,108.)) ;
#41863 = CARTESIAN_POINT('',(0.,-13.6,108.)) ;
#41864 = CARTESIAN_POINT('',(28.4,-13.6,108.6)) ;
#41865 = CARTESIAN_POINT('',(28.4,-13.6,108.3)) ;
#41866 = CARTESIAN_POINT('',(0.,-13.6,108.6)) ;
#41867 = CARTESIAN_POINT('Origin',(0.,-27.6,108.3)) ;
#41868 = CARTESIAN_POINT('',(28.4,-27.6,108.)) ;
#41869 = CARTESIAN_POINT('',(0.,-27.6,108.)) ;
#41870 = CARTESIAN_POINT('',(28.4,-27.6,108.6)) ;
#41871 = CARTESIAN_POINT('',(28.4,-27.6,108.3)) ;
#41872 = CARTESIAN_POINT('',(0.,-27.6,108.6)) ;
#41873 = CARTESIAN_POINT('Origin',(0.,0.,108.6)) ;
#41874 = CARTESIAN_POINT('',(29.8035232816525,42.4,108.6)) ;
#41875 = CARTESIAN_POINT('',(29.8035232816525,42.,108.6)) ;
#41876 = CARTESIAN_POINT('',(29.2316609175736,42.4,108.6)) ;
#41877 = CARTESIAN_POINT('',(0.,42.4,108.6)) ;
#41878 = CARTESIAN_POINT('',(28.4,42.9614943874163,108.6)) ;
#41879 = CARTESIAN_POINT('Origin',(0.,0.,108.6)) ;
#41880 = CARTESIAN_POINT('',(28.4,43.2232576282723,108.6)) ;
#41881 = CARTESIAN_POINT('',(28.4,0.,108.6)) ;
#41882 = CARTESIAN_POINT('',(28.,43.2232576282723,108.6)) ;
#41883 = CARTESIAN_POINT('',(28.,43.2232576282723,108.6)) ;
#41884 = CARTESIAN_POINT('',(14.4,49.4458289444115,108.6)) ;
#41885 = CARTESIAN_POINT('Origin',(0.,0.,108.6)) ;
#41886 = CARTESIAN_POINT('',(14.4,49.5605690039975,108.6)) ;
#41887 = CARTESIAN_POINT('',(14.4,0.,108.6)) ;
#41888 = CARTESIAN_POINT('',(14.,49.5605690039975,108.6)) ;
#41889 = CARTESIAN_POINT('',(14.,49.5605690039975,108.6)) ;
#41890 = CARTESIAN_POINT('',(0.4,51.4984465785134,108.6)) ;
#41891 = CARTESIAN_POINT('Origin',(0.,0.,108.6)) ;
#41892 = CARTESIAN_POINT('',(0.4,51.5,108.6)) ;
#41893 = CARTESIAN_POINT('',(0.4,0.,108.6)) ;
#41894 = CARTESIAN_POINT('',(-0.4,51.5,108.6)) ;
#41895 = CARTESIAN_POINT('',(0.,51.5,108.6)) ;
#41896 = CARTESIAN_POINT('',(-0.4,51.4984465785134,108.6)) ;
#41897 = CARTESIAN_POINT('',(-0.4,0.,108.6)) ;
#41898 = CARTESIAN_POINT('',(-14.,49.5605690039975,108.6)) ;
#41899 = CARTESIAN_POINT('Origin',(0.,0.,108.6)) ;
#41900 = CARTESIAN_POINT('',(-14.4,49.5605690039975,108.6)) ;
#41901 = CARTESIAN_POINT('',(-14.,49.5605690039975,108.6)) ;
#41902 = CARTESIAN_POINT('',(-14.4,49.4458289444115,108.6)) ;
#41903 = CARTESIAN_POINT('',(-14.4,0.,108.6)) ;
#41904 = CARTESIAN_POINT('',(-28.,43.2232576282723,108.6)) ;
#41905 = CARTESIAN_POINT('Origin',(0.,0.,108.6)) ;
#41906 = CARTESIAN_POINT('',(-28.4,43.2232576282723,108.6)) ;
#41907 = CARTESIAN_POINT('',(-28.,43.2232576282723,108.6)) ;
#41908 = CARTESIAN_POINT('',(-28.4,42.9614943874163,108.6)) ;
#41909 = CARTESIAN_POINT('',(-28.4,0.,108.6)) ;
#41910 = CARTESIAN_POINT('',(-29.2316609175736,42.4,108.6)) ;
#41911 = CARTESIAN_POINT('Origin',(0.,0.,108.6)) ;
#41912 = CARTESIAN_POINT('',(-29.8035232816525,42.4,108.6)) ;
#41913 = CARTESIAN_POINT('',(0.,42.4,108.6)) ;
#41914 = CARTESIAN_POINT('',(-29.8035232816525,42.,108.6)) ;
#41915 = CARTESIAN_POINT('',(-29.8035232816525,42.,108.6)) ;
#41916 = CARTESIAN_POINT('',(-42.,29.8035232816525,108.6)) ;
#41917 = CARTESIAN_POINT('Origin',(0.,0.,108.6)) ;
#41918 = CARTESIAN_POINT('',(-42.4,29.8035232816525,108.6)) ;
#41919 = CARTESIAN_POINT('',(-42.,29.8035232816525,108.6)) ;
#41920 = CARTESIAN_POINT('',(-42.4,29.2316609175736,108.6)) ;
#41921 = CARTESIAN_POINT('',(-42.4,0.,108.6)) ;
#41922 = CARTESIAN_POINT('',(-42.9614943874163,28.4,108.6)) ;
#41923 = CARTESIAN_POINT('Origin',(0.,0.,108.6)) ;
#41924 = CARTESIAN_POINT('',(-43.2232576282723,28.4,108.6)) ;
#41925 = CARTESIAN_POINT('',(0.,28.4,108.6)) ;
#41926 = CARTESIAN_POINT('',(-43.2232576282723,28.,108.6)) ;
#41927 = CARTESIAN_POINT('',(-43.2232576282723,28.,108.6)) ;
#41928 = CARTESIAN_POINT('',(-49.4458289444115,14.4,108.6)) ;
#41929 = CARTESIAN_POINT('Origin',(0.,0.,108.6)) ;
#41930 = CARTESIAN_POINT('',(-49.5605690039975,14.4,108.6)) ;
#41931 = CARTESIAN_POINT('',(0.,14.4,108.6)) ;
#41932 = CARTESIAN_POINT('',(-49.5605690039975,14.,108.6)) ;
#41933 = CARTESIAN_POINT('',(-49.5605690039975,14.,108.6)) ;
#41934 = CARTESIAN_POINT('',(-51.4984465785134,0.4,108.6)) ;
#41935 = CARTESIAN_POINT('Origin',(0.,0.,108.6)) ;
#41936 = CARTESIAN_POINT('',(-51.5,0.4,108.6)) ;
#41937 = CARTESIAN_POINT('',(0.,0.4,108.6)) ;
#41938 = CARTESIAN_POINT('',(-51.5,-0.4,108.6)) ;
#41939 = CARTESIAN_POINT('',(-51.5,0.,108.6)) ;
#41940 = CARTESIAN_POINT('',(-51.4984465785134,-0.4,108.6)) ;
#41941 = CARTESIAN_POINT('',(0.,-0.4,108.6)) ;
#41942 = CARTESIAN_POINT('',(-49.5605690039975,-14.,108.6)) ;
#41943 = CARTESIAN_POINT('Origin',(0.,0.,108.6)) ;
#41944 = CARTESIAN_POINT('',(-49.5605690039975,-14.4,108.6)) ;
#41945 = CARTESIAN_POINT('',(-49.5605690039975,-14.,108.6)) ;
#41946 = CARTESIAN_POINT('',(-49.4458289444115,-14.4,108.6)) ;
#41947 = CARTESIAN_POINT('',(0.,-14.4,108.6)) ;
#41948 = CARTESIAN_POINT('',(-43.2232576282723,-28.,108.6)) ;
#41949 = CARTESIAN_POINT('Origin',(0.,0.,108.6)) ;
#41950 = CARTESIAN_POINT('',(-43.2232576282723,-28.4,108.6)) ;
#41951 = CARTESIAN_POINT('',(-43.2232576282723,-28.,108.6)) ;
#41952 = CARTESIAN_POINT('',(-42.9614943874163,-28.4,108.6)) ;
#41953 = CARTESIAN_POINT('',(0.,-28.4,108.6)) ;
#41954 = CARTESIAN_POINT('',(-42.4,-29.2316609175736,108.6)) ;
#41955 = CARTESIAN_POINT('Origin',(0.,0.,108.6)) ;
#41956 = CARTESIAN_POINT('',(-42.4,-29.8035232816525,108.6)) ;
#41957 = CARTESIAN_POINT('',(-42.4,0.,108.6)) ;
#41958 = CARTESIAN_POINT('',(-42.,-29.8035232816525,108.6)) ;
#41959 = CARTESIAN_POINT('',(-42.,-29.8035232816525,108.6)) ;
#41960 = CARTESIAN_POINT('',(-29.8035232816525,-42.,108.6)) ;
#41961 = CARTESIAN_POINT('Origin',(0.,0.,108.6)) ;
#41962 = CARTESIAN_POINT('',(-29.8035232816525,-42.4,108.6)) ;
#41963 = CARTESIAN_POINT('',(-29.8035232816525,-42.,108.6)) ;
#41964 = CARTESIAN_POINT('',(-29.2316609175736,-42.4,108.6)) ;
#41965 = CARTESIAN_POINT('',(0.,-42.4,108.6)) ;
#41966 = CARTESIAN_POINT('',(-28.4,-42.9614943874163,108.6)) ;
#41967 = CARTESIAN_POINT('Origin',(0.,0.,108.6)) ;
#41968 = CARTESIAN_POINT('',(-28.4,-43.2232576282723,108.6)) ;
#41969 = CARTESIAN_POINT('',(-28.4,0.,108.6)) ;
#41970 = CARTESIAN_POINT('',(-28.,-43.2232576282723,108.6)) ;
#41971 = CARTESIAN_POINT('',(-28.,-43.2232576282723,108.6)) ;
#41972 = CARTESIAN_POINT('',(-14.4,-49.4458289444115,108.6)) ;
#41973 = CARTESIAN_POINT('Origin',(0.,0.,108.6)) ;
#41974 = CARTESIAN_POINT('',(-14.4,-49.5605690039975,108.6)) ;
#41975 = CARTESIAN_POINT('',(-14.4,0.,108.6)) ;
#41976 = CARTESIAN_POINT('',(-14.,-49.5605690039975,108.6)) ;
#41977 = CARTESIAN_POINT('',(-14.,-49.5605690039975,108.6)) ;
#41978 = CARTESIAN_POINT('',(-0.4,-51.4984465785134,108.6)) ;
#41979 = CARTESIAN_POINT('Origin',(0.,0.,108.6)) ;
#41980 = CARTESIAN_POINT('',(-0.4,-51.5,108.6)) ;
#41981 = CARTESIAN_POINT('',(-0.4,0.,108.6)) ;
#41982 = CARTESIAN_POINT('',(0.4,-51.5,108.6)) ;
#41983 = CARTESIAN_POINT('',(0.,-51.5,108.6)) ;
#41984 = CARTESIAN_POINT('',(0.4,-51.4984465785134,108.6)) ;
#41985 = CARTESIAN_POINT('',(0.4,0.,108.6)) ;
#41986 = CARTESIAN_POINT('',(14.,-49.5605690039975,108.6)) ;
#41987 = CARTESIAN_POINT('Origin',(0.,0.,108.6)) ;
#41988 = CARTESIAN_POINT('',(14.4,-49.5605690039975,108.6)) ;
#41989 = CARTESIAN_POINT('',(14.,-49.5605690039975,108.6)) ;
#41990 = CARTESIAN_POINT('',(14.4,-49.4458289444115,108.6)) ;
#41991 = CARTESIAN_POINT('',(14.4,0.,108.6)) ;
#41992 = CARTESIAN_POINT('',(28.,-43.2232576282723,108.6)) ;
#41993 = CARTESIAN_POINT('Origin',(0.,0.,108.6)) ;
#41994 = CARTESIAN_POINT('',(28.4,-43.2232576282723,108.6)) ;
#41995 = CARTESIAN_POINT('',(28.,-43.2232576282723,108.6)) ;
#41996 = CARTESIAN_POINT('',(28.4,-42.9614943874163,108.6)) ;
#41997 = CARTESIAN_POINT('',(28.4,0.,108.6)) ;
#41998 = CARTESIAN_POINT('',(29.2316609175736,-42.4,108.6)) ;
#41999 = CARTESIAN_POINT('Origin',(0.,0.,108.6)) ;
#42000 = CARTESIAN_POINT('',(29.8035232816525,-42.4,108.6)) ;
#42001 = CARTESIAN_POINT('',(0.,-42.4,108.6)) ;
#42002 = CARTESIAN_POINT('',(29.8035232816525,-42.,108.6)) ;
#42003 = CARTESIAN_POINT('',(29.8035232816525,-42.,108.6)) ;
#42004 = CARTESIAN_POINT('Origin',(0.,0.,108.6)) ;
#42005 = CARTESIAN_POINT('',(42.9614943874163,-28.4,108.6)) ;
#42006 = CARTESIAN_POINT('Origin',(0.,0.,108.6)) ;
#42007 = CARTESIAN_POINT('',(43.2232576282723,-28.4,108.6)) ;
#42008 = CARTESIAN_POINT('',(0.,-28.4,108.6)) ;
#42009 = CARTESIAN_POINT('',(43.2232576282723,-28.,108.6)) ;
#42010 = CARTESIAN_POINT('',(43.2232576282723,-28.,108.6)) ;
#42011 = CARTESIAN_POINT('',(49.4458289444115,-14.4,108.6)) ;
#42012 = CARTESIAN_POINT('Origin',(0.,0.,108.6)) ;
#42013 = CARTESIAN_POINT('',(49.5605690039975,-14.4,108.6)) ;
#42014 = CARTESIAN_POINT('',(0.,-14.4,108.6)) ;
#42015 = CARTESIAN_POINT('',(49.5605690039975,-14.,108.6)) ;
#42016 = CARTESIAN_POINT('',(49.5605690039975,-14.,108.6)) ;
#42017 = CARTESIAN_POINT('',(51.4984465785134,-0.4,108.6)) ;
#42018 = CARTESIAN_POINT('Origin',(0.,0.,108.6)) ;
#42019 = CARTESIAN_POINT('',(51.5,-0.4,108.6)) ;
#42020 = CARTESIAN_POINT('',(0.,-0.4,108.6)) ;
#42021 = CARTESIAN_POINT('',(51.5,0.4,108.6)) ;
#42022 = CARTESIAN_POINT('',(51.5,0.,108.6)) ;
#42023 = CARTESIAN_POINT('',(51.4984465785134,0.4,108.6)) ;
#42024 = CARTESIAN_POINT('',(0.,0.4,108.6)) ;
#42025 = CARTESIAN_POINT('',(49.5605690039975,14.,108.6)) ;
#42026 = CARTESIAN_POINT('Origin',(0.,0.,108.6)) ;
#42027 = CARTESIAN_POINT('',(49.5605690039975,14.4,108.6)) ;
#42028 = CARTESIAN_POINT('',(49.5605690039975,14.,108.6)) ;
#42029 = CARTESIAN_POINT('',(49.4458289444115,14.4,108.6)) ;
#42030 = CARTESIAN_POINT('',(0.,14.4,108.6)) ;
#42031 = CARTESIAN_POINT('',(43.2232576282723,28.,108.6)) ;
#42032 = CARTESIAN_POINT('Origin',(0.,0.,108.6)) ;
#42033 = CARTESIAN_POINT('',(43.2232576282723,28.4,108.6)) ;
#42034 = CARTESIAN_POINT('',(43.2232576282723,28.,108.6)) ;
#42035 = CARTESIAN_POINT('',(0.,28.4,108.6)) ;
#42036 = CARTESIAN_POINT('',(0.,14.4,108.6)) ;
#42037 = CARTESIAN_POINT('',(50.4984158167363,0.4,108.6)) ;
#42038 = CARTESIAN_POINT('Origin',(0.,0.,108.6)) ;
#42039 = CARTESIAN_POINT('',(0.,0.4,108.6)) ;
#42040 = CARTESIAN_POINT('',(48.6342471926933,-13.6,108.6)) ;
#42041 = CARTESIAN_POINT('Origin',(0.,0.,108.6)) ;
#42042 = CARTESIAN_POINT('',(0.,-13.6,108.6)) ;
#42043 = CARTESIAN_POINT('Origin',(0.,0.,108.6)) ;
#42044 = CARTESIAN_POINT('',(28.4,27.6,108.6)) ;
#42045 = CARTESIAN_POINT('',(28.4,0.,108.6)) ;
#42046 = CARTESIAN_POINT('',(0.,27.6,108.6)) ;
#42047 = CARTESIAN_POINT('',(28.4,13.6,108.6)) ;
#42048 = CARTESIAN_POINT('',(28.4,0.,108.6)) ;
#42049 = CARTESIAN_POINT('',(0.,13.6,108.6)) ;
#42050 = CARTESIAN_POINT('',(28.4,-0.4,108.6)) ;
#42051 = CARTESIAN_POINT('',(28.4,0.,108.6)) ;
#42052 = CARTESIAN_POINT('',(0.,-0.4,108.6)) ;
#42053 = CARTESIAN_POINT('',(28.4,-14.4,108.6)) ;
#42054 = CARTESIAN_POINT('',(28.4,0.,108.6)) ;
#42055 = CARTESIAN_POINT('',(0.,-14.4,108.6)) ;
#42056 = CARTESIAN_POINT('',(28.4,41.6,108.6)) ;
#42057 = CARTESIAN_POINT('',(28.4,0.,108.6)) ;
#42058 = CARTESIAN_POINT('',(28.6302287800849,41.6,108.6)) ;
#42059 = CARTESIAN_POINT('',(0.,41.6,108.6)) ;
#42060 = CARTESIAN_POINT('Origin',(0.,0.,108.6)) ;
#42061 = CARTESIAN_POINT('',(14.4,42.4,108.6)) ;
#42062 = CARTESIAN_POINT('',(14.4,48.4034089708566,108.6)) ;
#42063 = CARTESIAN_POINT('',(14.4,0.,108.6)) ;
#42064 = CARTESIAN_POINT('',(27.4315511774307,42.4,108.6)) ;
#42065 = CARTESIAN_POINT('Origin',(0.,0.,108.6)) ;
#42066 = CARTESIAN_POINT('',(0.,42.4,108.6)) ;
#42067 = CARTESIAN_POINT('',(13.6,41.6,108.6)) ;
#42068 = CARTESIAN_POINT('',(13.6,28.4,108.6)) ;
#42069 = CARTESIAN_POINT('',(13.6,0.,108.6)) ;
#42070 = CARTESIAN_POINT('',(0.4,28.4,108.6)) ;
#42071 = CARTESIAN_POINT('',(0.,28.4,108.6)) ;
#42072 = CARTESIAN_POINT('',(0.4,41.6,108.6)) ;
#42073 = CARTESIAN_POINT('',(0.4,0.,108.6)) ;
#42074 = CARTESIAN_POINT('',(0.,41.6,108.6)) ;
#42075 = CARTESIAN_POINT('',(-0.4,41.6,108.6)) ;
#42076 = CARTESIAN_POINT('',(-0.4,28.4,108.6)) ;
#42077 = CARTESIAN_POINT('',(-0.4,0.,108.6)) ;
#42078 = CARTESIAN_POINT('',(-13.6,28.4,108.6)) ;
#42079 = CARTESIAN_POINT('',(0.,28.4,108.6)) ;
#42080 = CARTESIAN_POINT('',(-13.6,41.6,108.6)) ;
#42081 = CARTESIAN_POINT('',(-13.6,0.,108.6)) ;
#42082 = CARTESIAN_POINT('',(0.,41.6,108.6)) ;
#42083 = CARTESIAN_POINT('',(-14.4,41.6,108.6)) ;
#42084 = CARTESIAN_POINT('',(-14.4,28.4,108.6)) ;
#42085 = CARTESIAN_POINT('',(-14.4,0.,108.6)) ;
#42086 = CARTESIAN_POINT('',(-27.6,28.4,108.6)) ;
#42087 = CARTESIAN_POINT('',(0.,28.4,108.6)) ;
#42088 = CARTESIAN_POINT('',(-27.6,41.6,108.6)) ;
#42089 = CARTESIAN_POINT('',(-27.6,0.,108.6)) ;
#42090 = CARTESIAN_POINT('',(0.,41.6,108.6)) ;
#42091 = CARTESIAN_POINT('',(14.4,41.6,108.6)) ;
#42092 = CARTESIAN_POINT('',(27.6,41.6,108.6)) ;
#42093 = CARTESIAN_POINT('',(0.,41.6,108.6)) ;
#42094 = CARTESIAN_POINT('',(27.6,28.4,108.6)) ;
#42095 = CARTESIAN_POINT('',(27.6,0.,108.6)) ;
#42096 = CARTESIAN_POINT('',(14.4,28.4,108.6)) ;
#42097 = CARTESIAN_POINT('',(0.,28.4,108.6)) ;
#42098 = CARTESIAN_POINT('',(14.4,0.,108.6)) ;
#42099 = CARTESIAN_POINT('',(13.6,42.4,108.6)) ;
#42100 = CARTESIAN_POINT('',(0.4,42.4,108.6)) ;
#42101 = CARTESIAN_POINT('',(0.,42.4,108.6)) ;
#42102 = CARTESIAN_POINT('',(0.4,50.4984158167363,108.6)) ;
#42103 = CARTESIAN_POINT('',(0.4,0.,108.6)) ;
#42104 = CARTESIAN_POINT('',(13.6,48.6342471926933,108.6)) ;
#42105 = CARTESIAN_POINT('Origin',(0.,0.,108.6)) ;
#42106 = CARTESIAN_POINT('',(13.6,0.,108.6)) ;
#42107 = CARTESIAN_POINT('',(-0.4,42.4,108.6)) ;
#42108 = CARTESIAN_POINT('',(-13.6,42.4,108.6)) ;
#42109 = CARTESIAN_POINT('',(0.,42.4,108.6)) ;
#42110 = CARTESIAN_POINT('',(-13.6,48.6342471926933,108.6)) ;
#42111 = CARTESIAN_POINT('',(-13.6,0.,108.6)) ;
#42112 = CARTESIAN_POINT('',(-0.4,50.4984158167363,108.6)) ;
#42113 = CARTESIAN_POINT('Origin',(0.,0.,108.6)) ;
#42114 = CARTESIAN_POINT('',(-0.4,0.,108.6)) ;
#42115 = CARTESIAN_POINT('',(-28.4,41.6,108.6)) ;
#42116 = CARTESIAN_POINT('',(-28.4,28.4,108.6)) ;
#42117 = CARTESIAN_POINT('',(-28.4,0.,108.6)) ;
#42118 = CARTESIAN_POINT('',(-41.6,28.4,108.6)) ;
#42119 = CARTESIAN_POINT('',(0.,28.4,108.6)) ;
#42120 = CARTESIAN_POINT('',(-41.6,28.6302287800849,108.6)) ;
#42121 = CARTESIAN_POINT('',(-41.6,0.,108.6)) ;
#42122 = CARTESIAN_POINT('',(-28.6302287800849,41.6,108.6)) ;
#42123 = CARTESIAN_POINT('Origin',(0.,0.,108.6)) ;
#42124 = CARTESIAN_POINT('',(0.,41.6,108.6)) ;
#42125 = CARTESIAN_POINT('',(-14.4,42.4,108.6)) ;
#42126 = CARTESIAN_POINT('',(-27.4315511774307,42.4,108.6)) ;
#42127 = CARTESIAN_POINT('',(0.,42.4,108.6)) ;
#42128 = CARTESIAN_POINT('',(-14.4,48.4034089708566,108.6)) ;
#42129 = CARTESIAN_POINT('Origin',(0.,0.,108.6)) ;
#42130 = CARTESIAN_POINT('',(-14.4,0.,108.6)) ;
#42131 = CARTESIAN_POINT('',(-0.4,-50.4984158167363,108.6)) ;
#42132 = CARTESIAN_POINT('',(-13.6,-48.6342471926933,108.6)) ;
#42133 = CARTESIAN_POINT('Origin',(0.,0.,108.6)) ;
#42134 = CARTESIAN_POINT('',(-13.6,-42.4,108.6)) ;
#42135 = CARTESIAN_POINT('',(-13.6,0.,108.6)) ;
#42136 = CARTESIAN_POINT('',(-0.4,-42.4,108.6)) ;
#42137 = CARTESIAN_POINT('',(0.,-42.4,108.6)) ;
#42138 = CARTESIAN_POINT('',(-0.4,0.,108.6)) ;
#42139 = CARTESIAN_POINT('',(-0.4,-0.4,108.6)) ;
#42140 = CARTESIAN_POINT('',(-0.4,-13.6,108.6)) ;
#42141 = CARTESIAN_POINT('',(-0.4,0.,108.6)) ;
#42142 = CARTESIAN_POINT('',(-13.6,-13.6,108.6)) ;
#42143 = CARTESIAN_POINT('',(0.,-13.6,108.6)) ;
#42144 = CARTESIAN_POINT('',(-13.6,-0.4,108.6)) ;
#42145 = CARTESIAN_POINT('',(-13.6,0.,108.6)) ;
#42146 = CARTESIAN_POINT('',(0.,-0.4,108.6)) ;
#42147 = CARTESIAN_POINT('',(-0.4,-14.4,108.6)) ;
#42148 = CARTESIAN_POINT('',(-0.4,-27.6,108.6)) ;
#42149 = CARTESIAN_POINT('',(-0.4,0.,108.6)) ;
#42150 = CARTESIAN_POINT('',(-13.6,-27.6,108.6)) ;
#42151 = CARTESIAN_POINT('',(0.,-27.6,108.6)) ;
#42152 = CARTESIAN_POINT('',(-13.6,-14.4,108.6)) ;
#42153 = CARTESIAN_POINT('',(-13.6,0.,108.6)) ;
#42154 = CARTESIAN_POINT('',(0.,-14.4,108.6)) ;
#42155 = CARTESIAN_POINT('',(-0.4,-28.4,108.6)) ;
#42156 = CARTESIAN_POINT('',(-0.4,-41.6,108.6)) ;
#42157 = CARTESIAN_POINT('',(-0.4,0.,108.6)) ;
#42158 = CARTESIAN_POINT('',(-13.6,-41.6,108.6)) ;
#42159 = CARTESIAN_POINT('',(0.,-41.6,108.6)) ;
#42160 = CARTESIAN_POINT('',(-13.6,-28.4,108.6)) ;
#42161 = CARTESIAN_POINT('',(-13.6,0.,108.6)) ;
#42162 = CARTESIAN_POINT('',(0.,-28.4,108.6)) ;
#42163 = CARTESIAN_POINT('',(-14.4,-0.4,108.6)) ;
#42164 = CARTESIAN_POINT('',(-14.4,-13.6,108.6)) ;
#42165 = CARTESIAN_POINT('',(-14.4,0.,108.6)) ;
#42166 = CARTESIAN_POINT('',(-27.6,-13.6,108.6)) ;
#42167 = CARTESIAN_POINT('',(0.,-13.6,108.6)) ;
#42168 = CARTESIAN_POINT('',(-27.6,-0.4,108.6)) ;
#42169 = CARTESIAN_POINT('',(-27.6,0.,108.6)) ;
#42170 = CARTESIAN_POINT('',(0.,-0.4,108.6)) ;
#42171 = CARTESIAN_POINT('',(-28.4,-0.4,108.6)) ;
#42172 = CARTESIAN_POINT('',(-28.4,-13.6,108.6)) ;
#42173 = CARTESIAN_POINT('',(-28.4,0.,108.6)) ;
#42174 = CARTESIAN_POINT('',(-41.6,-13.6,108.6)) ;
#42175 = CARTESIAN_POINT('',(0.,-13.6,108.6)) ;
#42176 = CARTESIAN_POINT('',(-41.6,-0.4,108.6)) ;
#42177 = CARTESIAN_POINT('',(-41.6,0.,108.6)) ;
#42178 = CARTESIAN_POINT('',(0.,-0.4,108.6)) ;
#42179 = CARTESIAN_POINT('',(-42.4,-0.4,108.6)) ;
#42180 = CARTESIAN_POINT('',(-42.4,-13.6,108.6)) ;
#42181 = CARTESIAN_POINT('',(-42.4,0.,108.6)) ;
#42182 = CARTESIAN_POINT('',(-48.6342471926933,-13.6,108.6)) ;
#42183 = CARTESIAN_POINT('',(0.,-13.6,108.6)) ;
#42184 = CARTESIAN_POINT('',(-50.4984158167363,-0.4,108.6)) ;
#42185 = CARTESIAN_POINT('Origin',(0.,0.,108.6)) ;
#42186 = CARTESIAN_POINT('',(0.,-0.4,108.6)) ;
#42187 = CARTESIAN_POINT('',(-14.4,-28.4,108.6)) ;
#42188 = CARTESIAN_POINT('',(-14.4,-41.6,108.6)) ;
#42189 = CARTESIAN_POINT('',(-14.4,0.,108.6)) ;
#42190 = CARTESIAN_POINT('',(-27.6,-41.6,108.6)) ;
#42191 = CARTESIAN_POINT('',(0.,-41.6,108.6)) ;
#42192 = CARTESIAN_POINT('',(-27.6,-28.4,108.6)) ;
#42193 = CARTESIAN_POINT('',(-27.6,0.,108.6)) ;
#42194 = CARTESIAN_POINT('',(0.,-28.4,108.6)) ;
#42195 = CARTESIAN_POINT('',(-14.4,-14.4,108.6)) ;
#42196 = CARTESIAN_POINT('',(-14.4,-27.6,108.6)) ;
#42197 = CARTESIAN_POINT('',(-14.4,0.,108.6)) ;
#42198 = CARTESIAN_POINT('',(-27.6,-27.6,108.6)) ;
#42199 = CARTESIAN_POINT('',(0.,-27.6,108.6)) ;
#42200 = CARTESIAN_POINT('',(-27.6,-14.4,108.6)) ;
#42201 = CARTESIAN_POINT('',(-27.6,0.,108.6)) ;
#42202 = CARTESIAN_POINT('',(0.,-14.4,108.6)) ;
#42203 = CARTESIAN_POINT('',(-14.4,-42.4,108.6)) ;
#42204 = CARTESIAN_POINT('',(-14.4,-48.4034089708566,108.6)) ;
#42205 = CARTESIAN_POINT('',(-14.4,0.,108.6)) ;
#42206 = CARTESIAN_POINT('',(-27.4315511774307,-42.4,108.6)) ;
#42207 = CARTESIAN_POINT('Origin',(0.,0.,108.6)) ;
#42208 = CARTESIAN_POINT('',(0.,-42.4,108.6)) ;
#42209 = CARTESIAN_POINT('',(-28.4,-28.4,108.6)) ;
#42210 = CARTESIAN_POINT('',(-28.4,-41.6,108.6)) ;
#42211 = CARTESIAN_POINT('',(-28.4,0.,108.6)) ;
#42212 = CARTESIAN_POINT('',(-28.6302287800849,-41.6,108.6)) ;
#42213 = CARTESIAN_POINT('',(0.,-41.6,108.6)) ;
#42214 = CARTESIAN_POINT('',(-41.6,-28.6302287800849,108.6)) ;
#42215 = CARTESIAN_POINT('Origin',(0.,0.,108.6)) ;
#42216 = CARTESIAN_POINT('',(-41.6,-28.4,108.6)) ;
#42217 = CARTESIAN_POINT('',(-41.6,0.,108.6)) ;
#42218 = CARTESIAN_POINT('',(0.,-28.4,108.6)) ;
#42219 = CARTESIAN_POINT('',(-42.4,-14.4,108.6)) ;
#42220 = CARTESIAN_POINT('',(-42.4,-27.4315511774307,108.6)) ;
#42221 = CARTESIAN_POINT('',(-42.4,0.,108.6)) ;
#42222 = CARTESIAN_POINT('',(-48.4034089708566,-14.4,108.6)) ;
#42223 = CARTESIAN_POINT('Origin',(0.,0.,108.6)) ;
#42224 = CARTESIAN_POINT('',(0.,-14.4,108.6)) ;
#42225 = CARTESIAN_POINT('',(-28.4,-14.4,108.6)) ;
#42226 = CARTESIAN_POINT('',(-28.4,-27.6,108.6)) ;
#42227 = CARTESIAN_POINT('',(-28.4,0.,108.6)) ;
#42228 = CARTESIAN_POINT('',(-41.6,-27.6,108.6)) ;
#42229 = CARTESIAN_POINT('',(0.,-27.6,108.6)) ;
#42230 = CARTESIAN_POINT('',(-41.6,-14.4,108.6)) ;
#42231 = CARTESIAN_POINT('',(-41.6,0.,108.6)) ;
#42232 = CARTESIAN_POINT('',(0.,-14.4,108.6)) ;
#42233 = CARTESIAN_POINT('',(-42.4,14.4,108.6)) ;
#42234 = CARTESIAN_POINT('',(-48.4034089708566,14.4,108.6)) ;
#42235 = CARTESIAN_POINT('',(0.,14.4,108.6)) ;
#42236 = CARTESIAN_POINT('',(-42.4,27.4315511774307,108.6)) ;
#42237 = CARTESIAN_POINT('Origin',(0.,0.,108.6)) ;
#42238 = CARTESIAN_POINT('',(-42.4,0.,108.6)) ;
#42239 = CARTESIAN_POINT('',(-42.4,13.6,108.6)) ;
#42240 = CARTESIAN_POINT('',(-42.4,0.4,108.6)) ;
#42241 = CARTESIAN_POINT('',(-42.4,0.,108.6)) ;
#42242 = CARTESIAN_POINT('',(-50.4984158167363,0.4,108.6)) ;
#42243 = CARTESIAN_POINT('',(0.,0.4,108.6)) ;
#42244 = CARTESIAN_POINT('',(-48.6342471926933,13.6,108.6)) ;
#42245 = CARTESIAN_POINT('Origin',(0.,0.,108.6)) ;
#42246 = CARTESIAN_POINT('',(0.,13.6,108.6)) ;
#42247 = CARTESIAN_POINT('',(-28.4,13.6,108.6)) ;
#42248 = CARTESIAN_POINT('',(-28.4,0.4,108.6)) ;
#42249 = CARTESIAN_POINT('',(-28.4,0.,108.6)) ;
#42250 = CARTESIAN_POINT('',(-41.6,0.4,108.6)) ;
#42251 = CARTESIAN_POINT('',(0.,0.4,108.6)) ;
#42252 = CARTESIAN_POINT('',(-41.6,13.6,108.6)) ;
#42253 = CARTESIAN_POINT('',(-41.6,0.,108.6)) ;
#42254 = CARTESIAN_POINT('',(0.,13.6,108.6)) ;
#42255 = CARTESIAN_POINT('',(-14.4,13.6,108.6)) ;
#42256 = CARTESIAN_POINT('',(-14.4,0.4,108.6)) ;
#42257 = CARTESIAN_POINT('',(-14.4,0.,108.6)) ;
#42258 = CARTESIAN_POINT('',(-27.6,0.4,108.6)) ;
#42259 = CARTESIAN_POINT('',(0.,0.4,108.6)) ;
#42260 = CARTESIAN_POINT('',(-27.6,13.6,108.6)) ;
#42261 = CARTESIAN_POINT('',(-27.6,0.,108.6)) ;
#42262 = CARTESIAN_POINT('',(0.,13.6,108.6)) ;
#42263 = CARTESIAN_POINT('',(-0.4,13.6,108.6)) ;
#42264 = CARTESIAN_POINT('',(-0.4,0.4,108.6)) ;
#42265 = CARTESIAN_POINT('',(-0.4,0.,108.6)) ;
#42266 = CARTESIAN_POINT('',(-13.6,0.4,108.6)) ;
#42267 = CARTESIAN_POINT('',(0.,0.4,108.6)) ;
#42268 = CARTESIAN_POINT('',(-13.6,13.6,108.6)) ;
#42269 = CARTESIAN_POINT('',(-13.6,0.,108.6)) ;
#42270 = CARTESIAN_POINT('',(0.,13.6,108.6)) ;
#42271 = CARTESIAN_POINT('',(13.6,-28.4,108.6)) ;
#42272 = CARTESIAN_POINT('',(13.6,-41.6,108.6)) ;
#42273 = CARTESIAN_POINT('',(13.6,0.,108.6)) ;
#42274 = CARTESIAN_POINT('',(0.4,-41.6,108.6)) ;
#42275 = CARTESIAN_POINT('',(0.,-41.6,108.6)) ;
#42276 = CARTESIAN_POINT('',(0.4,-28.4,108.6)) ;
#42277 = CARTESIAN_POINT('',(0.4,0.,108.6)) ;
#42278 = CARTESIAN_POINT('',(0.,-28.4,108.6)) ;
#42279 = CARTESIAN_POINT('',(13.6,-14.4,108.6)) ;
#42280 = CARTESIAN_POINT('',(13.6,-27.6,108.6)) ;
#42281 = CARTESIAN_POINT('',(13.6,0.,108.6)) ;
#42282 = CARTESIAN_POINT('',(0.4,-27.6,108.6)) ;
#42283 = CARTESIAN_POINT('',(0.,-27.6,108.6)) ;
#42284 = CARTESIAN_POINT('',(0.4,-14.4,108.6)) ;
#42285 = CARTESIAN_POINT('',(0.4,0.,108.6)) ;
#42286 = CARTESIAN_POINT('',(0.,-14.4,108.6)) ;
#42287 = CARTESIAN_POINT('',(13.6,-0.4,108.6)) ;
#42288 = CARTESIAN_POINT('',(13.6,-13.6,108.6)) ;
#42289 = CARTESIAN_POINT('',(13.6,0.,108.6)) ;
#42290 = CARTESIAN_POINT('',(0.4,-13.6,108.6)) ;
#42291 = CARTESIAN_POINT('',(0.,-13.6,108.6)) ;
#42292 = CARTESIAN_POINT('',(0.4,-0.4,108.6)) ;
#42293 = CARTESIAN_POINT('',(0.4,0.,108.6)) ;
#42294 = CARTESIAN_POINT('',(0.,-0.4,108.6)) ;
#42295 = CARTESIAN_POINT('',(14.4,-48.4034089708566,108.6)) ;
#42296 = CARTESIAN_POINT('',(14.4,-42.4,108.6)) ;
#42297 = CARTESIAN_POINT('',(14.4,0.,108.6)) ;
#42298 = CARTESIAN_POINT('',(27.4315511774307,-42.4,108.6)) ;
#42299 = CARTESIAN_POINT('',(0.,-42.4,108.6)) ;
#42300 = CARTESIAN_POINT('Origin',(0.,0.,108.6)) ;
#42301 = CARTESIAN_POINT('',(13.6,13.6,108.6)) ;
#42302 = CARTESIAN_POINT('',(13.6,0.4,108.6)) ;
#42303 = CARTESIAN_POINT('',(13.6,0.,108.6)) ;
#42304 = CARTESIAN_POINT('',(0.4,0.4,108.6)) ;
#42305 = CARTESIAN_POINT('',(0.,0.4,108.6)) ;
#42306 = CARTESIAN_POINT('',(0.4,13.6,108.6)) ;
#42307 = CARTESIAN_POINT('',(0.4,0.,108.6)) ;
#42308 = CARTESIAN_POINT('',(0.,13.6,108.6)) ;
#42309 = CARTESIAN_POINT('',(13.6,-48.6342471926933,108.6)) ;
#42310 = CARTESIAN_POINT('',(0.4,-50.4984158167363,108.6)) ;
#42311 = CARTESIAN_POINT('Origin',(0.,0.,108.6)) ;
#42312 = CARTESIAN_POINT('',(0.4,-42.4,108.6)) ;
#42313 = CARTESIAN_POINT('',(0.4,0.,108.6)) ;
#42314 = CARTESIAN_POINT('',(13.6,-42.4,108.6)) ;
#42315 = CARTESIAN_POINT('',(0.,-42.4,108.6)) ;
#42316 = CARTESIAN_POINT('',(13.6,0.,108.6)) ;
#42317 = CARTESIAN_POINT('',(-41.6,27.6,108.6)) ;
#42318 = CARTESIAN_POINT('',(-28.4,27.6,108.6)) ;
#42319 = CARTESIAN_POINT('',(0.,27.6,108.6)) ;
#42320 = CARTESIAN_POINT('',(-28.4,14.4,108.6)) ;
#42321 = CARTESIAN_POINT('',(-28.4,0.,108.6)) ;
#42322 = CARTESIAN_POINT('',(-41.6,14.4,108.6)) ;
#42323 = CARTESIAN_POINT('',(0.,14.4,108.6)) ;
#42324 = CARTESIAN_POINT('',(-41.6,0.,108.6)) ;
#42325 = CARTESIAN_POINT('',(-14.4,27.6,108.6)) ;
#42326 = CARTESIAN_POINT('',(-14.4,14.4,108.6)) ;
#42327 = CARTESIAN_POINT('',(-14.4,0.,108.6)) ;
#42328 = CARTESIAN_POINT('',(-27.6,14.4,108.6)) ;
#42329 = CARTESIAN_POINT('',(0.,14.4,108.6)) ;
#42330 = CARTESIAN_POINT('',(-27.6,27.6,108.6)) ;
#42331 = CARTESIAN_POINT('',(-27.6,0.,108.6)) ;
#42332 = CARTESIAN_POINT('',(0.,27.6,108.6)) ;
#42333 = CARTESIAN_POINT('',(-0.4,27.6,108.6)) ;
#42334 = CARTESIAN_POINT('',(-0.4,14.4,108.6)) ;
#42335 = CARTESIAN_POINT('',(-0.4,0.,108.6)) ;
#42336 = CARTESIAN_POINT('',(-13.6,14.4,108.6)) ;
#42337 = CARTESIAN_POINT('',(0.,14.4,108.6)) ;
#42338 = CARTESIAN_POINT('',(-13.6,27.6,108.6)) ;
#42339 = CARTESIAN_POINT('',(-13.6,0.,108.6)) ;
#42340 = CARTESIAN_POINT('',(0.,27.6,108.6)) ;
#42341 = CARTESIAN_POINT('',(13.6,27.6,108.6)) ;
#42342 = CARTESIAN_POINT('',(13.6,14.4,108.6)) ;
#42343 = CARTESIAN_POINT('',(13.6,0.,108.6)) ;
#42344 = CARTESIAN_POINT('',(0.4,14.4,108.6)) ;
#42345 = CARTESIAN_POINT('',(0.,14.4,108.6)) ;
#42346 = CARTESIAN_POINT('',(0.4,27.6,108.6)) ;
#42347 = CARTESIAN_POINT('',(0.4,0.,108.6)) ;
#42348 = CARTESIAN_POINT('',(0.,27.6,108.6)) ;
#42349 = CARTESIAN_POINT('',(27.6,-28.4,108.6)) ;
#42350 = CARTESIAN_POINT('',(27.6,-41.6,108.6)) ;
#42351 = CARTESIAN_POINT('',(27.6,0.,108.6)) ;
#42352 = CARTESIAN_POINT('',(14.4,-41.6,108.6)) ;
#42353 = CARTESIAN_POINT('',(0.,-41.6,108.6)) ;
#42354 = CARTESIAN_POINT('',(14.4,-28.4,108.6)) ;
#42355 = CARTESIAN_POINT('',(14.4,0.,108.6)) ;
#42356 = CARTESIAN_POINT('',(0.,-28.4,108.6)) ;
#42357 = CARTESIAN_POINT('',(27.6,-14.4,108.6)) ;
#42358 = CARTESIAN_POINT('',(27.6,-27.6,108.6)) ;
#42359 = CARTESIAN_POINT('',(27.6,0.,108.6)) ;
#42360 = CARTESIAN_POINT('',(14.4,-27.6,108.6)) ;
#42361 = CARTESIAN_POINT('',(0.,-27.6,108.6)) ;
#42362 = CARTESIAN_POINT('',(14.4,-14.4,108.6)) ;
#42363 = CARTESIAN_POINT('',(14.4,0.,108.6)) ;
#42364 = CARTESIAN_POINT('',(0.,-14.4,108.6)) ;
#42365 = CARTESIAN_POINT('',(27.6,-0.4,108.6)) ;
#42366 = CARTESIAN_POINT('',(27.6,-13.6,108.6)) ;
#42367 = CARTESIAN_POINT('',(27.6,0.,108.6)) ;
#42368 = CARTESIAN_POINT('',(14.4,-13.6,108.6)) ;
#42369 = CARTESIAN_POINT('',(0.,-13.6,108.6)) ;
#42370 = CARTESIAN_POINT('',(14.4,-0.4,108.6)) ;
#42371 = CARTESIAN_POINT('',(14.4,0.,108.6)) ;
#42372 = CARTESIAN_POINT('',(0.,-0.4,108.6)) ;
#42373 = CARTESIAN_POINT('',(27.6,13.6,108.6)) ;
#42374 = CARTESIAN_POINT('',(27.6,0.4,108.6)) ;
#42375 = CARTESIAN_POINT('',(27.6,0.,108.6)) ;
#42376 = CARTESIAN_POINT('',(14.4,0.4,108.6)) ;
#42377 = CARTESIAN_POINT('',(0.,0.4,108.6)) ;
#42378 = CARTESIAN_POINT('',(14.4,13.6,108.6)) ;
#42379 = CARTESIAN_POINT('',(14.4,0.,108.6)) ;
#42380 = CARTESIAN_POINT('',(0.,13.6,108.6)) ;
#42381 = CARTESIAN_POINT('',(27.6,27.6,108.6)) ;
#42382 = CARTESIAN_POINT('',(27.6,14.4,108.6)) ;
#42383 = CARTESIAN_POINT('',(27.6,0.,108.6)) ;
#42384 = CARTESIAN_POINT('',(14.4,14.4,108.6)) ;
#42385 = CARTESIAN_POINT('',(0.,14.4,108.6)) ;
#42386 = CARTESIAN_POINT('',(14.4,27.6,108.6)) ;
#42387 = CARTESIAN_POINT('',(14.4,0.,108.6)) ;
#42388 = CARTESIAN_POINT('',(0.,27.6,108.6)) ;
#42389 = CARTESIAN_POINT('',(28.6302287800849,-41.6,108.6)) ;
#42390 = CARTESIAN_POINT('Origin',(0.,0.,108.6)) ;
#42391 = CARTESIAN_POINT('',(28.4,-41.6,108.6)) ;
#42392 = CARTESIAN_POINT('',(0.,-41.6,108.6)) ;
#42393 = CARTESIAN_POINT('',(28.4,-28.4,108.6)) ;
#42394 = CARTESIAN_POINT('',(28.4,0.,108.6)) ;
#42395 = CARTESIAN_POINT('',(0.,-28.4,108.6)) ;
#42396 = CARTESIAN_POINT('Origin',(0.,0.,108.3)) ;
#42397 = CARTESIAN_POINT('',(28.6302287800849,-41.6,108.)) ;
#42398 = CARTESIAN_POINT('Origin',(0.,0.,108.)) ;
#42399 = CARTESIAN_POINT('',(28.6302287800849,-41.6,108.3)) ;
#42400 = CARTESIAN_POINT('Origin',(0.,0.,108.)) ;
#42401 = CARTESIAN_POINT('',(43.2232576282723,28.4,108.)) ;
#42402 = CARTESIAN_POINT('',(0.,28.4,108.)) ;
#42403 = CARTESIAN_POINT('',(43.2232576282723,28.,108.)) ;
#42404 = CARTESIAN_POINT('',(43.2232576282723,28.,108.)) ;
#42405 = CARTESIAN_POINT('',(49.4458289444115,14.4,108.)) ;
#42406 = CARTESIAN_POINT('Origin',(0.,0.,108.)) ;
#42407 = CARTESIAN_POINT('',(49.5605690039975,14.4,108.)) ;
#42408 = CARTESIAN_POINT('',(0.,14.4,108.)) ;
#42409 = CARTESIAN_POINT('',(49.5605690039975,14.,108.)) ;
#42410 = CARTESIAN_POINT('',(49.5605690039975,14.,108.)) ;
#42411 = CARTESIAN_POINT('',(51.4984465785134,0.4,108.)) ;
#42412 = CARTESIAN_POINT('Origin',(0.,0.,108.)) ;
#42413 = CARTESIAN_POINT('',(51.5,0.4,108.)) ;
#42414 = CARTESIAN_POINT('',(0.,0.4,108.)) ;
#42415 = CARTESIAN_POINT('',(51.5,-0.4,108.)) ;
#42416 = CARTESIAN_POINT('',(51.5,0.,108.)) ;
#42417 = CARTESIAN_POINT('',(51.4984465785134,-0.4,108.)) ;
#42418 = CARTESIAN_POINT('',(0.,-0.4,108.)) ;
#42419 = CARTESIAN_POINT('',(49.5605690039975,-14.,108.)) ;
#42420 = CARTESIAN_POINT('Origin',(0.,0.,108.)) ;
#42421 = CARTESIAN_POINT('',(49.5605690039975,-14.4,108.)) ;
#42422 = CARTESIAN_POINT('',(49.5605690039975,-14.,108.)) ;
#42423 = CARTESIAN_POINT('',(49.4458289444115,-14.4,108.)) ;
#42424 = CARTESIAN_POINT('',(0.,-14.4,108.)) ;
#42425 = CARTESIAN_POINT('',(43.2232576282723,-28.,108.)) ;
#42426 = CARTESIAN_POINT('Origin',(0.,0.,108.)) ;
#42427 = CARTESIAN_POINT('',(43.2232576282723,-28.4,108.)) ;
#42428 = CARTESIAN_POINT('',(43.2232576282723,-28.,108.)) ;
#42429 = CARTESIAN_POINT('',(42.9614943874163,-28.4,108.)) ;
#42430 = CARTESIAN_POINT('',(0.,-28.4,108.)) ;
#42431 = CARTESIAN_POINT('Origin',(0.,0.,108.)) ;
#42432 = CARTESIAN_POINT('',(29.8035232816525,-42.,108.)) ;
#42433 = CARTESIAN_POINT('Origin',(0.,0.,108.)) ;
#42434 = CARTESIAN_POINT('',(29.8035232816525,-42.4,108.)) ;
#42435 = CARTESIAN_POINT('',(29.8035232816525,-42.,108.)) ;
#42436 = CARTESIAN_POINT('',(29.2316609175736,-42.4,108.)) ;
#42437 = CARTESIAN_POINT('',(0.,-42.4,108.)) ;
#42438 = CARTESIAN_POINT('',(28.4,-42.9614943874163,108.)) ;
#42439 = CARTESIAN_POINT('Origin',(0.,0.,108.)) ;
#42440 = CARTESIAN_POINT('',(28.4,-43.2232576282723,108.)) ;
#42441 = CARTESIAN_POINT('',(28.4,0.,108.)) ;
#42442 = CARTESIAN_POINT('',(28.,-43.2232576282723,108.)) ;
#42443 = CARTESIAN_POINT('',(28.,-43.2232576282723,108.)) ;
#42444 = CARTESIAN_POINT('',(14.4,-49.4458289444115,108.)) ;
#42445 = CARTESIAN_POINT('Origin',(0.,0.,108.)) ;
#42446 = CARTESIAN_POINT('',(14.4,-49.5605690039975,108.)) ;
#42447 = CARTESIAN_POINT('',(14.4,0.,108.)) ;
#42448 = CARTESIAN_POINT('',(14.,-49.5605690039975,108.)) ;
#42449 = CARTESIAN_POINT('',(14.,-49.5605690039975,108.)) ;
#42450 = CARTESIAN_POINT('',(0.4,-51.4984465785134,108.)) ;
#42451 = CARTESIAN_POINT('Origin',(0.,0.,108.)) ;
#42452 = CARTESIAN_POINT('',(0.4,-51.5,108.)) ;
#42453 = CARTESIAN_POINT('',(0.4,0.,108.)) ;
#42454 = CARTESIAN_POINT('',(-0.4,-51.5,108.)) ;
#42455 = CARTESIAN_POINT('',(0.,-51.5,108.)) ;
#42456 = CARTESIAN_POINT('',(-0.4,-51.4984465785134,108.)) ;
#42457 = CARTESIAN_POINT('',(-0.4,0.,108.)) ;
#42458 = CARTESIAN_POINT('',(-14.,-49.5605690039975,108.)) ;
#42459 = CARTESIAN_POINT('Origin',(0.,0.,108.)) ;
#42460 = CARTESIAN_POINT('',(-14.4,-49.5605690039975,108.)) ;
#42461 = CARTESIAN_POINT('',(-14.,-49.5605690039975,108.)) ;
#42462 = CARTESIAN_POINT('',(-14.4,-49.4458289444115,108.)) ;
#42463 = CARTESIAN_POINT('',(-14.4,0.,108.)) ;
#42464 = CARTESIAN_POINT('',(-28.,-43.2232576282723,108.)) ;
#42465 = CARTESIAN_POINT('Origin',(0.,0.,108.)) ;
#42466 = CARTESIAN_POINT('',(-28.4,-43.2232576282723,108.)) ;
#42467 = CARTESIAN_POINT('',(-28.,-43.2232576282723,108.)) ;
#42468 = CARTESIAN_POINT('',(-28.4,-42.9614943874163,108.)) ;
#42469 = CARTESIAN_POINT('',(-28.4,0.,108.)) ;
#42470 = CARTESIAN_POINT('',(-29.2316609175736,-42.4,108.)) ;
#42471 = CARTESIAN_POINT('Origin',(0.,0.,108.)) ;
#42472 = CARTESIAN_POINT('',(-29.8035232816525,-42.4,108.)) ;
#42473 = CARTESIAN_POINT('',(0.,-42.4,108.)) ;
#42474 = CARTESIAN_POINT('',(-29.8035232816525,-42.,108.)) ;
#42475 = CARTESIAN_POINT('',(-29.8035232816525,-42.,108.)) ;
#42476 = CARTESIAN_POINT('',(-42.,-29.8035232816525,108.)) ;
#42477 = CARTESIAN_POINT('Origin',(0.,0.,108.)) ;
#42478 = CARTESIAN_POINT('',(-42.4,-29.8035232816525,108.)) ;
#42479 = CARTESIAN_POINT('',(-42.,-29.8035232816525,108.)) ;
#42480 = CARTESIAN_POINT('',(-42.4,-29.2316609175736,108.)) ;
#42481 = CARTESIAN_POINT('',(-42.4,0.,108.)) ;
#42482 = CARTESIAN_POINT('',(-42.9614943874163,-28.4,108.)) ;
#42483 = CARTESIAN_POINT('Origin',(0.,0.,108.)) ;
#42484 = CARTESIAN_POINT('',(-43.2232576282723,-28.4,108.)) ;
#42485 = CARTESIAN_POINT('',(0.,-28.4,108.)) ;
#42486 = CARTESIAN_POINT('',(-43.2232576282723,-28.,108.)) ;
#42487 = CARTESIAN_POINT('',(-43.2232576282723,-28.,108.)) ;
#42488 = CARTESIAN_POINT('',(-49.4458289444115,-14.4,108.)) ;
#42489 = CARTESIAN_POINT('Origin',(0.,0.,108.)) ;
#42490 = CARTESIAN_POINT('',(-49.5605690039975,-14.4,108.)) ;
#42491 = CARTESIAN_POINT('',(0.,-14.4,108.)) ;
#42492 = CARTESIAN_POINT('',(-49.5605690039975,-14.,108.)) ;
#42493 = CARTESIAN_POINT('',(-49.5605690039975,-14.,108.)) ;
#42494 = CARTESIAN_POINT('',(-51.4984465785134,-0.4,108.)) ;
#42495 = CARTESIAN_POINT('Origin',(0.,0.,108.)) ;
#42496 = CARTESIAN_POINT('',(-51.5,-0.4,108.)) ;
#42497 = CARTESIAN_POINT('',(0.,-0.4,108.)) ;
#42498 = CARTESIAN_POINT('',(-51.5,0.4,108.)) ;
#42499 = CARTESIAN_POINT('',(-51.5,0.,108.)) ;
#42500 = CARTESIAN_POINT('',(-51.4984465785134,0.4,108.)) ;
#42501 = CARTESIAN_POINT('',(0.,0.4,108.)) ;
#42502 = CARTESIAN_POINT('',(-49.5605690039975,14.,108.)) ;
#42503 = CARTESIAN_POINT('Origin',(0.,0.,108.)) ;
#42504 = CARTESIAN_POINT('',(-49.5605690039975,14.4,108.)) ;
#42505 = CARTESIAN_POINT('',(-49.5605690039975,14.,108.)) ;
#42506 = CARTESIAN_POINT('',(-49.4458289444115,14.4,108.)) ;
#42507 = CARTESIAN_POINT('',(0.,14.4,108.)) ;
#42508 = CARTESIAN_POINT('',(-43.2232576282723,28.,108.)) ;
#42509 = CARTESIAN_POINT('Origin',(0.,0.,108.)) ;
#42510 = CARTESIAN_POINT('',(-43.2232576282723,28.4,108.)) ;
#42511 = CARTESIAN_POINT('',(-43.2232576282723,28.,108.)) ;
#42512 = CARTESIAN_POINT('',(-42.9614943874163,28.4,108.)) ;
#42513 = CARTESIAN_POINT('',(0.,28.4,108.)) ;
#42514 = CARTESIAN_POINT('',(-42.4,29.2316609175736,108.)) ;
#42515 = CARTESIAN_POINT('Origin',(0.,0.,108.)) ;
#42516 = CARTESIAN_POINT('',(-42.4,29.8035232816525,108.)) ;
#42517 = CARTESIAN_POINT('',(-42.4,0.,108.)) ;
#42518 = CARTESIAN_POINT('',(-42.,29.8035232816525,108.)) ;
#42519 = CARTESIAN_POINT('',(-42.,29.8035232816525,108.)) ;
#42520 = CARTESIAN_POINT('',(-29.8035232816525,42.,108.)) ;
#42521 = CARTESIAN_POINT('Origin',(0.,0.,108.)) ;
#42522 = CARTESIAN_POINT('',(-29.8035232816525,42.4,108.)) ;
#42523 = CARTESIAN_POINT('',(-29.8035232816525,42.,108.)) ;
#42524 = CARTESIAN_POINT('',(-29.2316609175736,42.4,108.)) ;
#42525 = CARTESIAN_POINT('',(0.,42.4,108.)) ;
#42526 = CARTESIAN_POINT('',(-28.4,42.9614943874163,108.)) ;
#42527 = CARTESIAN_POINT('Origin',(0.,0.,108.)) ;
#42528 = CARTESIAN_POINT('',(-28.4,43.2232576282723,108.)) ;
#42529 = CARTESIAN_POINT('',(-28.4,0.,108.)) ;
#42530 = CARTESIAN_POINT('',(-28.,43.2232576282723,108.)) ;
#42531 = CARTESIAN_POINT('',(-28.,43.2232576282723,108.)) ;
#42532 = CARTESIAN_POINT('',(-14.4,49.4458289444115,108.)) ;
#42533 = CARTESIAN_POINT('Origin',(0.,0.,108.)) ;
#42534 = CARTESIAN_POINT('',(-14.4,49.5605690039975,108.)) ;
#42535 = CARTESIAN_POINT('',(-14.4,0.,108.)) ;
#42536 = CARTESIAN_POINT('',(-14.,49.5605690039975,108.)) ;
#42537 = CARTESIAN_POINT('',(-14.,49.5605690039975,108.)) ;
#42538 = CARTESIAN_POINT('',(-0.4,51.4984465785134,108.)) ;
#42539 = CARTESIAN_POINT('Origin',(0.,0.,108.)) ;
#42540 = CARTESIAN_POINT('',(-0.4,51.5,108.)) ;
#42541 = CARTESIAN_POINT('',(-0.4,0.,108.)) ;
#42542 = CARTESIAN_POINT('',(0.4,51.5,108.)) ;
#42543 = CARTESIAN_POINT('',(0.,51.5,108.)) ;
#42544 = CARTESIAN_POINT('',(0.4,51.4984465785134,108.)) ;
#42545 = CARTESIAN_POINT('',(0.4,0.,108.)) ;
#42546 = CARTESIAN_POINT('',(14.,49.5605690039975,108.)) ;
#42547 = CARTESIAN_POINT('Origin',(0.,0.,108.)) ;
#42548 = CARTESIAN_POINT('',(14.4,49.5605690039975,108.)) ;
#42549 = CARTESIAN_POINT('',(14.,49.5605690039975,108.)) ;
#42550 = CARTESIAN_POINT('',(14.4,49.4458289444115,108.)) ;
#42551 = CARTESIAN_POINT('',(14.4,0.,108.)) ;
#42552 = CARTESIAN_POINT('',(28.,43.2232576282723,108.)) ;
#42553 = CARTESIAN_POINT('Origin',(0.,0.,108.)) ;
#42554 = CARTESIAN_POINT('',(28.4,43.2232576282723,108.)) ;
#42555 = CARTESIAN_POINT('',(28.,43.2232576282723,108.)) ;
#42556 = CARTESIAN_POINT('',(28.4,42.9614943874163,108.)) ;
#42557 = CARTESIAN_POINT('',(28.4,0.,108.)) ;
#42558 = CARTESIAN_POINT('',(29.2316609175736,42.4,108.)) ;
#42559 = CARTESIAN_POINT('Origin',(0.,0.,108.)) ;
#42560 = CARTESIAN_POINT('',(29.8035232816525,42.4,108.)) ;
#42561 = CARTESIAN_POINT('',(0.,42.4,108.)) ;
#42562 = CARTESIAN_POINT('',(29.8035232816525,42.,108.)) ;
#42563 = CARTESIAN_POINT('',(28.4,27.6,108.)) ;
#42564 = CARTESIAN_POINT('',(0.,27.6,108.)) ;
#42565 = CARTESIAN_POINT('',(28.4,0.,108.)) ;
#42566 = CARTESIAN_POINT('',(28.4,13.6,108.)) ;
#42567 = CARTESIAN_POINT('',(0.,13.6,108.)) ;
#42568 = CARTESIAN_POINT('',(28.4,0.,108.)) ;
#42569 = CARTESIAN_POINT('',(28.4,-0.4,108.)) ;
#42570 = CARTESIAN_POINT('',(0.,-0.4,108.)) ;
#42571 = CARTESIAN_POINT('',(28.4,0.,108.)) ;
#42572 = CARTESIAN_POINT('',(28.4,-14.4,108.)) ;
#42573 = CARTESIAN_POINT('',(0.,-14.4,108.)) ;
#42574 = CARTESIAN_POINT('',(28.4,0.,108.)) ;
#42575 = CARTESIAN_POINT('',(28.6302287800849,41.6,108.)) ;
#42576 = CARTESIAN_POINT('Origin',(0.,0.,108.)) ;
#42577 = CARTESIAN_POINT('',(28.4,41.6,108.)) ;
#42578 = CARTESIAN_POINT('',(0.,41.6,108.)) ;
#42579 = CARTESIAN_POINT('',(28.4,0.,108.)) ;
#42580 = CARTESIAN_POINT('',(50.4984158167363,0.4,108.)) ;
#42581 = CARTESIAN_POINT('',(0.,0.4,108.)) ;
#42582 = CARTESIAN_POINT('Origin',(0.,0.,108.)) ;
#42583 = CARTESIAN_POINT('',(48.6342471926933,-13.6,108.)) ;
#42584 = CARTESIAN_POINT('',(0.,-13.6,108.)) ;
#42585 = CARTESIAN_POINT('Origin',(0.,0.,108.)) ;
#42586 = CARTESIAN_POINT('Origin',(0.,0.,108.)) ;
#42587 = CARTESIAN_POINT('',(28.4,-28.4,108.)) ;
#42588 = CARTESIAN_POINT('',(0.,-28.4,108.)) ;
#42589 = CARTESIAN_POINT('',(28.4,-41.6,108.)) ;
#42590 = CARTESIAN_POINT('',(28.4,0.,108.)) ;
#42591 = CARTESIAN_POINT('',(0.,-41.6,108.)) ;
#42592 = CARTESIAN_POINT('',(0.,14.4,108.)) ;
#42593 = CARTESIAN_POINT('',(-28.4,41.6,108.)) ;
#42594 = CARTESIAN_POINT('',(-28.6302287800849,41.6,108.)) ;
#42595 = CARTESIAN_POINT('',(0.,41.6,108.)) ;
#42596 = CARTESIAN_POINT('',(-41.6,28.6302287800849,108.)) ;
#42597 = CARTESIAN_POINT('Origin',(0.,0.,108.)) ;
#42598 = CARTESIAN_POINT('',(-41.6,28.4,108.)) ;
#42599 = CARTESIAN_POINT('',(-41.6,0.,108.)) ;
#42600 = CARTESIAN_POINT('',(-28.4,28.4,108.)) ;
#42601 = CARTESIAN_POINT('',(0.,28.4,108.)) ;
#42602 = CARTESIAN_POINT('',(-28.4,0.,108.)) ;
#42603 = CARTESIAN_POINT('',(-41.6,27.6,108.)) ;
#42604 = CARTESIAN_POINT('',(-41.6,14.4,108.)) ;
#42605 = CARTESIAN_POINT('',(-41.6,0.,108.)) ;
#42606 = CARTESIAN_POINT('',(-28.4,14.4,108.)) ;
#42607 = CARTESIAN_POINT('',(0.,14.4,108.)) ;
#42608 = CARTESIAN_POINT('',(-28.4,27.6,108.)) ;
#42609 = CARTESIAN_POINT('',(-28.4,0.,108.)) ;
#42610 = CARTESIAN_POINT('',(0.,27.6,108.)) ;
#42611 = CARTESIAN_POINT('',(13.6,27.6,108.)) ;
#42612 = CARTESIAN_POINT('',(0.4,27.6,108.)) ;
#42613 = CARTESIAN_POINT('',(0.,27.6,108.)) ;
#42614 = CARTESIAN_POINT('',(0.4,14.4,108.)) ;
#42615 = CARTESIAN_POINT('',(0.4,0.,108.)) ;
#42616 = CARTESIAN_POINT('',(13.6,14.4,108.)) ;
#42617 = CARTESIAN_POINT('',(0.,14.4,108.)) ;
#42618 = CARTESIAN_POINT('',(13.6,0.,108.)) ;
#42619 = CARTESIAN_POINT('',(-0.4,27.6,108.)) ;
#42620 = CARTESIAN_POINT('',(-13.6,27.6,108.)) ;
#42621 = CARTESIAN_POINT('',(0.,27.6,108.)) ;
#42622 = CARTESIAN_POINT('',(-13.6,14.4,108.)) ;
#42623 = CARTESIAN_POINT('',(-13.6,0.,108.)) ;
#42624 = CARTESIAN_POINT('',(-0.4,14.4,108.)) ;
#42625 = CARTESIAN_POINT('',(0.,14.4,108.)) ;
#42626 = CARTESIAN_POINT('',(-0.4,0.,108.)) ;
#42627 = CARTESIAN_POINT('',(-14.4,27.6,108.)) ;
#42628 = CARTESIAN_POINT('',(-27.6,27.6,108.)) ;
#42629 = CARTESIAN_POINT('',(0.,27.6,108.)) ;
#42630 = CARTESIAN_POINT('',(-27.6,14.4,108.)) ;
#42631 = CARTESIAN_POINT('',(-27.6,0.,108.)) ;
#42632 = CARTESIAN_POINT('',(-14.4,14.4,108.)) ;
#42633 = CARTESIAN_POINT('',(0.,14.4,108.)) ;
#42634 = CARTESIAN_POINT('',(-14.4,0.,108.)) ;
#42635 = CARTESIAN_POINT('',(-42.4,14.4,108.)) ;
#42636 = CARTESIAN_POINT('',(-42.4,27.4315511774307,108.)) ;
#42637 = CARTESIAN_POINT('',(-42.4,0.,108.)) ;
#42638 = CARTESIAN_POINT('',(-48.4034089708566,14.4,108.)) ;
#42639 = CARTESIAN_POINT('Origin',(0.,0.,108.)) ;
#42640 = CARTESIAN_POINT('',(0.,14.4,108.)) ;
#42641 = CARTESIAN_POINT('',(-0.4,13.6,108.)) ;
#42642 = CARTESIAN_POINT('',(-13.6,13.6,108.)) ;
#42643 = CARTESIAN_POINT('',(0.,13.6,108.)) ;
#42644 = CARTESIAN_POINT('',(-13.6,0.4,108.)) ;
#42645 = CARTESIAN_POINT('',(-13.6,0.,108.)) ;
#42646 = CARTESIAN_POINT('',(-0.4,0.4,108.)) ;
#42647 = CARTESIAN_POINT('',(0.,0.4,108.)) ;
#42648 = CARTESIAN_POINT('',(-0.4,0.,108.)) ;
#42649 = CARTESIAN_POINT('',(-14.4,13.6,108.)) ;
#42650 = CARTESIAN_POINT('',(-27.6,13.6,108.)) ;
#42651 = CARTESIAN_POINT('',(0.,13.6,108.)) ;
#42652 = CARTESIAN_POINT('',(-27.6,0.4,108.)) ;
#42653 = CARTESIAN_POINT('',(-27.6,0.,108.)) ;
#42654 = CARTESIAN_POINT('',(-14.4,0.4,108.)) ;
#42655 = CARTESIAN_POINT('',(0.,0.4,108.)) ;
#42656 = CARTESIAN_POINT('',(-14.4,0.,108.)) ;
#42657 = CARTESIAN_POINT('',(-28.4,13.6,108.)) ;
#42658 = CARTESIAN_POINT('',(-41.6,13.6,108.)) ;
#42659 = CARTESIAN_POINT('',(0.,13.6,108.)) ;
#42660 = CARTESIAN_POINT('',(-41.6,0.4,108.)) ;
#42661 = CARTESIAN_POINT('',(-41.6,0.,108.)) ;
#42662 = CARTESIAN_POINT('',(-28.4,0.4,108.)) ;
#42663 = CARTESIAN_POINT('',(0.,0.4,108.)) ;
#42664 = CARTESIAN_POINT('',(-28.4,0.,108.)) ;
#42665 = CARTESIAN_POINT('',(-0.4,-0.4,108.)) ;
#42666 = CARTESIAN_POINT('',(-13.6,-0.4,108.)) ;
#42667 = CARTESIAN_POINT('',(0.,-0.4,108.)) ;
#42668 = CARTESIAN_POINT('',(-13.6,-13.6,108.)) ;
#42669 = CARTESIAN_POINT('',(-13.6,0.,108.)) ;
#42670 = CARTESIAN_POINT('',(-0.4,-13.6,108.)) ;
#42671 = CARTESIAN_POINT('',(0.,-13.6,108.)) ;
#42672 = CARTESIAN_POINT('',(-0.4,0.,108.)) ;
#42673 = CARTESIAN_POINT('',(-0.4,-14.4,108.)) ;
#42674 = CARTESIAN_POINT('',(-13.6,-14.4,108.)) ;
#42675 = CARTESIAN_POINT('',(0.,-14.4,108.)) ;
#42676 = CARTESIAN_POINT('',(-13.6,-27.6,108.)) ;
#42677 = CARTESIAN_POINT('',(-13.6,0.,108.)) ;
#42678 = CARTESIAN_POINT('',(-0.4,-27.6,108.)) ;
#42679 = CARTESIAN_POINT('',(0.,-27.6,108.)) ;
#42680 = CARTESIAN_POINT('',(-0.4,0.,108.)) ;
#42681 = CARTESIAN_POINT('',(-0.4,-28.4,108.)) ;
#42682 = CARTESIAN_POINT('',(-13.6,-28.4,108.)) ;
#42683 = CARTESIAN_POINT('',(0.,-28.4,108.)) ;
#42684 = CARTESIAN_POINT('',(-13.6,-41.6,108.)) ;
#42685 = CARTESIAN_POINT('',(-13.6,0.,108.)) ;
#42686 = CARTESIAN_POINT('',(-0.4,-41.6,108.)) ;
#42687 = CARTESIAN_POINT('',(0.,-41.6,108.)) ;
#42688 = CARTESIAN_POINT('',(-0.4,0.,108.)) ;
#42689 = CARTESIAN_POINT('',(-0.4,-50.4984158167363,108.)) ;
#42690 = CARTESIAN_POINT('',(-0.4,-42.4,108.)) ;
#42691 = CARTESIAN_POINT('',(-0.4,0.,108.)) ;
#42692 = CARTESIAN_POINT('',(-13.6,-42.4,108.)) ;
#42693 = CARTESIAN_POINT('',(0.,-42.4,108.)) ;
#42694 = CARTESIAN_POINT('',(-13.6,-48.6342471926933,108.)) ;
#42695 = CARTESIAN_POINT('',(-13.6,0.,108.)) ;
#42696 = CARTESIAN_POINT('Origin',(0.,0.,108.)) ;
#42697 = CARTESIAN_POINT('',(-42.4,-0.4,108.)) ;
#42698 = CARTESIAN_POINT('',(-50.4984158167363,-0.4,108.)) ;
#42699 = CARTESIAN_POINT('',(0.,-0.4,108.)) ;
#42700 = CARTESIAN_POINT('',(-48.6342471926933,-13.6,108.)) ;
#42701 = CARTESIAN_POINT('Origin',(0.,0.,108.)) ;
#42702 = CARTESIAN_POINT('',(-42.4,-13.6,108.)) ;
#42703 = CARTESIAN_POINT('',(0.,-13.6,108.)) ;
#42704 = CARTESIAN_POINT('',(-42.4,0.,108.)) ;
#42705 = CARTESIAN_POINT('',(-28.4,-28.4,108.)) ;
#42706 = CARTESIAN_POINT('',(-41.6,-28.4,108.)) ;
#42707 = CARTESIAN_POINT('',(0.,-28.4,108.)) ;
#42708 = CARTESIAN_POINT('',(-41.6,-28.6302287800849,108.)) ;
#42709 = CARTESIAN_POINT('',(-41.6,0.,108.)) ;
#42710 = CARTESIAN_POINT('',(-28.6302287800849,-41.6,108.)) ;
#42711 = CARTESIAN_POINT('Origin',(0.,0.,108.)) ;
#42712 = CARTESIAN_POINT('',(-28.4,-41.6,108.)) ;
#42713 = CARTESIAN_POINT('',(0.,-41.6,108.)) ;
#42714 = CARTESIAN_POINT('',(-28.4,0.,108.)) ;
#42715 = CARTESIAN_POINT('',(-42.4,-14.4,108.)) ;
#42716 = CARTESIAN_POINT('',(-48.4034089708566,-14.4,108.)) ;
#42717 = CARTESIAN_POINT('',(0.,-14.4,108.)) ;
#42718 = CARTESIAN_POINT('',(-42.4,-27.4315511774307,108.)) ;
#42719 = CARTESIAN_POINT('Origin',(0.,0.,108.)) ;
#42720 = CARTESIAN_POINT('',(-42.4,0.,108.)) ;
#42721 = CARTESIAN_POINT('',(-28.4,-14.4,108.)) ;
#42722 = CARTESIAN_POINT('',(-41.6,-14.4,108.)) ;
#42723 = CARTESIAN_POINT('',(0.,-14.4,108.)) ;
#42724 = CARTESIAN_POINT('',(-41.6,-27.6,108.)) ;
#42725 = CARTESIAN_POINT('',(-41.6,0.,108.)) ;
#42726 = CARTESIAN_POINT('',(-28.4,-27.6,108.)) ;
#42727 = CARTESIAN_POINT('',(0.,-27.6,108.)) ;
#42728 = CARTESIAN_POINT('',(-28.4,0.,108.)) ;
#42729 = CARTESIAN_POINT('',(-14.4,-42.4,108.)) ;
#42730 = CARTESIAN_POINT('',(-27.4315511774307,-42.4,108.)) ;
#42731 = CARTESIAN_POINT('',(0.,-42.4,108.)) ;
#42732 = CARTESIAN_POINT('',(-14.4,-48.4034089708566,108.)) ;
#42733 = CARTESIAN_POINT('Origin',(0.,0.,108.)) ;
#42734 = CARTESIAN_POINT('',(-14.4,0.,108.)) ;
#42735 = CARTESIAN_POINT('',(-14.4,-28.4,108.)) ;
#42736 = CARTESIAN_POINT('',(-27.6,-28.4,108.)) ;
#42737 = CARTESIAN_POINT('',(0.,-28.4,108.)) ;
#42738 = CARTESIAN_POINT('',(-27.6,-41.6,108.)) ;
#42739 = CARTESIAN_POINT('',(-27.6,0.,108.)) ;
#42740 = CARTESIAN_POINT('',(-14.4,-41.6,108.)) ;
#42741 = CARTESIAN_POINT('',(0.,-41.6,108.)) ;
#42742 = CARTESIAN_POINT('',(-14.4,0.,108.)) ;
#42743 = CARTESIAN_POINT('',(-14.4,-14.4,108.)) ;
#42744 = CARTESIAN_POINT('',(-27.6,-14.4,108.)) ;
#42745 = CARTESIAN_POINT('',(0.,-14.4,108.)) ;
#42746 = CARTESIAN_POINT('',(-27.6,-27.6,108.)) ;
#42747 = CARTESIAN_POINT('',(-27.6,0.,108.)) ;
#42748 = CARTESIAN_POINT('',(-14.4,-27.6,108.)) ;
#42749 = CARTESIAN_POINT('',(0.,-27.6,108.)) ;
#42750 = CARTESIAN_POINT('',(-14.4,0.,108.)) ;
#42751 = CARTESIAN_POINT('',(-28.4,-0.4,108.)) ;
#42752 = CARTESIAN_POINT('',(-41.6,-0.4,108.)) ;
#42753 = CARTESIAN_POINT('',(0.,-0.4,108.)) ;
#42754 = CARTESIAN_POINT('',(-41.6,-13.6,108.)) ;
#42755 = CARTESIAN_POINT('',(-41.6,0.,108.)) ;
#42756 = CARTESIAN_POINT('',(-28.4,-13.6,108.)) ;
#42757 = CARTESIAN_POINT('',(0.,-13.6,108.)) ;
#42758 = CARTESIAN_POINT('',(-28.4,0.,108.)) ;
#42759 = CARTESIAN_POINT('',(-14.4,-0.4,108.)) ;
#42760 = CARTESIAN_POINT('',(-27.6,-0.4,108.)) ;
#42761 = CARTESIAN_POINT('',(0.,-0.4,108.)) ;
#42762 = CARTESIAN_POINT('',(-27.6,-13.6,108.)) ;
#42763 = CARTESIAN_POINT('',(-27.6,0.,108.)) ;
#42764 = CARTESIAN_POINT('',(-14.4,-13.6,108.)) ;
#42765 = CARTESIAN_POINT('',(0.,-13.6,108.)) ;
#42766 = CARTESIAN_POINT('',(-14.4,0.,108.)) ;
#42767 = CARTESIAN_POINT('',(-42.4,13.6,108.)) ;
#42768 = CARTESIAN_POINT('',(-48.6342471926933,13.6,108.)) ;
#42769 = CARTESIAN_POINT('',(0.,13.6,108.)) ;
#42770 = CARTESIAN_POINT('',(-50.4984158167363,0.4,108.)) ;
#42771 = CARTESIAN_POINT('Origin',(0.,0.,108.)) ;
#42772 = CARTESIAN_POINT('',(-42.4,0.4,108.)) ;
#42773 = CARTESIAN_POINT('',(0.,0.4,108.)) ;
#42774 = CARTESIAN_POINT('',(-42.4,0.,108.)) ;
#42775 = CARTESIAN_POINT('',(13.6,-48.6342471926933,108.)) ;
#42776 = CARTESIAN_POINT('',(13.6,-42.4,108.)) ;
#42777 = CARTESIAN_POINT('',(13.6,0.,108.)) ;
#42778 = CARTESIAN_POINT('',(0.4,-42.4,108.)) ;
#42779 = CARTESIAN_POINT('',(0.,-42.4,108.)) ;
#42780 = CARTESIAN_POINT('',(0.4,-50.4984158167363,108.)) ;
#42781 = CARTESIAN_POINT('',(0.4,0.,108.)) ;
#42782 = CARTESIAN_POINT('Origin',(0.,0.,108.)) ;
#42783 = CARTESIAN_POINT('',(13.6,-28.4,108.)) ;
#42784 = CARTESIAN_POINT('',(0.4,-28.4,108.)) ;
#42785 = CARTESIAN_POINT('',(0.,-28.4,108.)) ;
#42786 = CARTESIAN_POINT('',(0.4,-41.6,108.)) ;
#42787 = CARTESIAN_POINT('',(0.4,0.,108.)) ;
#42788 = CARTESIAN_POINT('',(13.6,-41.6,108.)) ;
#42789 = CARTESIAN_POINT('',(0.,-41.6,108.)) ;
#42790 = CARTESIAN_POINT('',(13.6,0.,108.)) ;
#42791 = CARTESIAN_POINT('',(13.6,-14.4,108.)) ;
#42792 = CARTESIAN_POINT('',(0.4,-14.4,108.)) ;
#42793 = CARTESIAN_POINT('',(0.,-14.4,108.)) ;
#42794 = CARTESIAN_POINT('',(0.4,-27.6,108.)) ;
#42795 = CARTESIAN_POINT('',(0.4,0.,108.)) ;
#42796 = CARTESIAN_POINT('',(13.6,-27.6,108.)) ;
#42797 = CARTESIAN_POINT('',(0.,-27.6,108.)) ;
#42798 = CARTESIAN_POINT('',(13.6,0.,108.)) ;
#42799 = CARTESIAN_POINT('',(13.6,-0.4,108.)) ;
#42800 = CARTESIAN_POINT('',(0.4,-0.4,108.)) ;
#42801 = CARTESIAN_POINT('',(0.,-0.4,108.)) ;
#42802 = CARTESIAN_POINT('',(0.4,-13.6,108.)) ;
#42803 = CARTESIAN_POINT('',(0.4,0.,108.)) ;
#42804 = CARTESIAN_POINT('',(13.6,-13.6,108.)) ;
#42805 = CARTESIAN_POINT('',(0.,-13.6,108.)) ;
#42806 = CARTESIAN_POINT('',(13.6,0.,108.)) ;
#42807 = CARTESIAN_POINT('',(14.4,-48.4034089708566,108.)) ;
#42808 = CARTESIAN_POINT('',(27.4315511774307,-42.4,108.)) ;
#42809 = CARTESIAN_POINT('Origin',(0.,0.,108.)) ;
#42810 = CARTESIAN_POINT('',(14.4,-42.4,108.)) ;
#42811 = CARTESIAN_POINT('',(0.,-42.4,108.)) ;
#42812 = CARTESIAN_POINT('',(14.4,0.,108.)) ;
#42813 = CARTESIAN_POINT('',(13.6,13.6,108.)) ;
#42814 = CARTESIAN_POINT('',(0.4,13.6,108.)) ;
#42815 = CARTESIAN_POINT('',(0.,13.6,108.)) ;
#42816 = CARTESIAN_POINT('',(0.4,0.4,108.)) ;
#42817 = CARTESIAN_POINT('',(0.4,0.,108.)) ;
#42818 = CARTESIAN_POINT('',(13.6,0.4,108.)) ;
#42819 = CARTESIAN_POINT('',(0.,0.4,108.)) ;
#42820 = CARTESIAN_POINT('',(13.6,0.,108.)) ;
#42821 = CARTESIAN_POINT('',(27.6,-28.4,108.)) ;
#42822 = CARTESIAN_POINT('',(14.4,-28.4,108.)) ;
#42823 = CARTESIAN_POINT('',(0.,-28.4,108.)) ;
#42824 = CARTESIAN_POINT('',(14.4,-41.6,108.)) ;
#42825 = CARTESIAN_POINT('',(14.4,0.,108.)) ;
#42826 = CARTESIAN_POINT('',(27.6,-41.6,108.)) ;
#42827 = CARTESIAN_POINT('',(0.,-41.6,108.)) ;
#42828 = CARTESIAN_POINT('',(27.6,0.,108.)) ;
#42829 = CARTESIAN_POINT('',(27.6,-14.4,108.)) ;
#42830 = CARTESIAN_POINT('',(14.4,-14.4,108.)) ;
#42831 = CARTESIAN_POINT('',(0.,-14.4,108.)) ;
#42832 = CARTESIAN_POINT('',(14.4,-27.6,108.)) ;
#42833 = CARTESIAN_POINT('',(14.4,0.,108.)) ;
#42834 = CARTESIAN_POINT('',(27.6,-27.6,108.)) ;
#42835 = CARTESIAN_POINT('',(0.,-27.6,108.)) ;
#42836 = CARTESIAN_POINT('',(27.6,0.,108.)) ;
#42837 = CARTESIAN_POINT('',(27.6,-0.4,108.)) ;
#42838 = CARTESIAN_POINT('',(14.4,-0.4,108.)) ;
#42839 = CARTESIAN_POINT('',(0.,-0.4,108.)) ;
#42840 = CARTESIAN_POINT('',(14.4,-13.6,108.)) ;
#42841 = CARTESIAN_POINT('',(14.4,0.,108.)) ;
#42842 = CARTESIAN_POINT('',(27.6,-13.6,108.)) ;
#42843 = CARTESIAN_POINT('',(0.,-13.6,108.)) ;
#42844 = CARTESIAN_POINT('',(27.6,0.,108.)) ;
#42845 = CARTESIAN_POINT('',(27.6,13.6,108.)) ;
#42846 = CARTESIAN_POINT('',(14.4,13.6,108.)) ;
#42847 = CARTESIAN_POINT('',(0.,13.6,108.)) ;
#42848 = CARTESIAN_POINT('',(14.4,0.4,108.)) ;
#42849 = CARTESIAN_POINT('',(14.4,0.,108.)) ;
#42850 = CARTESIAN_POINT('',(27.6,0.4,108.)) ;
#42851 = CARTESIAN_POINT('',(0.,0.4,108.)) ;
#42852 = CARTESIAN_POINT('',(27.6,0.,108.)) ;
#42853 = CARTESIAN_POINT('',(27.6,27.6,108.)) ;
#42854 = CARTESIAN_POINT('',(14.4,27.6,108.)) ;
#42855 = CARTESIAN_POINT('',(0.,27.6,108.)) ;
#42856 = CARTESIAN_POINT('',(14.4,14.4,108.)) ;
#42857 = CARTESIAN_POINT('',(14.4,0.,108.)) ;
#42858 = CARTESIAN_POINT('',(27.6,14.4,108.)) ;
#42859 = CARTESIAN_POINT('',(0.,14.4,108.)) ;
#42860 = CARTESIAN_POINT('',(27.6,0.,108.)) ;
#42861 = CARTESIAN_POINT('',(-14.4,41.6,108.)) ;
#42862 = CARTESIAN_POINT('',(-27.6,41.6,108.)) ;
#42863 = CARTESIAN_POINT('',(0.,41.6,108.)) ;
#42864 = CARTESIAN_POINT('',(-27.6,28.4,108.)) ;
#42865 = CARTESIAN_POINT('',(-27.6,0.,108.)) ;
#42866 = CARTESIAN_POINT('',(-14.4,28.4,108.)) ;
#42867 = CARTESIAN_POINT('',(0.,28.4,108.)) ;
#42868 = CARTESIAN_POINT('',(-14.4,0.,108.)) ;
#42869 = CARTESIAN_POINT('',(-0.4,41.6,108.)) ;
#42870 = CARTESIAN_POINT('',(-13.6,41.6,108.)) ;
#42871 = CARTESIAN_POINT('',(0.,41.6,108.)) ;
#42872 = CARTESIAN_POINT('',(-13.6,28.4,108.)) ;
#42873 = CARTESIAN_POINT('',(-13.6,0.,108.)) ;
#42874 = CARTESIAN_POINT('',(-0.4,28.4,108.)) ;
#42875 = CARTESIAN_POINT('',(0.,28.4,108.)) ;
#42876 = CARTESIAN_POINT('',(-0.4,0.,108.)) ;
#42877 = CARTESIAN_POINT('',(13.6,41.6,108.)) ;
#42878 = CARTESIAN_POINT('',(0.4,41.6,108.)) ;
#42879 = CARTESIAN_POINT('',(0.,41.6,108.)) ;
#42880 = CARTESIAN_POINT('',(0.4,28.4,108.)) ;
#42881 = CARTESIAN_POINT('',(0.4,0.,108.)) ;
#42882 = CARTESIAN_POINT('',(13.6,28.4,108.)) ;
#42883 = CARTESIAN_POINT('',(0.,28.4,108.)) ;
#42884 = CARTESIAN_POINT('',(13.6,0.,108.)) ;
#42885 = CARTESIAN_POINT('',(14.4,42.4,108.)) ;
#42886 = CARTESIAN_POINT('',(27.4315511774307,42.4,108.)) ;
#42887 = CARTESIAN_POINT('',(0.,42.4,108.)) ;
#42888 = CARTESIAN_POINT('',(14.4,48.4034089708566,108.)) ;
#42889 = CARTESIAN_POINT('Origin',(0.,0.,108.)) ;
#42890 = CARTESIAN_POINT('',(14.4,0.,108.)) ;
#42891 = CARTESIAN_POINT('',(-14.4,42.4,108.)) ;
#42892 = CARTESIAN_POINT('',(-14.4,48.4034089708566,108.)) ;
#42893 = CARTESIAN_POINT('',(-14.4,0.,108.)) ;
#42894 = CARTESIAN_POINT('',(-27.4315511774307,42.4,108.)) ;
#42895 = CARTESIAN_POINT('Origin',(0.,0.,108.)) ;
#42896 = CARTESIAN_POINT('',(0.,42.4,108.)) ;
#42897 = CARTESIAN_POINT('',(-0.4,42.4,108.)) ;
#42898 = CARTESIAN_POINT('',(-0.4,50.4984158167363,108.)) ;
#42899 = CARTESIAN_POINT('',(-0.4,0.,108.)) ;
#42900 = CARTESIAN_POINT('',(-13.6,48.6342471926933,108.)) ;
#42901 = CARTESIAN_POINT('Origin',(0.,0.,108.)) ;
#42902 = CARTESIAN_POINT('',(-13.6,42.4,108.)) ;
#42903 = CARTESIAN_POINT('',(-13.6,0.,108.)) ;
#42904 = CARTESIAN_POINT('',(0.,42.4,108.)) ;
#42905 = CARTESIAN_POINT('',(13.6,42.4,108.)) ;
#42906 = CARTESIAN_POINT('',(13.6,48.6342471926933,108.)) ;
#42907 = CARTESIAN_POINT('',(13.6,0.,108.)) ;
#42908 = CARTESIAN_POINT('',(0.4,50.4984158167363,108.)) ;
#42909 = CARTESIAN_POINT('Origin',(0.,0.,108.)) ;
#42910 = CARTESIAN_POINT('',(0.4,42.4,108.)) ;
#42911 = CARTESIAN_POINT('',(0.4,0.,108.)) ;
#42912 = CARTESIAN_POINT('',(0.,42.4,108.)) ;
#42913 = CARTESIAN_POINT('',(14.4,41.6,108.)) ;
#42914 = CARTESIAN_POINT('',(14.4,28.4,108.)) ;
#42915 = CARTESIAN_POINT('',(14.4,0.,108.)) ;
#42916 = CARTESIAN_POINT('',(27.6,28.4,108.)) ;
#42917 = CARTESIAN_POINT('',(0.,28.4,108.)) ;
#42918 = CARTESIAN_POINT('',(27.6,41.6,108.)) ;
#42919 = CARTESIAN_POINT('',(27.6,0.,108.)) ;
#42920 = CARTESIAN_POINT('',(0.,41.6,108.)) ;
#42921 = CARTESIAN_POINT('Origin',(0.,0.,108.3)) ;
#42922 = CARTESIAN_POINT('',(29.8035232816525,-42.,108.3)) ;
#42923 = CARTESIAN_POINT('Origin',(0.,0.,108.3)) ;
#42924 = CARTESIAN_POINT('',(42.9614943874163,-28.4,108.3)) ;
#42925 = CARTESIAN_POINT('Origin',(29.8035232816525,42.,108.3)) ;
#42926 = CARTESIAN_POINT('',(29.8035232816525,42.4,108.3)) ;
#42927 = CARTESIAN_POINT('Origin',(0.,41.6,108.3)) ;
#42928 = CARTESIAN_POINT('',(-28.4,41.6,108.3)) ;
#42929 = CARTESIAN_POINT('',(-28.6302287800849,41.6,108.3)) ;
#42930 = CARTESIAN_POINT('Origin',(0.,41.6,108.3)) ;
#42931 = CARTESIAN_POINT('',(-14.4,41.6,108.3)) ;
#42932 = CARTESIAN_POINT('',(-27.6,41.6,108.3)) ;
#42933 = CARTESIAN_POINT('Origin',(0.,41.6,108.3)) ;
#42934 = CARTESIAN_POINT('',(-0.4,41.6,108.3)) ;
#42935 = CARTESIAN_POINT('',(-13.6,41.6,108.3)) ;
#42936 = CARTESIAN_POINT('Origin',(0.,41.6,108.3)) ;
#42937 = CARTESIAN_POINT('',(28.4,41.6,108.3)) ;
#42938 = CARTESIAN_POINT('',(28.6302287800849,41.6,108.3)) ;
#42939 = CARTESIAN_POINT('Origin',(0.,41.6,108.3)) ;
#42940 = CARTESIAN_POINT('',(14.4,41.6,108.3)) ;
#42941 = CARTESIAN_POINT('',(27.6,41.6,108.3)) ;
#42942 = CARTESIAN_POINT('Origin',(0.,41.6,108.3)) ;
#42943 = CARTESIAN_POINT('',(13.6,41.6,108.3)) ;
#42944 = CARTESIAN_POINT('',(0.4,41.6,108.3)) ;
#42945 = CARTESIAN_POINT('Origin',(0.,42.4,108.3)) ;
#42946 = CARTESIAN_POINT('',(-29.2316609175736,42.4,108.3)) ;
#42947 = CARTESIAN_POINT('',(-29.8035232816525,42.4,108.3)) ;
#42948 = CARTESIAN_POINT('Origin',(0.,42.4,108.3)) ;
#42949 = CARTESIAN_POINT('',(-14.4,42.4,108.3)) ;
#42950 = CARTESIAN_POINT('',(-27.4315511774307,42.4,108.3)) ;
#42951 = CARTESIAN_POINT('Origin',(0.,42.4,108.3)) ;
#42952 = CARTESIAN_POINT('',(-0.4,42.4,108.3)) ;
#42953 = CARTESIAN_POINT('',(-13.6,42.4,108.3)) ;
#42954 = CARTESIAN_POINT('Origin',(0.,42.4,108.3)) ;
#42955 = CARTESIAN_POINT('',(13.6,42.4,108.3)) ;
#42956 = CARTESIAN_POINT('',(0.4,42.4,108.3)) ;
#42957 = CARTESIAN_POINT('Origin',(0.,42.4,108.3)) ;
#42958 = CARTESIAN_POINT('',(29.2316609175736,42.4,108.3)) ;
#42959 = CARTESIAN_POINT('Origin',(-29.8035232816525,42.,108.3)) ;
#42960 = CARTESIAN_POINT('',(-29.8035232816525,42.,108.3)) ;
#42961 = CARTESIAN_POINT('Origin',(0.,42.4,108.3)) ;
#42962 = CARTESIAN_POINT('',(14.4,42.4,108.3)) ;
#42963 = CARTESIAN_POINT('',(27.4315511774307,42.4,108.3)) ;
#42964 = CARTESIAN_POINT('Origin',(14.4,0.,108.3)) ;
#42965 = CARTESIAN_POINT('',(14.4,48.4034089708566,108.3)) ;
#42966 = CARTESIAN_POINT('Origin',(13.6,0.,108.3)) ;
#42967 = CARTESIAN_POINT('',(13.6,28.4,108.3)) ;
#42968 = CARTESIAN_POINT('Origin',(27.6,0.,108.3)) ;
#42969 = CARTESIAN_POINT('',(27.6,28.4,108.3)) ;
#42970 = CARTESIAN_POINT('Origin',(0.,0.,108.3)) ;
#42971 = CARTESIAN_POINT('Origin',(0.,0.,108.3)) ;
#42972 = CARTESIAN_POINT('',(28.4,42.9614943874163,108.3)) ;
#42973 = CARTESIAN_POINT('Origin',(0.4,0.,108.3)) ;
#42974 = CARTESIAN_POINT('',(0.4,50.4984158167363,108.3)) ;
#42975 = CARTESIAN_POINT('Origin',(-0.4,0.,108.3)) ;
#42976 = CARTESIAN_POINT('',(-0.4,28.4,108.3)) ;
#42977 = CARTESIAN_POINT('Origin',(-13.6,0.,108.3)) ;
#42978 = CARTESIAN_POINT('',(-13.6,48.6342471926933,108.3)) ;
#42979 = CARTESIAN_POINT('Origin',(-14.4,0.,108.3)) ;
#42980 = CARTESIAN_POINT('',(-14.4,28.4,108.3)) ;
#42981 = CARTESIAN_POINT('Origin',(-28.4,0.,108.3)) ;
#42982 = CARTESIAN_POINT('',(-28.4,28.4,108.3)) ;
#42983 = CARTESIAN_POINT('Origin',(0.,0.,108.3)) ;
#42984 = CARTESIAN_POINT('',(-14.4,48.4034089708566,108.3)) ;
#42985 = CARTESIAN_POINT('Origin',(0.,0.,108.3)) ;
#42986 = CARTESIAN_POINT('',(-28.4,42.9614943874163,108.3)) ;
#42987 = CARTESIAN_POINT('Origin',(0.,0.,108.3)) ;
#42988 = CARTESIAN_POINT('',(-42.,29.8035232816525,108.3)) ;
#42989 = CARTESIAN_POINT('Origin',(28.,-43.2232576282723,108.3)) ;
#42990 = CARTESIAN_POINT('',(28.,-43.2232576282723,108.3)) ;
#42991 = CARTESIAN_POINT('',(28.4,-43.2232576282723,108.3)) ;
#42992 = CARTESIAN_POINT('Origin',(28.4,0.,108.3)) ;
#42993 = CARTESIAN_POINT('',(28.4,43.2232576282723,108.3)) ;
#42994 = CARTESIAN_POINT('Origin',(28.4,0.,108.3)) ;
#42995 = CARTESIAN_POINT('',(28.4,-42.9614943874163,108.3)) ;
#42996 = CARTESIAN_POINT('Origin',(28.4,0.,108.3)) ;
#42997 = CARTESIAN_POINT('',(28.4,-28.4,108.3)) ;
#42998 = CARTESIAN_POINT('',(28.4,-41.6,108.3)) ;
#42999 = CARTESIAN_POINT('Origin',(28.4,0.,108.3)) ;
#43000 = CARTESIAN_POINT('',(28.4,-14.4,108.3)) ;
#43001 = CARTESIAN_POINT('Origin',(28.4,0.,108.3)) ;
#43002 = CARTESIAN_POINT('',(28.4,-0.4,108.3)) ;
#43003 = CARTESIAN_POINT('Origin',(28.4,0.,108.3)) ;
#43004 = CARTESIAN_POINT('',(28.4,13.6,108.3)) ;
#43005 = CARTESIAN_POINT('Origin',(28.4,0.,108.3)) ;
#43006 = CARTESIAN_POINT('Origin',(27.6,0.,108.3)) ;
#43007 = CARTESIAN_POINT('',(27.6,-28.4,108.3)) ;
#43008 = CARTESIAN_POINT('',(27.6,-41.6,108.3)) ;
#43009 = CARTESIAN_POINT('Origin',(27.6,0.,108.3)) ;
#43010 = CARTESIAN_POINT('',(27.6,-14.4,108.3)) ;
#43011 = CARTESIAN_POINT('',(27.6,-27.6,108.3)) ;
#43012 = CARTESIAN_POINT('Origin',(27.6,0.,108.3)) ;
#43013 = CARTESIAN_POINT('',(27.6,-0.4,108.3)) ;
#43014 = CARTESIAN_POINT('',(27.6,-13.6,108.3)) ;
#43015 = CARTESIAN_POINT('Origin',(27.6,0.,108.3)) ;
#43016 = CARTESIAN_POINT('',(27.6,13.6,108.3)) ;
#43017 = CARTESIAN_POINT('',(27.6,0.4,108.3)) ;
#43018 = CARTESIAN_POINT('Origin',(27.6,0.,108.3)) ;
#43019 = CARTESIAN_POINT('',(27.6,27.6,108.3)) ;
#43020 = CARTESIAN_POINT('',(27.6,14.4,108.3)) ;
#43021 = CARTESIAN_POINT('Origin',(28.,43.2232576282723,108.3)) ;
#43022 = CARTESIAN_POINT('',(28.,43.2232576282723,108.3)) ;
#43023 = CARTESIAN_POINT('Origin',(28.4,0.,108.3)) ;
#43024 = CARTESIAN_POINT('',(28.4,27.6,108.3)) ;
#43025 = CARTESIAN_POINT('Origin',(0.,27.6,108.3)) ;
#43026 = CARTESIAN_POINT('Origin',(0.,28.4,108.3)) ;
#43027 = CARTESIAN_POINT('',(14.4,28.4,108.3)) ;
#43028 = CARTESIAN_POINT('Origin',(0.,0.,108.3)) ;
#43029 = CARTESIAN_POINT('',(14.4,49.4458289444115,108.3)) ;
#43030 = CARTESIAN_POINT('Origin',(0.,13.6,108.3)) ;
#43031 = CARTESIAN_POINT('Origin',(0.,14.4,108.3)) ;
#43032 = CARTESIAN_POINT('',(14.4,14.4,108.3)) ;
#43033 = CARTESIAN_POINT('Origin',(0.,-0.4,108.3)) ;
#43034 = CARTESIAN_POINT('Origin',(0.,0.4,108.3)) ;
#43035 = CARTESIAN_POINT('',(14.4,0.4,108.3)) ;
#43036 = CARTESIAN_POINT('Origin',(0.,-14.4,108.3)) ;
#43037 = CARTESIAN_POINT('Origin',(0.,-13.6,108.3)) ;
#43038 = CARTESIAN_POINT('',(14.4,-13.6,108.3)) ;
#43039 = CARTESIAN_POINT('Origin',(0.,-28.4,108.3)) ;
#43040 = CARTESIAN_POINT('Origin',(0.,-27.6,108.3)) ;
#43041 = CARTESIAN_POINT('',(14.4,-27.6,108.3)) ;
#43042 = CARTESIAN_POINT('Origin',(0.,0.,108.3)) ;
#43043 = CARTESIAN_POINT('',(29.2316609175736,-42.4,108.3)) ;
#43044 = CARTESIAN_POINT('Origin',(0.,-41.6,108.3)) ;
#43045 = CARTESIAN_POINT('',(14.4,-41.6,108.3)) ;
#43046 = CARTESIAN_POINT('Origin',(43.2232576282723,28.,108.3)) ;
#43047 = CARTESIAN_POINT('',(43.2232576282723,28.,108.3)) ;
#43048 = CARTESIAN_POINT('',(43.2232576282723,28.4,108.3)) ;
#43049 = CARTESIAN_POINT('Origin',(0.,28.4,108.3)) ;
#43050 = CARTESIAN_POINT('',(-42.9614943874163,28.4,108.3)) ;
#43051 = CARTESIAN_POINT('',(-43.2232576282723,28.4,108.3)) ;
#43052 = CARTESIAN_POINT('Origin',(0.,28.4,108.3)) ;
#43053 = CARTESIAN_POINT('',(-27.6,28.4,108.3)) ;
#43054 = CARTESIAN_POINT('Origin',(0.,28.4,108.3)) ;
#43055 = CARTESIAN_POINT('',(-13.6,28.4,108.3)) ;
#43056 = CARTESIAN_POINT('Origin',(0.,28.4,108.3)) ;
#43057 = CARTESIAN_POINT('',(-41.6,28.4,108.3)) ;
#43058 = CARTESIAN_POINT('Origin',(0.,28.4,108.3)) ;
#43059 = CARTESIAN_POINT('Origin',(0.,28.4,108.3)) ;
#43060 = CARTESIAN_POINT('',(0.4,28.4,108.3)) ;
#43061 = CARTESIAN_POINT('Origin',(0.,27.6,108.3)) ;
#43062 = CARTESIAN_POINT('',(-41.6,27.6,108.3)) ;
#43063 = CARTESIAN_POINT('',(-28.4,27.6,108.3)) ;
#43064 = CARTESIAN_POINT('Origin',(0.,27.6,108.3)) ;
#43065 = CARTESIAN_POINT('',(-14.4,27.6,108.3)) ;
#43066 = CARTESIAN_POINT('',(-27.6,27.6,108.3)) ;
#43067 = CARTESIAN_POINT('Origin',(0.,27.6,108.3)) ;
#43068 = CARTESIAN_POINT('',(14.4,27.6,108.3)) ;
#43069 = CARTESIAN_POINT('Origin',(0.,27.6,108.3)) ;
#43070 = CARTESIAN_POINT('',(-0.4,27.6,108.3)) ;
#43071 = CARTESIAN_POINT('',(-13.6,27.6,108.3)) ;
#43072 = CARTESIAN_POINT('Origin',(0.,27.6,108.3)) ;
#43073 = CARTESIAN_POINT('',(13.6,27.6,108.3)) ;
#43074 = CARTESIAN_POINT('',(0.4,27.6,108.3)) ;
#43075 = CARTESIAN_POINT('Origin',(-43.2232576282723,28.,108.3)) ;
#43076 = CARTESIAN_POINT('',(-43.2232576282723,28.,108.3)) ;
#43077 = CARTESIAN_POINT('Origin',(14.4,0.,108.3)) ;
#43078 = CARTESIAN_POINT('Origin',(13.6,0.,108.3)) ;
#43079 = CARTESIAN_POINT('',(13.6,48.6342471926933,108.3)) ;
#43080 = CARTESIAN_POINT('Origin',(13.6,0.,108.3)) ;
#43081 = CARTESIAN_POINT('',(13.6,14.4,108.3)) ;
#43082 = CARTESIAN_POINT('Origin',(0.4,0.,108.3)) ;
#43083 = CARTESIAN_POINT('Origin',(-0.4,0.,108.3)) ;
#43084 = CARTESIAN_POINT('',(-0.4,14.4,108.3)) ;
#43085 = CARTESIAN_POINT('Origin',(0.,0.,108.3)) ;
#43086 = CARTESIAN_POINT('Origin',(0.,0.,108.3)) ;
#43087 = CARTESIAN_POINT('',(49.4458289444115,14.4,108.3)) ;
#43088 = CARTESIAN_POINT('Origin',(-41.6,0.,108.3)) ;
#43089 = CARTESIAN_POINT('',(-41.6,28.6302287800849,108.3)) ;
#43090 = CARTESIAN_POINT('Origin',(0.,0.,108.3)) ;
#43091 = CARTESIAN_POINT('',(-42.4,29.2316609175736,108.3)) ;
#43092 = CARTESIAN_POINT('Origin',(0.,0.,108.3)) ;
#43093 = CARTESIAN_POINT('',(-49.4458289444115,14.4,108.3)) ;
#43094 = CARTESIAN_POINT('Origin',(-13.6,0.,108.3)) ;
#43095 = CARTESIAN_POINT('Origin',(-14.4,0.,108.3)) ;
#43096 = CARTESIAN_POINT('',(-14.4,14.4,108.3)) ;
#43097 = CARTESIAN_POINT('Origin',(-27.6,0.,108.3)) ;
#43098 = CARTESIAN_POINT('Origin',(-28.4,0.,108.3)) ;
#43099 = CARTESIAN_POINT('',(-28.4,14.4,108.3)) ;
#43100 = CARTESIAN_POINT('Origin',(14.,-49.5605690039975,108.3)) ;
#43101 = CARTESIAN_POINT('',(14.,-49.5605690039975,108.3)) ;
#43102 = CARTESIAN_POINT('',(14.4,-49.5605690039975,108.3)) ;
#43103 = CARTESIAN_POINT('Origin',(14.4,0.,108.3)) ;
#43104 = CARTESIAN_POINT('',(14.4,49.5605690039975,108.3)) ;
#43105 = CARTESIAN_POINT('Origin',(14.4,0.,108.3)) ;
#43106 = CARTESIAN_POINT('',(14.4,-48.4034089708566,108.3)) ;
#43107 = CARTESIAN_POINT('',(14.4,-42.4,108.3)) ;
#43108 = CARTESIAN_POINT('Origin',(14.4,0.,108.3)) ;
#43109 = CARTESIAN_POINT('',(14.4,-28.4,108.3)) ;
#43110 = CARTESIAN_POINT('Origin',(14.4,0.,108.3)) ;
#43111 = CARTESIAN_POINT('',(14.4,-14.4,108.3)) ;
#43112 = CARTESIAN_POINT('Origin',(14.4,0.,108.3)) ;
#43113 = CARTESIAN_POINT('',(14.4,-0.4,108.3)) ;
#43114 = CARTESIAN_POINT('Origin',(14.4,0.,108.3)) ;
#43115 = CARTESIAN_POINT('',(14.4,-49.4458289444115,108.3)) ;
#43116 = CARTESIAN_POINT('Origin',(14.4,0.,108.3)) ;
#43117 = CARTESIAN_POINT('Origin',(13.6,0.,108.3)) ;
#43118 = CARTESIAN_POINT('',(13.6,-28.4,108.3)) ;
#43119 = CARTESIAN_POINT('',(13.6,-41.6,108.3)) ;
#43120 = CARTESIAN_POINT('Origin',(13.6,0.,108.3)) ;
#43121 = CARTESIAN_POINT('',(13.6,-14.4,108.3)) ;
#43122 = CARTESIAN_POINT('',(13.6,-27.6,108.3)) ;
#43123 = CARTESIAN_POINT('Origin',(13.6,0.,108.3)) ;
#43124 = CARTESIAN_POINT('',(13.6,-0.4,108.3)) ;
#43125 = CARTESIAN_POINT('',(13.6,-13.6,108.3)) ;
#43126 = CARTESIAN_POINT('Origin',(13.6,0.,108.3)) ;
#43127 = CARTESIAN_POINT('',(13.6,13.6,108.3)) ;
#43128 = CARTESIAN_POINT('',(13.6,0.4,108.3)) ;
#43129 = CARTESIAN_POINT('Origin',(13.6,0.,108.3)) ;
#43130 = CARTESIAN_POINT('',(13.6,-48.6342471926933,108.3)) ;
#43131 = CARTESIAN_POINT('',(13.6,-42.4,108.3)) ;
#43132 = CARTESIAN_POINT('Origin',(14.,49.5605690039975,108.3)) ;
#43133 = CARTESIAN_POINT('',(14.,49.5605690039975,108.3)) ;
#43134 = CARTESIAN_POINT('Origin',(14.4,0.,108.3)) ;
#43135 = CARTESIAN_POINT('',(14.4,13.6,108.3)) ;
#43136 = CARTESIAN_POINT('Origin',(0.,13.6,108.3)) ;
#43137 = CARTESIAN_POINT('Origin',(0.,14.4,108.3)) ;
#43138 = CARTESIAN_POINT('Origin',(0.,14.4,108.3)) ;
#43139 = CARTESIAN_POINT('',(0.4,14.4,108.3)) ;
#43140 = CARTESIAN_POINT('Origin',(0.,0.,108.3)) ;
#43141 = CARTESIAN_POINT('',(0.4,51.4984465785134,108.3)) ;
#43142 = CARTESIAN_POINT('Origin',(0.,0.,108.3)) ;
#43143 = CARTESIAN_POINT('Origin',(0.,0.,108.3)) ;
#43144 = CARTESIAN_POINT('',(27.4315511774307,-42.4,108.3)) ;
#43145 = CARTESIAN_POINT('Origin',(0.,0.,108.3)) ;
#43146 = CARTESIAN_POINT('',(0.4,-50.4984158167363,108.3)) ;
#43147 = CARTESIAN_POINT('Origin',(0.,-0.4,108.3)) ;
#43148 = CARTESIAN_POINT('Origin',(0.,0.4,108.3)) ;
#43149 = CARTESIAN_POINT('',(0.4,0.4,108.3)) ;
#43150 = CARTESIAN_POINT('Origin',(0.,-14.4,108.3)) ;
#43151 = CARTESIAN_POINT('Origin',(0.,-13.6,108.3)) ;
#43152 = CARTESIAN_POINT('',(0.4,-13.6,108.3)) ;
#43153 = CARTESIAN_POINT('Origin',(0.,-28.4,108.3)) ;
#43154 = CARTESIAN_POINT('Origin',(0.,-27.6,108.3)) ;
#43155 = CARTESIAN_POINT('',(0.4,-27.6,108.3)) ;
#43156 = CARTESIAN_POINT('Origin',(0.,-42.4,108.3)) ;
#43157 = CARTESIAN_POINT('Origin',(0.,-41.6,108.3)) ;
#43158 = CARTESIAN_POINT('',(0.4,-41.6,108.3)) ;
#43159 = CARTESIAN_POINT('Origin',(49.5605690039975,14.,108.3)) ;
#43160 = CARTESIAN_POINT('',(49.5605690039975,14.,108.3)) ;
#43161 = CARTESIAN_POINT('',(49.5605690039975,14.4,108.3)) ;
#43162 = CARTESIAN_POINT('Origin',(0.,13.6,108.3)) ;
#43163 = CARTESIAN_POINT('',(-42.4,13.6,108.3)) ;
#43164 = CARTESIAN_POINT('',(-48.6342471926933,13.6,108.3)) ;
#43165 = CARTESIAN_POINT('Origin',(0.,13.6,108.3)) ;
#43166 = CARTESIAN_POINT('',(-28.4,13.6,108.3)) ;
#43167 = CARTESIAN_POINT('',(-41.6,13.6,108.3)) ;
#43168 = CARTESIAN_POINT('Origin',(0.,13.6,108.3)) ;
#43169 = CARTESIAN_POINT('',(-14.4,13.6,108.3)) ;
#43170 = CARTESIAN_POINT('',(-27.6,13.6,108.3)) ;
#43171 = CARTESIAN_POINT('Origin',(0.,13.6,108.3)) ;
#43172 = CARTESIAN_POINT('',(0.4,13.6,108.3)) ;
#43173 = CARTESIAN_POINT('Origin',(0.,13.6,108.3)) ;
#43174 = CARTESIAN_POINT('',(-0.4,13.6,108.3)) ;
#43175 = CARTESIAN_POINT('',(-13.6,13.6,108.3)) ;
#43176 = CARTESIAN_POINT('Origin',(0.,14.4,108.3)) ;
#43177 = CARTESIAN_POINT('',(-49.5605690039975,14.4,108.3)) ;
#43178 = CARTESIAN_POINT('Origin',(0.,14.4,108.3)) ;
#43179 = CARTESIAN_POINT('',(-42.4,14.4,108.3)) ;
#43180 = CARTESIAN_POINT('',(-48.4034089708566,14.4,108.3)) ;
#43181 = CARTESIAN_POINT('Origin',(0.,14.4,108.3)) ;
#43182 = CARTESIAN_POINT('',(-41.6,14.4,108.3)) ;
#43183 = CARTESIAN_POINT('Origin',(0.,14.4,108.3)) ;
#43184 = CARTESIAN_POINT('',(-27.6,14.4,108.3)) ;
#43185 = CARTESIAN_POINT('Origin',(0.,14.4,108.3)) ;
#43186 = CARTESIAN_POINT('',(-13.6,14.4,108.3)) ;
#43187 = CARTESIAN_POINT('Origin',(0.,14.4,108.3)) ;
#43188 = CARTESIAN_POINT('Origin',(-49.5605690039975,14.,108.3)) ;
#43189 = CARTESIAN_POINT('',(-49.5605690039975,14.,108.3)) ;
#43190 = CARTESIAN_POINT('Origin',(0.4,0.,108.3)) ;
#43191 = CARTESIAN_POINT('Origin',(-0.4,0.,108.3)) ;
#43192 = CARTESIAN_POINT('',(-0.4,50.4984158167363,108.3)) ;
#43193 = CARTESIAN_POINT('Origin',(-0.4,0.,108.3)) ;
#43194 = CARTESIAN_POINT('',(-0.4,0.4,108.3)) ;
#43195 = CARTESIAN_POINT('Origin',(0.,0.,108.3)) ;
#43196 = CARTESIAN_POINT('Origin',(0.,0.,108.3)) ;
#43197 = CARTESIAN_POINT('',(50.4984158167363,0.4,108.3)) ;
#43198 = CARTESIAN_POINT('Origin',(0.,0.,108.3)) ;
#43199 = CARTESIAN_POINT('',(51.4984465785134,0.4,108.3)) ;
#43200 = CARTESIAN_POINT('Origin',(-13.6,0.,108.3)) ;
#43201 = CARTESIAN_POINT('Origin',(-14.4,0.,108.3)) ;
#43202 = CARTESIAN_POINT('',(-14.4,0.4,108.3)) ;
#43203 = CARTESIAN_POINT('Origin',(-27.6,0.,108.3)) ;
#43204 = CARTESIAN_POINT('Origin',(-28.4,0.,108.3)) ;
#43205 = CARTESIAN_POINT('',(-28.4,0.4,108.3)) ;
#43206 = CARTESIAN_POINT('Origin',(-41.6,0.,108.3)) ;
#43207 = CARTESIAN_POINT('Origin',(-42.4,0.,108.3)) ;
#43208 = CARTESIAN_POINT('',(-42.4,0.4,108.3)) ;
#43209 = CARTESIAN_POINT('Origin',(0.,0.,108.3)) ;
#43210 = CARTESIAN_POINT('',(-42.4,27.4315511774307,108.3)) ;
#43211 = CARTESIAN_POINT('Origin',(0.,0.,108.3)) ;
#43212 = CARTESIAN_POINT('',(-51.4984465785134,0.4,108.3)) ;
#43213 = CARTESIAN_POINT('Origin',(0.4,0.,108.3)) ;
#43214 = CARTESIAN_POINT('',(0.4,51.5,108.3)) ;
#43215 = CARTESIAN_POINT('Origin',(0.4,0.,108.3)) ;
#43216 = CARTESIAN_POINT('',(0.4,-42.4,108.3)) ;
#43217 = CARTESIAN_POINT('Origin',(0.4,0.,108.3)) ;
#43218 = CARTESIAN_POINT('',(0.4,-28.4,108.3)) ;
#43219 = CARTESIAN_POINT('Origin',(0.4,0.,108.3)) ;
#43220 = CARTESIAN_POINT('',(0.4,-51.4984465785134,108.3)) ;
#43221 = CARTESIAN_POINT('',(0.4,-51.5,108.3)) ;
#43222 = CARTESIAN_POINT('Origin',(0.4,0.,108.3)) ;
#43223 = CARTESIAN_POINT('',(0.4,-14.4,108.3)) ;
#43224 = CARTESIAN_POINT('Origin',(0.4,0.,108.3)) ;
#43225 = CARTESIAN_POINT('Origin',(0.4,0.,108.3)) ;
#43226 = CARTESIAN_POINT('',(0.4,-0.4,108.3)) ;
#43227 = CARTESIAN_POINT('Origin',(-0.4,0.,108.3)) ;
#43228 = CARTESIAN_POINT('',(-0.4,-51.4984465785134,108.3)) ;
#43229 = CARTESIAN_POINT('',(-0.4,-51.5,108.3)) ;
#43230 = CARTESIAN_POINT('Origin',(-0.4,0.,108.3)) ;
#43231 = CARTESIAN_POINT('',(-0.4,-28.4,108.3)) ;
#43232 = CARTESIAN_POINT('',(-0.4,-41.6,108.3)) ;
#43233 = CARTESIAN_POINT('Origin',(-0.4,0.,108.3)) ;
#43234 = CARTESIAN_POINT('',(-0.4,-14.4,108.3)) ;
#43235 = CARTESIAN_POINT('',(-0.4,-27.6,108.3)) ;
#43236 = CARTESIAN_POINT('Origin',(-0.4,0.,108.3)) ;
#43237 = CARTESIAN_POINT('',(-0.4,-50.4984158167363,108.3)) ;
#43238 = CARTESIAN_POINT('',(-0.4,-42.4,108.3)) ;
#43239 = CARTESIAN_POINT('Origin',(-0.4,0.,108.3)) ;
#43240 = CARTESIAN_POINT('',(-0.4,-0.4,108.3)) ;
#43241 = CARTESIAN_POINT('',(-0.4,-13.6,108.3)) ;
#43242 = CARTESIAN_POINT('Origin',(-0.4,0.,108.3)) ;
#43243 = CARTESIAN_POINT('',(-0.4,51.4984465785134,108.3)) ;
#43244 = CARTESIAN_POINT('',(-0.4,51.5,108.3)) ;
#43245 = CARTESIAN_POINT('Origin',(0.,-51.5,108.3)) ;
#43246 = CARTESIAN_POINT('Origin',(0.,51.5,108.3)) ;
#43247 = CARTESIAN_POINT('Origin',(0.,0.4,108.3)) ;
#43248 = CARTESIAN_POINT('',(-13.6,0.4,108.3)) ;
#43249 = CARTESIAN_POINT('Origin',(0.,-0.4,108.3)) ;
#43250 = CARTESIAN_POINT('',(-13.6,-0.4,108.3)) ;
#43251 = CARTESIAN_POINT('Origin',(0.,-0.4,108.3)) ;
#43252 = CARTESIAN_POINT('Origin',(0.,0.,108.3)) ;
#43253 = CARTESIAN_POINT('Origin',(0.,0.,108.3)) ;
#43254 = CARTESIAN_POINT('',(-14.,49.5605690039975,108.3)) ;
#43255 = CARTESIAN_POINT('Origin',(0.,-14.4,108.3)) ;
#43256 = CARTESIAN_POINT('Origin',(0.,-13.6,108.3)) ;
#43257 = CARTESIAN_POINT('',(-13.6,-13.6,108.3)) ;
#43258 = CARTESIAN_POINT('Origin',(0.,0.,108.3)) ;
#43259 = CARTESIAN_POINT('Origin',(0.,0.,108.3)) ;
#43260 = CARTESIAN_POINT('',(-14.,-49.5605690039975,108.3)) ;
#43261 = CARTESIAN_POINT('Origin',(0.,0.,108.3)) ;
#43262 = CARTESIAN_POINT('',(-13.6,-48.6342471926933,108.3)) ;
#43263 = CARTESIAN_POINT('Origin',(0.,-28.4,108.3)) ;
#43264 = CARTESIAN_POINT('Origin',(0.,-27.6,108.3)) ;
#43265 = CARTESIAN_POINT('',(-13.6,-27.6,108.3)) ;
#43266 = CARTESIAN_POINT('Origin',(0.,-42.4,108.3)) ;
#43267 = CARTESIAN_POINT('Origin',(0.,-41.6,108.3)) ;
#43268 = CARTESIAN_POINT('',(-13.6,-41.6,108.3)) ;
#43269 = CARTESIAN_POINT('Origin',(0.,0.4,108.3)) ;
#43270 = CARTESIAN_POINT('',(-51.5,0.4,108.3)) ;
#43271 = CARTESIAN_POINT('Origin',(0.,0.4,108.3)) ;
#43272 = CARTESIAN_POINT('',(-50.4984158167363,0.4,108.3)) ;
#43273 = CARTESIAN_POINT('Origin',(0.,0.4,108.3)) ;
#43274 = CARTESIAN_POINT('',(-41.6,0.4,108.3)) ;
#43275 = CARTESIAN_POINT('Origin',(0.,0.4,108.3)) ;
#43276 = CARTESIAN_POINT('',(51.5,0.4,108.3)) ;
#43277 = CARTESIAN_POINT('Origin',(0.,0.4,108.3)) ;
#43278 = CARTESIAN_POINT('',(-27.6,0.4,108.3)) ;
#43279 = CARTESIAN_POINT('Origin',(0.,0.4,108.3)) ;
#43280 = CARTESIAN_POINT('Origin',(0.,-0.4,108.3)) ;
#43281 = CARTESIAN_POINT('',(51.4984465785134,-0.4,108.3)) ;
#43282 = CARTESIAN_POINT('',(51.5,-0.4,108.3)) ;
#43283 = CARTESIAN_POINT('Origin',(0.,-0.4,108.3)) ;
#43284 = CARTESIAN_POINT('',(-51.4984465785134,-0.4,108.3)) ;
#43285 = CARTESIAN_POINT('',(-51.5,-0.4,108.3)) ;
#43286 = CARTESIAN_POINT('Origin',(0.,-0.4,108.3)) ;
#43287 = CARTESIAN_POINT('',(-42.4,-0.4,108.3)) ;
#43288 = CARTESIAN_POINT('',(-50.4984158167363,-0.4,108.3)) ;
#43289 = CARTESIAN_POINT('Origin',(0.,-0.4,108.3)) ;
#43290 = CARTESIAN_POINT('',(-28.4,-0.4,108.3)) ;
#43291 = CARTESIAN_POINT('',(-41.6,-0.4,108.3)) ;
#43292 = CARTESIAN_POINT('Origin',(0.,-0.4,108.3)) ;
#43293 = CARTESIAN_POINT('',(-14.4,-0.4,108.3)) ;
#43294 = CARTESIAN_POINT('',(-27.6,-0.4,108.3)) ;
#43295 = CARTESIAN_POINT('Origin',(-51.5,0.,108.3)) ;
#43296 = CARTESIAN_POINT('Origin',(51.5,0.,108.3)) ;
#43297 = CARTESIAN_POINT('Origin',(-14.4,0.,108.3)) ;
#43298 = CARTESIAN_POINT('',(-14.4,-13.6,108.3)) ;
#43299 = CARTESIAN_POINT('Origin',(-13.6,0.,108.3)) ;
#43300 = CARTESIAN_POINT('Origin',(-13.6,0.,108.3)) ;
#43301 = CARTESIAN_POINT('Origin',(-27.6,0.,108.3)) ;
#43302 = CARTESIAN_POINT('Origin',(-28.4,0.,108.3)) ;
#43303 = CARTESIAN_POINT('',(-28.4,-13.6,108.3)) ;
#43304 = CARTESIAN_POINT('Origin',(0.,0.,108.3)) ;
#43305 = CARTESIAN_POINT('',(48.6342471926933,-13.6,108.3)) ;
#43306 = CARTESIAN_POINT('Origin',(-41.6,0.,108.3)) ;
#43307 = CARTESIAN_POINT('Origin',(-42.4,0.,108.3)) ;
#43308 = CARTESIAN_POINT('',(-42.4,-13.6,108.3)) ;
#43309 = CARTESIAN_POINT('Origin',(0.,0.,108.3)) ;
#43310 = CARTESIAN_POINT('',(-48.6342471926933,-13.6,108.3)) ;
#43311 = CARTESIAN_POINT('Origin',(0.,0.,108.3)) ;
#43312 = CARTESIAN_POINT('Origin',(0.,0.,108.3)) ;
#43313 = CARTESIAN_POINT('',(-49.5605690039975,-14.,108.3)) ;
#43314 = CARTESIAN_POINT('Origin',(-14.,49.5605690039975,108.3)) ;
#43315 = CARTESIAN_POINT('',(-14.4,49.5605690039975,108.3)) ;
#43316 = CARTESIAN_POINT('Origin',(-14.4,0.,108.3)) ;
#43317 = CARTESIAN_POINT('',(-14.4,-49.4458289444115,108.3)) ;
#43318 = CARTESIAN_POINT('',(-14.4,-49.5605690039975,108.3)) ;
#43319 = CARTESIAN_POINT('Origin',(-14.4,0.,108.3)) ;
#43320 = CARTESIAN_POINT('',(-14.4,-42.4,108.3)) ;
#43321 = CARTESIAN_POINT('',(-14.4,-48.4034089708566,108.3)) ;
#43322 = CARTESIAN_POINT('Origin',(-14.4,0.,108.3)) ;
#43323 = CARTESIAN_POINT('',(-14.4,-28.4,108.3)) ;
#43324 = CARTESIAN_POINT('',(-14.4,-41.6,108.3)) ;
#43325 = CARTESIAN_POINT('Origin',(-14.4,0.,108.3)) ;
#43326 = CARTESIAN_POINT('',(-14.4,49.4458289444115,108.3)) ;
#43327 = CARTESIAN_POINT('Origin',(-14.4,0.,108.3)) ;
#43328 = CARTESIAN_POINT('',(-14.4,-14.4,108.3)) ;
#43329 = CARTESIAN_POINT('',(-14.4,-27.6,108.3)) ;
#43330 = CARTESIAN_POINT('Origin',(-14.4,0.,108.3)) ;
#43331 = CARTESIAN_POINT('Origin',(-13.6,0.,108.3)) ;
#43332 = CARTESIAN_POINT('',(-13.6,-42.4,108.3)) ;
#43333 = CARTESIAN_POINT('Origin',(-13.6,0.,108.3)) ;
#43334 = CARTESIAN_POINT('',(-13.6,-28.4,108.3)) ;
#43335 = CARTESIAN_POINT('Origin',(-14.,-49.5605690039975,108.3)) ;
#43336 = CARTESIAN_POINT('Origin',(-13.6,0.,108.3)) ;
#43337 = CARTESIAN_POINT('',(-13.6,-14.4,108.3)) ;
#43338 = CARTESIAN_POINT('Origin',(0.,-14.4,108.3)) ;
#43339 = CARTESIAN_POINT('Origin',(0.,-13.6,108.3)) ;
#43340 = CARTESIAN_POINT('Origin',(0.,-13.6,108.3)) ;
#43341 = CARTESIAN_POINT('',(-27.6,-13.6,108.3)) ;
#43342 = CARTESIAN_POINT('Origin',(0.,-28.4,108.3)) ;
#43343 = CARTESIAN_POINT('Origin',(0.,-27.6,108.3)) ;
#43344 = CARTESIAN_POINT('',(-27.6,-27.6,108.3)) ;
#43345 = CARTESIAN_POINT('Origin',(0.,0.,108.3)) ;
#43346 = CARTESIAN_POINT('',(-28.,43.2232576282723,108.3)) ;
#43347 = CARTESIAN_POINT('Origin',(0.,-41.6,108.3)) ;
#43348 = CARTESIAN_POINT('',(-27.6,-41.6,108.3)) ;
#43349 = CARTESIAN_POINT('Origin',(0.,-42.4,108.3)) ;
#43350 = CARTESIAN_POINT('Origin',(0.,0.,108.3)) ;
#43351 = CARTESIAN_POINT('',(-28.,-43.2232576282723,108.3)) ;
#43352 = CARTESIAN_POINT('Origin',(0.,0.,108.3)) ;
#43353 = CARTESIAN_POINT('',(-27.4315511774307,-42.4,108.3)) ;
#43354 = CARTESIAN_POINT('Origin',(-49.5605690039975,-14.,108.3)) ;
#43355 = CARTESIAN_POINT('',(-49.5605690039975,-14.4,108.3)) ;
#43356 = CARTESIAN_POINT('Origin',(0.,-13.6,108.3)) ;
#43357 = CARTESIAN_POINT('Origin',(0.,-13.6,108.3)) ;
#43358 = CARTESIAN_POINT('',(-41.6,-13.6,108.3)) ;
#43359 = CARTESIAN_POINT('Origin',(0.,-14.4,108.3)) ;
#43360 = CARTESIAN_POINT('',(-49.4458289444115,-14.4,108.3)) ;
#43361 = CARTESIAN_POINT('Origin',(0.,-14.4,108.3)) ;
#43362 = CARTESIAN_POINT('',(-42.4,-14.4,108.3)) ;
#43363 = CARTESIAN_POINT('',(-48.4034089708566,-14.4,108.3)) ;
#43364 = CARTESIAN_POINT('Origin',(0.,-14.4,108.3)) ;
#43365 = CARTESIAN_POINT('',(49.4458289444115,-14.4,108.3)) ;
#43366 = CARTESIAN_POINT('',(49.5605690039975,-14.4,108.3)) ;
#43367 = CARTESIAN_POINT('Origin',(0.,-14.4,108.3)) ;
#43368 = CARTESIAN_POINT('',(-28.4,-14.4,108.3)) ;
#43369 = CARTESIAN_POINT('',(-41.6,-14.4,108.3)) ;
#43370 = CARTESIAN_POINT('Origin',(0.,-14.4,108.3)) ;
#43371 = CARTESIAN_POINT('',(-27.6,-14.4,108.3)) ;
#43372 = CARTESIAN_POINT('Origin',(49.5605690039975,-14.,108.3)) ;
#43373 = CARTESIAN_POINT('',(49.5605690039975,-14.,108.3)) ;
#43374 = CARTESIAN_POINT('Origin',(-27.6,0.,108.3)) ;
#43375 = CARTESIAN_POINT('Origin',(-28.4,0.,108.3)) ;
#43376 = CARTESIAN_POINT('',(-28.4,-27.6,108.3)) ;
#43377 = CARTESIAN_POINT('Origin',(0.,0.,108.3)) ;
#43378 = CARTESIAN_POINT('Origin',(0.,0.,108.3)) ;
#43379 = CARTESIAN_POINT('',(43.2232576282723,-28.,108.3)) ;
#43380 = CARTESIAN_POINT('Origin',(0.,0.,108.3)) ;
#43381 = CARTESIAN_POINT('Origin',(-41.6,0.,108.3)) ;
#43382 = CARTESIAN_POINT('Origin',(-42.4,0.,108.3)) ;
#43383 = CARTESIAN_POINT('',(-42.4,-27.4315511774307,108.3)) ;
#43384 = CARTESIAN_POINT('Origin',(0.,0.,108.3)) ;
#43385 = CARTESIAN_POINT('',(-43.2232576282723,-28.,108.3)) ;
#43386 = CARTESIAN_POINT('Origin',(0.,0.,108.3)) ;
#43387 = CARTESIAN_POINT('Origin',(-28.,43.2232576282723,108.3)) ;
#43388 = CARTESIAN_POINT('',(-28.4,43.2232576282723,108.3)) ;
#43389 = CARTESIAN_POINT('Origin',(-27.6,0.,108.3)) ;
#43390 = CARTESIAN_POINT('Origin',(-28.4,0.,108.3)) ;
#43391 = CARTESIAN_POINT('',(-28.4,-42.9614943874163,108.3)) ;
#43392 = CARTESIAN_POINT('',(-28.4,-43.2232576282723,108.3)) ;
#43393 = CARTESIAN_POINT('Origin',(-28.4,0.,108.3)) ;
#43394 = CARTESIAN_POINT('Origin',(-28.4,0.,108.3)) ;
#43395 = CARTESIAN_POINT('',(-28.4,-28.4,108.3)) ;
#43396 = CARTESIAN_POINT('',(-28.4,-41.6,108.3)) ;
#43397 = CARTESIAN_POINT('Origin',(-28.,-43.2232576282723,108.3)) ;
#43398 = CARTESIAN_POINT('Origin',(-27.6,0.,108.3)) ;
#43399 = CARTESIAN_POINT('',(-27.6,-28.4,108.3)) ;
#43400 = CARTESIAN_POINT('Origin',(0.,-28.4,108.3)) ;
#43401 = CARTESIAN_POINT('Origin',(0.,-27.6,108.3)) ;
#43402 = CARTESIAN_POINT('',(-41.6,-27.6,108.3)) ;
#43403 = CARTESIAN_POINT('Origin',(0.,0.,108.3)) ;
#43404 = CARTESIAN_POINT('Origin',(0.,-41.6,108.3)) ;
#43405 = CARTESIAN_POINT('',(-28.6302287800849,-41.6,108.3)) ;
#43406 = CARTESIAN_POINT('Origin',(0.,0.,108.3)) ;
#43407 = CARTESIAN_POINT('',(-29.2316609175736,-42.4,108.3)) ;
#43408 = CARTESIAN_POINT('Origin',(-43.2232576282723,-28.,108.3)) ;
#43409 = CARTESIAN_POINT('',(-43.2232576282723,-28.4,108.3)) ;
#43410 = CARTESIAN_POINT('Origin',(0.,-28.4,108.3)) ;
#43411 = CARTESIAN_POINT('',(43.2232576282723,-28.4,108.3)) ;
#43412 = CARTESIAN_POINT('Origin',(0.,-28.4,108.3)) ;
#43413 = CARTESIAN_POINT('',(-42.9614943874163,-28.4,108.3)) ;
#43414 = CARTESIAN_POINT('Origin',(0.,-28.4,108.3)) ;
#43415 = CARTESIAN_POINT('',(-41.6,-28.4,108.3)) ;
#43416 = CARTESIAN_POINT('Origin',(43.2232576282723,-28.,108.3)) ;
#43417 = CARTESIAN_POINT('Origin',(-41.6,0.,108.3)) ;
#43418 = CARTESIAN_POINT('',(-41.6,-28.6302287800849,108.3)) ;
#43419 = CARTESIAN_POINT('Origin',(-41.6,0.,108.3)) ;
#43420 = CARTESIAN_POINT('Origin',(0.,0.,108.3)) ;
#43421 = CARTESIAN_POINT('',(-42.4,-29.2316609175736,108.3)) ;
#43422 = CARTESIAN_POINT('Origin',(-42.,29.8035232816525,108.3)) ;
#43423 = CARTESIAN_POINT('',(-42.4,29.8035232816525,108.3)) ;
#43424 = CARTESIAN_POINT('Origin',(-42.4,0.,108.3)) ;
#43425 = CARTESIAN_POINT('Origin',(-42.4,0.,108.3)) ;
#43426 = CARTESIAN_POINT('Origin',(-42.4,0.,108.3)) ;
#43427 = CARTESIAN_POINT('',(-42.4,-29.8035232816525,108.3)) ;
#43428 = CARTESIAN_POINT('Origin',(-42.,-29.8035232816525,108.3)) ;
#43429 = CARTESIAN_POINT('',(-42.,-29.8035232816525,108.3)) ;
#43430 = CARTESIAN_POINT('Origin',(0.,0.,108.3)) ;
#43431 = CARTESIAN_POINT('',(-29.8035232816525,-42.,108.3)) ;
#43432 = CARTESIAN_POINT('Origin',(0.,0.,108.3)) ;
#43433 = CARTESIAN_POINT('Origin',(0.,-41.6,108.3)) ;
#43434 = CARTESIAN_POINT('Origin',(-29.8035232816525,-42.,108.3)) ;
#43435 = CARTESIAN_POINT('',(-29.8035232816525,-42.4,108.3)) ;
#43436 = CARTESIAN_POINT('Origin',(0.,-42.4,108.3)) ;
#43437 = CARTESIAN_POINT('',(29.8035232816525,-42.4,108.3)) ;
#43438 = CARTESIAN_POINT('Origin',(0.,-42.4,108.3)) ;
#43439 = CARTESIAN_POINT('Origin',(0.,-42.4,108.3)) ;
#43440 = CARTESIAN_POINT('Origin',(29.8035232816525,-42.,108.3)) ;
#43441 = CARTESIAN_POINT('',(0.,0.,0.)) ;
#43442 = CARTESIAN_POINT('Origin',(31.,0.,70.)) ;
#43443 = CARTESIAN_POINT('',(30.9999999999999,-2.15655990727168E-15,72.)) ;
#43444 = CARTESIAN_POINT('',(30.9999999999999,-2.15655990727168E-15,68.)) ;
#43445 = CARTESIAN_POINT('Origin',(31.,-7.99360577730113E-15,70.)) ;
#43446 = CARTESIAN_POINT('Origin',(31.,0.,70.)) ;
#43447 = CARTESIAN_POINT('Origin',(30.2227652776365,-6.89814895264575,70.)) ;
#43448 = CARTESIAN_POINT('',(30.2227652776365,-6.89814895264575,68.)) ;
#43449 = CARTESIAN_POINT('',(30.2227652776365,-6.89814895264575,72.)) ;
#43450 = CARTESIAN_POINT('Origin',(30.2227652776365,-6.89814895264575,70.)) ;
#43451 = CARTESIAN_POINT('Origin',(30.2227652776365,-6.89814895264576,70.)) ;
#43452 = CARTESIAN_POINT('Origin',(27.930034904975,-13.4503959126443,70.)) ;
#43453 = CARTESIAN_POINT('',(27.930034904975,-13.4503959126443,68.)) ;
#43454 = CARTESIAN_POINT('',(27.930034904975,-13.4503959126443,72.)) ;
#43455 = CARTESIAN_POINT('Origin',(27.930034904975,-13.4503959126443,70.)) ;
#43456 = CARTESIAN_POINT('Origin',(27.930034904975,-13.4503959126443,70.)) ;
#43457 = CARTESIAN_POINT('Origin',(24.2367759565089,-19.3281838576207,70.)) ;
#43458 = CARTESIAN_POINT('',(24.2367759565089,-19.3281838576207,68.)) ;
#43459 = CARTESIAN_POINT('',(24.2367759565089,-19.3281838576207,72.)) ;
#43460 = CARTESIAN_POINT('Origin',(24.2367759565089,-19.3281838576207,70.)) ;
#43461 = CARTESIAN_POINT('Origin',(24.2367759565089,-19.3281838576208,70.)) ;
#43462 = CARTESIAN_POINT('Origin',(19.3281838576207,-24.2367759565089,70.)) ;
#43463 = CARTESIAN_POINT('',(19.3281838576208,-24.236775956509,68.)) ;
#43464 = CARTESIAN_POINT('',(19.3281838576208,-24.236775956509,72.)) ;
#43465 = CARTESIAN_POINT('Origin',(19.3281838576207,-24.2367759565089,70.)) ;
#43466 = CARTESIAN_POINT('Origin',(19.3281838576207,-24.2367759565089,70.)) ;
#43467 = CARTESIAN_POINT('Origin',(13.4503959126443,-27.930034904975,70.)) ;
#43468 = CARTESIAN_POINT('',(13.4503959126442,-27.9300349049749,68.)) ;
#43469 = CARTESIAN_POINT('',(13.4503959126442,-27.9300349049749,72.)) ;
#43470 = CARTESIAN_POINT('Origin',(13.4503959126443,-27.930034904975,70.)) ;
#43471 = CARTESIAN_POINT('Origin',(13.4503959126443,-27.930034904975,70.)) ;
#43472 = CARTESIAN_POINT('Origin',(6.89814895264571,-30.2227652776365,70.)) ;
#43473 = CARTESIAN_POINT('',(6.89814895264574,-30.2227652776366,68.)) ;
#43474 = CARTESIAN_POINT('',(6.89814895264574,-30.2227652776366,72.)) ;
#43475 = CARTESIAN_POINT('Origin',(6.89814895264571,-30.2227652776365,70.)) ;
#43476 = CARTESIAN_POINT('Origin',(6.89814895264571,-30.2227652776365,70.)) ;
#43477 = CARTESIAN_POINT('Origin',(-5.69460761603519E-15,-31.,70.)) ;
#43478 = CARTESIAN_POINT('',(-9.22043443155371E-15,-31.,68.)) ;
#43479 = CARTESIAN_POINT('',(-9.22043443155371E-15,-31.,72.)) ;
#43480 = CARTESIAN_POINT('Origin',(-5.32907051820075E-15,-31.,70.)) ;
#43481 = CARTESIAN_POINT('',(-0.223928952206608,-32.9874244197865,70.)) ;
#43482 = CARTESIAN_POINT('Origin',(-5.32907051820075E-15,-31.,70.)) ;
#43483 = CARTESIAN_POINT('Origin',(-5.32907051820075E-15,-31.,70.)) ;
#43484 = CARTESIAN_POINT('Origin',(-6.89814895264575,-30.2227652776365,70.)) ;
#43485 = CARTESIAN_POINT('',(-6.89814895264576,-30.2227652776366,68.)) ;
#43486 = CARTESIAN_POINT('',(-7.12207790485237,-32.210189697423,70.)) ;
#43487 = CARTESIAN_POINT('Origin',(-6.89814895264575,-30.2227652776365,70.)) ;
#43488 = CARTESIAN_POINT('',(-6.89814895264576,-30.2227652776366,72.)) ;
#43489 = CARTESIAN_POINT('Origin',(-6.89814895264575,-30.2227652776365,70.)) ;
#43490 = CARTESIAN_POINT('',(-7.55870707655606,-32.1105319382533,70.)) ;
#43491 = CARTESIAN_POINT('Origin',(-6.89814895264575,-30.2227652776365,70.)) ;
#43492 = CARTESIAN_POINT('Origin',(-6.89814895264575,-30.2227652776365,70.)) ;
#43493 = CARTESIAN_POINT('Origin',(-13.4503959126443,-27.930034904975,70.)) ;
#43494 = CARTESIAN_POINT('',(-13.4503959126443,-27.930034904975,68.)) ;
#43495 = CARTESIAN_POINT('',(-14.1109540365546,-29.8178015655917,70.)) ;
#43496 = CARTESIAN_POINT('Origin',(-13.4503959126443,-27.930034904975,70.)) ;
#43497 = CARTESIAN_POINT('',(-13.4503959126443,-27.930034904975,72.)) ;
#43498 = CARTESIAN_POINT('Origin',(-13.4503959126443,-27.930034904975,70.)) ;
#43499 = CARTESIAN_POINT('',(-14.514460065675,-29.6234833034316,70.)) ;
#43500 = CARTESIAN_POINT('Origin',(-13.4503959126443,-27.930034904975,70.)) ;
#43501 = CARTESIAN_POINT('Origin',(-13.4503959126443,-27.930034904975,70.)) ;
#43502 = CARTESIAN_POINT('Origin',(-19.3281838576207,-24.2367759565089,70.)) ;
#43503 = CARTESIAN_POINT('',(-19.3281838576207,-24.2367759565089,68.)) ;
#43504 = CARTESIAN_POINT('',(-20.3922480106514,-25.9302243549655,70.)) ;
#43505 = CARTESIAN_POINT('Origin',(-19.3281838576207,-24.2367759565089,70.)) ;
#43506 = CARTESIAN_POINT('',(-19.3281838576207,-24.2367759565089,72.)) ;
#43507 = CARTESIAN_POINT('Origin',(-19.3281838576207,-24.2367759565089,70.)) ;
#43508 = CARTESIAN_POINT('',(-20.7423974199938,-25.650989518882,70.)) ;
#43509 = CARTESIAN_POINT('Origin',(-19.3281838576207,-24.2367759565089,70.)) ;
#43510 = CARTESIAN_POINT('Origin',(-19.3281838576207,-24.2367759565089,70.)) ;
#43511 = CARTESIAN_POINT('Origin',(-24.2367759565089,-19.3281838576208,70.)) ;
#43512 = CARTESIAN_POINT('',(-24.236775956509,-19.3281838576208,68.)) ;
#43513 = CARTESIAN_POINT('',(-25.650989518882,-20.7423974199938,70.)) ;
#43514 = CARTESIAN_POINT('Origin',(-24.2367759565089,-19.3281838576208,70.)) ;
#43515 = CARTESIAN_POINT('',(-24.236775956509,-19.3281838576208,72.)) ;
#43516 = CARTESIAN_POINT('Origin',(-24.2367759565089,-19.3281838576208,70.)) ;
#43517 = CARTESIAN_POINT('',(-25.9302243549655,-20.3922480106514,70.)) ;
#43518 = CARTESIAN_POINT('Origin',(-24.2367759565089,-19.3281838576208,70.)) ;
#43519 = CARTESIAN_POINT('Origin',(-24.2367759565089,-19.3281838576208,70.)) ;
#43520 = CARTESIAN_POINT('Origin',(-27.930034904975,-13.4503959126443,70.)) ;
#43521 = CARTESIAN_POINT('',(-27.930034904975,-13.4503959126443,68.)) ;
#43522 = CARTESIAN_POINT('',(-29.6234833034316,-14.514460065675,70.)) ;
#43523 = CARTESIAN_POINT('Origin',(-27.930034904975,-13.4503959126443,70.)) ;
#43524 = CARTESIAN_POINT('',(-27.930034904975,-13.4503959126443,72.)) ;
#43525 = CARTESIAN_POINT('Origin',(-27.930034904975,-13.4503959126443,70.)) ;
#43526 = CARTESIAN_POINT('',(-29.8178015655917,-14.1109540365547,70.)) ;
#43527 = CARTESIAN_POINT('Origin',(-27.930034904975,-13.4503959126443,70.)) ;
#43528 = CARTESIAN_POINT('Origin',(-27.930034904975,-13.4503959126443,70.)) ;
#43529 = CARTESIAN_POINT('Origin',(-30.2227652776365,-6.89814895264573,70.)) ;
#43530 = CARTESIAN_POINT('',(-30.2227652776365,-6.89814895264572,68.)) ;
#43531 = CARTESIAN_POINT('',(-32.1105319382533,-7.55870707655606,70.)) ;
#43532 = CARTESIAN_POINT('Origin',(-30.2227652776365,-6.89814895264573,70.)) ;
#43533 = CARTESIAN_POINT('',(-30.2227652776365,-6.89814895264572,72.)) ;
#43534 = CARTESIAN_POINT('Origin',(-30.2227652776365,-6.89814895264573,70.)) ;
#43535 = CARTESIAN_POINT('',(-32.210189697423,-7.12207790485236,70.)) ;
#43536 = CARTESIAN_POINT('Origin',(-30.2227652776365,-6.89814895264573,70.)) ;
#43537 = CARTESIAN_POINT('Origin',(-30.2227652776365,-6.89814895264573,70.)) ;
#43538 = CARTESIAN_POINT('Origin',(-31.,3.7964050773568E-15,70.)) ;
#43539 = CARTESIAN_POINT('',(-31.,7.44407759215346E-15,68.)) ;
#43540 = CARTESIAN_POINT('',(-32.9874244197865,-0.223928952206611,70.)) ;
#43541 = CARTESIAN_POINT('Origin',(-31.,3.5527136788005E-15,70.)) ;
#43542 = CARTESIAN_POINT('',(-31.,7.44407759215346E-15,72.)) ;
#43543 = CARTESIAN_POINT('Origin',(-31.,3.5527136788005E-15,70.)) ;
#43544 = CARTESIAN_POINT('',(-32.9874244197865,0.2239289522066,70.)) ;
#43545 = CARTESIAN_POINT('Origin',(-31.,3.5527136788005E-15,70.)) ;
#43546 = CARTESIAN_POINT('Origin',(-31.,3.5527136788005E-15,70.)) ;
#43547 = CARTESIAN_POINT('Origin',(-30.2227652776365,6.89814895264574,70.)) ;
#43548 = CARTESIAN_POINT('',(-30.2227652776366,6.89814895264574,68.)) ;
#43549 = CARTESIAN_POINT('',(-32.210189697423,7.12207790485236,70.)) ;
#43550 = CARTESIAN_POINT('Origin',(-30.2227652776365,6.89814895264574,70.)) ;
#43551 = CARTESIAN_POINT('',(-30.2227652776366,6.89814895264574,72.)) ;
#43552 = CARTESIAN_POINT('Origin',(-30.2227652776365,6.89814895264574,70.)) ;
#43553 = CARTESIAN_POINT('',(-32.1105319382533,7.55870707655606,70.)) ;
#43554 = CARTESIAN_POINT('Origin',(-30.2227652776365,6.89814895264574,70.)) ;
#43555 = CARTESIAN_POINT('Origin',(-30.2227652776365,6.89814895264574,70.)) ;
#43556 = CARTESIAN_POINT('Origin',(-27.930034904975,13.4503959126443,70.)) ;
#43557 = CARTESIAN_POINT('',(-27.930034904975,13.4503959126443,68.)) ;
#43558 = CARTESIAN_POINT('',(-29.8178015655917,14.1109540365546,70.)) ;
#43559 = CARTESIAN_POINT('Origin',(-27.930034904975,13.4503959126443,70.)) ;
#43560 = CARTESIAN_POINT('',(-27.930034904975,13.4503959126443,72.)) ;
#43561 = CARTESIAN_POINT('Origin',(-27.930034904975,13.4503959126443,70.)) ;
#43562 = CARTESIAN_POINT('',(-29.6234833034316,14.514460065675,70.)) ;
#43563 = CARTESIAN_POINT('Origin',(-27.930034904975,13.4503959126443,70.)) ;
#43564 = CARTESIAN_POINT('Origin',(-27.930034904975,13.4503959126443,70.)) ;
#43565 = CARTESIAN_POINT('Origin',(-24.2367759565089,19.3281838576208,70.)) ;
#43566 = CARTESIAN_POINT('',(-24.236775956509,19.3281838576208,68.)) ;
#43567 = CARTESIAN_POINT('',(-25.9302243549655,20.3922480106514,70.)) ;
#43568 = CARTESIAN_POINT('Origin',(-24.2367759565089,19.3281838576208,70.)) ;
#43569 = CARTESIAN_POINT('',(-24.236775956509,19.3281838576208,72.)) ;
#43570 = CARTESIAN_POINT('Origin',(-24.2367759565089,19.3281838576208,70.)) ;
#43571 = CARTESIAN_POINT('',(-25.650989518882,20.7423974199938,70.)) ;
#43572 = CARTESIAN_POINT('Origin',(-24.2367759565089,19.3281838576208,70.)) ;
#43573 = CARTESIAN_POINT('Origin',(-24.2367759565089,19.3281838576208,70.)) ;
#43574 = CARTESIAN_POINT('Origin',(-19.3281838576207,24.2367759565089,70.)) ;
#43575 = CARTESIAN_POINT('',(-19.3281838576207,24.2367759565089,68.)) ;
#43576 = CARTESIAN_POINT('',(-20.7423974199938,25.650989518882,70.)) ;
#43577 = CARTESIAN_POINT('Origin',(-19.3281838576207,24.2367759565089,70.)) ;
#43578 = CARTESIAN_POINT('',(-19.3281838576207,24.2367759565089,72.)) ;
#43579 = CARTESIAN_POINT('Origin',(-19.3281838576207,24.2367759565089,70.)) ;
#43580 = CARTESIAN_POINT('',(-20.3922480106514,25.9302243549655,70.)) ;
#43581 = CARTESIAN_POINT('Origin',(-19.3281838576207,24.2367759565089,70.)) ;
#43582 = CARTESIAN_POINT('Origin',(-19.3281838576207,24.2367759565089,70.)) ;
#43583 = CARTESIAN_POINT('Origin',(-13.4503959126443,27.930034904975,70.)) ;
#43584 = CARTESIAN_POINT('',(-13.4503959126443,27.930034904975,68.)) ;
#43585 = CARTESIAN_POINT('',(-14.514460065675,29.6234833034316,70.)) ;
#43586 = CARTESIAN_POINT('Origin',(-13.4503959126443,27.930034904975,70.)) ;
#43587 = CARTESIAN_POINT('',(-13.4503959126443,27.930034904975,72.)) ;
#43588 = CARTESIAN_POINT('Origin',(-13.4503959126443,27.930034904975,70.)) ;
#43589 = CARTESIAN_POINT('',(-14.1109540365547,29.8178015655917,70.)) ;
#43590 = CARTESIAN_POINT('Origin',(-13.4503959126443,27.930034904975,70.)) ;
#43591 = CARTESIAN_POINT('Origin',(-13.4503959126443,27.930034904975,70.)) ;
#43592 = CARTESIAN_POINT('Origin',(-6.89814895264574,30.2227652776365,70.)) ;
#43593 = CARTESIAN_POINT('',(-6.89814895264573,30.2227652776365,68.)) ;
#43594 = CARTESIAN_POINT('',(-7.55870707655608,32.1105319382533,70.)) ;
#43595 = CARTESIAN_POINT('Origin',(-6.89814895264574,30.2227652776365,70.)) ;
#43596 = CARTESIAN_POINT('',(-6.89814895264573,30.2227652776365,72.)) ;
#43597 = CARTESIAN_POINT('Origin',(-6.89814895264574,30.2227652776365,70.)) ;
#43598 = CARTESIAN_POINT('',(-7.12207790485237,32.210189697423,70.)) ;
#43599 = CARTESIAN_POINT('Origin',(-6.89814895264574,30.2227652776365,70.)) ;
#43600 = CARTESIAN_POINT('Origin',(-6.89814895264574,30.2227652776365,70.)) ;
#43601 = CARTESIAN_POINT('Origin',(1.8982025386784E-15,31.,70.)) ;
#43602 = CARTESIAN_POINT('',(5.66772075275322E-15,31.,68.)) ;
#43603 = CARTESIAN_POINT('',(-0.223928952206612,32.9874244197865,70.)) ;
#43604 = CARTESIAN_POINT('Origin',(1.77635683940025E-15,31.,70.)) ;
#43605 = CARTESIAN_POINT('',(5.66772075275322E-15,31.,72.)) ;
#43606 = CARTESIAN_POINT('Origin',(1.77635683940025E-15,31.,70.)) ;
#43607 = CARTESIAN_POINT('Origin',(1.77635683940025E-15,31.,70.)) ;
#43608 = CARTESIAN_POINT('Origin',(6.89814895264575,30.2227652776365,70.)) ;
#43609 = CARTESIAN_POINT('',(6.89814895264576,30.2227652776366,68.)) ;
#43610 = CARTESIAN_POINT('',(6.89814895264576,30.2227652776366,72.)) ;
#43611 = CARTESIAN_POINT('Origin',(6.89814895264575,30.2227652776365,70.)) ;
#43612 = CARTESIAN_POINT('Origin',(6.89814895264575,30.2227652776365,70.)) ;
#43613 = CARTESIAN_POINT('Origin',(13.4503959126443,27.930034904975,70.)) ;
#43614 = CARTESIAN_POINT('',(13.4503959126443,27.930034904975,68.)) ;
#43615 = CARTESIAN_POINT('',(13.4503959126443,27.930034904975,72.)) ;
#43616 = CARTESIAN_POINT('Origin',(13.4503959126443,27.930034904975,70.)) ;
#43617 = CARTESIAN_POINT('Origin',(13.4503959126443,27.930034904975,70.)) ;
#43618 = CARTESIAN_POINT('Origin',(19.3281838576207,24.2367759565089,70.)) ;
#43619 = CARTESIAN_POINT('',(19.3281838576208,24.236775956509,68.)) ;
#43620 = CARTESIAN_POINT('',(19.3281838576208,24.236775956509,72.)) ;
#43621 = CARTESIAN_POINT('Origin',(19.3281838576207,24.2367759565089,70.)) ;
#43622 = CARTESIAN_POINT('Origin',(19.3281838576207,24.2367759565089,70.)) ;
#43623 = CARTESIAN_POINT('Origin',(24.2367759565089,19.3281838576207,70.)) ;
#43624 = CARTESIAN_POINT('',(24.2367759565089,19.3281838576207,68.)) ;
#43625 = CARTESIAN_POINT('',(24.2367759565089,19.3281838576207,72.)) ;
#43626 = CARTESIAN_POINT('Origin',(24.2367759565089,19.3281838576207,70.)) ;
#43627 = CARTESIAN_POINT('Origin',(24.2367759565089,19.3281838576207,70.)) ;
#43628 = CARTESIAN_POINT('Origin',(27.930034904975,13.4503959126443,70.)) ;
#43629 = CARTESIAN_POINT('',(27.930034904975,13.4503959126443,68.)) ;
#43630 = CARTESIAN_POINT('',(27.930034904975,13.4503959126443,72.)) ;
#43631 = CARTESIAN_POINT('Origin',(27.930034904975,13.4503959126443,70.)) ;
#43632 = CARTESIAN_POINT('Origin',(27.930034904975,13.4503959126443,70.)) ;
#43633 = CARTESIAN_POINT('Origin',(30.2227652776365,6.89814895264575,70.)) ;
#43634 = CARTESIAN_POINT('',(30.2227652776365,6.89814895264574,68.)) ;
#43635 = CARTESIAN_POINT('',(30.2227652776365,6.89814895264574,72.)) ;
#43636 = CARTESIAN_POINT('Origin',(30.2227652776365,6.89814895264575,70.)) ;
#43637 = CARTESIAN_POINT('Origin',(30.2227652776365,6.89814895264575,70.)) ;
#43638 = CARTESIAN_POINT('Origin',(30.6113826388183,-3.44907447632288,70.)) ;
#43639 = CARTESIAN_POINT('',(28.9873448468396,1.4210854715202E-14,70.)) ;
#43640 = CARTESIAN_POINT('Origin',(31.,-1.37667655053519E-14,70.)) ;
#43641 = CARTESIAN_POINT('Origin',(31.,-1.37667655053519E-14,70.)) ;
#43642 = CARTESIAN_POINT('',(28.2605715912239,-6.4502910482325,70.)) ;
#43643 = CARTESIAN_POINT('',(28.6239582190318,-3.22514552411626,70.)) ;
#43644 = CARTESIAN_POINT('Origin',(30.2227652776365,-6.89814895264574,70.)) ;
#43645 = CARTESIAN_POINT('Origin',(30.2227652776365,-6.89814895264574,70.)) ;
#43646 = CARTESIAN_POINT('Origin',(29.0764000913058,-10.174272432645,70.)) ;
#43647 = CARTESIAN_POINT('',(26.1166952701541,-12.5771375692368,70.)) ;
#43648 = CARTESIAN_POINT('',(27.188633430689,-9.51371430873468,70.)) ;
#43649 = CARTESIAN_POINT('Origin',(27.930034904975,-13.4503959126443,70.)) ;
#43650 = CARTESIAN_POINT('Origin',(27.930034904975,-13.4503959126443,70.)) ;
#43651 = CARTESIAN_POINT('Origin',(26.083405430742,-16.3892898851325,70.)) ;
#43652 = CARTESIAN_POINT('',(22.6632187944166,-18.0733138949668,70.)) ;
#43653 = CARTESIAN_POINT('',(24.3899570322854,-15.3252257321018,70.)) ;
#43654 = CARTESIAN_POINT('Origin',(24.2367759565089,-19.3281838576207,70.)) ;
#43655 = CARTESIAN_POINT('Origin',(24.2367759565089,-19.3281838576207,70.)) ;
#43656 = CARTESIAN_POINT('Origin',(21.7824799070648,-21.7824799070648,70.)) ;
#43657 = CARTESIAN_POINT('',(18.0733138949668,-22.6632187944167,70.)) ;
#43658 = CARTESIAN_POINT('',(20.3682663446917,-20.3682663446917,70.)) ;
#43659 = CARTESIAN_POINT('Origin',(19.3281838576207,-24.2367759565089,70.)) ;
#43660 = CARTESIAN_POINT('Origin',(19.3281838576207,-24.2367759565089,70.)) ;
#43661 = CARTESIAN_POINT('Origin',(16.3892898851325,-26.083405430742,70.)) ;
#43662 = CARTESIAN_POINT('',(12.5771375692369,-26.1166952701541,70.)) ;
#43663 = CARTESIAN_POINT('',(15.3252257321018,-24.3899570322854,70.)) ;
#43664 = CARTESIAN_POINT('Origin',(13.4503959126443,-27.930034904975,70.)) ;
#43665 = CARTESIAN_POINT('Origin',(13.4503959126443,-27.930034904975,70.)) ;
#43666 = CARTESIAN_POINT('Origin',(10.174272432645,-29.0764000913058,70.)) ;
#43667 = CARTESIAN_POINT('',(6.45029104823252,-28.2605715912239,70.)) ;
#43668 = CARTESIAN_POINT('',(9.51371430873467,-27.188633430689,70.)) ;
#43669 = CARTESIAN_POINT('Origin',(6.89814895264574,-30.2227652776365,70.)) ;
#43670 = CARTESIAN_POINT('Origin',(6.89814895264574,-30.2227652776365,70.)) ;
#43671 = CARTESIAN_POINT('Origin',(3.44907447632285,-30.6113826388183,70.)) ;
#43672 = CARTESIAN_POINT('',(3.37507799486048E-14,-28.9873448468396,70.)) ;
#43673 = CARTESIAN_POINT('',(3.22514552411624,-28.6239582190318,70.)) ;
#43674 = CARTESIAN_POINT('Origin',(9.76996261670138E-15,-31.,70.)) ;
#43675 = CARTESIAN_POINT('Origin',(9.76996261670138E-15,-31.,70.)) ;
#43676 = CARTESIAN_POINT('Origin',(-3.44907447632288,-30.6113826388183,70.)) ;
#43677 = CARTESIAN_POINT('',(-3.67300342852949,-32.5988070586048,70.)) ;
#43678 = CARTESIAN_POINT('Origin',(-6.89814895264573,-30.2227652776365,70.)) ;
#43679 = CARTESIAN_POINT('Origin',(-10.174272432645,-29.0764000913058,70.)) ;
#43680 = CARTESIAN_POINT('',(-10.8348305565554,-30.9641667519225,70.)) ;
#43681 = CARTESIAN_POINT('Origin',(-13.4503959126443,-27.930034904975,70.)) ;
#43682 = CARTESIAN_POINT('Origin',(-16.3892898851325,-26.083405430742,70.)) ;
#43683 = CARTESIAN_POINT('',(-17.4533540381632,-27.7768538291985,70.)) ;
#43684 = CARTESIAN_POINT('Origin',(-19.3281838576207,-24.2367759565089,70.)) ;
#43685 = CARTESIAN_POINT('Origin',(-21.7824799070648,-21.7824799070648,70.)) ;
#43686 = CARTESIAN_POINT('',(-23.1966934694379,-23.1966934694379,70.)) ;
#43687 = CARTESIAN_POINT('Origin',(-24.2367759565089,-19.3281838576207,70.)) ;
#43688 = CARTESIAN_POINT('Origin',(-26.083405430742,-16.3892898851325,70.)) ;
#43689 = CARTESIAN_POINT('',(-27.7768538291985,-17.4533540381632,70.)) ;
#43690 = CARTESIAN_POINT('Origin',(-27.930034904975,-13.4503959126443,70.)) ;
#43691 = CARTESIAN_POINT('Origin',(-29.0764000913058,-10.174272432645,70.)) ;
#43692 = CARTESIAN_POINT('',(-30.9641667519225,-10.8348305565553,70.)) ;
#43693 = CARTESIAN_POINT('Origin',(-30.2227652776365,-6.89814895264575,70.)) ;
#43694 = CARTESIAN_POINT('Origin',(-30.6113826388183,-3.44907447632286,70.)) ;
#43695 = CARTESIAN_POINT('',(-32.5988070586048,-3.67300342852948,70.)) ;
#43696 = CARTESIAN_POINT('Origin',(-31.,-1.86517468137026E-14,70.)) ;
#43697 = CARTESIAN_POINT('Origin',(-30.6113826388183,3.44907447632287,70.)) ;
#43698 = CARTESIAN_POINT('',(-32.5988070586048,3.67300342852949,70.)) ;
#43699 = CARTESIAN_POINT('Origin',(-30.2227652776365,6.89814895264573,70.)) ;
#43700 = CARTESIAN_POINT('Origin',(-29.0764000913058,10.174272432645,70.)) ;
#43701 = CARTESIAN_POINT('',(-30.9641667519225,10.8348305565554,70.)) ;
#43702 = CARTESIAN_POINT('Origin',(-27.930034904975,13.4503959126443,70.)) ;
#43703 = CARTESIAN_POINT('Origin',(-26.083405430742,16.3892898851325,70.)) ;
#43704 = CARTESIAN_POINT('',(-27.7768538291985,17.4533540381632,70.)) ;
#43705 = CARTESIAN_POINT('Origin',(-24.2367759565089,19.3281838576207,70.)) ;
#43706 = CARTESIAN_POINT('Origin',(-21.7824799070648,21.7824799070648,70.)) ;
#43707 = CARTESIAN_POINT('',(-23.1966934694379,23.1966934694379,70.)) ;
#43708 = CARTESIAN_POINT('Origin',(-19.3281838576207,24.2367759565089,70.)) ;
#43709 = CARTESIAN_POINT('Origin',(-16.3892898851325,26.083405430742,70.)) ;
#43710 = CARTESIAN_POINT('',(-17.4533540381632,27.7768538291985,70.)) ;
#43711 = CARTESIAN_POINT('Origin',(-13.4503959126443,27.930034904975,70.)) ;
#43712 = CARTESIAN_POINT('Origin',(-10.174272432645,29.0764000913058,70.)) ;
#43713 = CARTESIAN_POINT('',(-10.8348305565554,30.9641667519225,70.)) ;
#43714 = CARTESIAN_POINT('Origin',(-6.89814895264576,30.2227652776365,70.)) ;
#43715 = CARTESIAN_POINT('Origin',(-3.44907447632287,30.6113826388183,70.)) ;
#43716 = CARTESIAN_POINT('',(-3.67300342852949,32.5988070586048,70.)) ;
#43717 = CARTESIAN_POINT('',(-5.10980147083728E-14,28.9873448468396,70.)) ;
#43718 = CARTESIAN_POINT('Origin',(-2.39808173319034E-14,31.,70.)) ;
#43719 = CARTESIAN_POINT('Origin',(-2.39808173319034E-14,31.,70.)) ;
#43720 = CARTESIAN_POINT('Origin',(3.44907447632287,30.6113826388183,70.)) ;
#43721 = CARTESIAN_POINT('',(6.45029104823248,28.2605715912239,70.)) ;
#43722 = CARTESIAN_POINT('',(3.22514552411626,28.6239582190318,70.)) ;
#43723 = CARTESIAN_POINT('Origin',(6.89814895264572,30.2227652776365,70.)) ;
#43724 = CARTESIAN_POINT('Origin',(6.89814895264572,30.2227652776365,70.)) ;
#43725 = CARTESIAN_POINT('Origin',(10.174272432645,29.0764000913058,70.)) ;
#43726 = CARTESIAN_POINT('',(12.5771375692369,26.1166952701541,70.)) ;
#43727 = CARTESIAN_POINT('',(9.51371430873469,27.188633430689,70.)) ;
#43728 = CARTESIAN_POINT('Origin',(13.4503959126443,27.930034904975,70.)) ;
#43729 = CARTESIAN_POINT('Origin',(13.4503959126443,27.930034904975,70.)) ;
#43730 = CARTESIAN_POINT('Origin',(16.3892898851325,26.083405430742,70.)) ;
#43731 = CARTESIAN_POINT('',(18.0733138949668,22.6632187944167,70.)) ;
#43732 = CARTESIAN_POINT('',(15.3252257321019,24.3899570322854,70.)) ;
#43733 = CARTESIAN_POINT('Origin',(19.3281838576207,24.2367759565089,70.)) ;
#43734 = CARTESIAN_POINT('Origin',(19.3281838576207,24.2367759565089,70.)) ;
#43735 = CARTESIAN_POINT('Origin',(21.7824799070648,21.7824799070648,70.)) ;
#43736 = CARTESIAN_POINT('',(22.6632187944166,18.0733138949668,70.)) ;
#43737 = CARTESIAN_POINT('',(20.3682663446917,20.3682663446917,70.)) ;
#43738 = CARTESIAN_POINT('Origin',(24.2367759565089,19.3281838576207,70.)) ;
#43739 = CARTESIAN_POINT('Origin',(24.2367759565089,19.3281838576207,70.)) ;
#43740 = CARTESIAN_POINT('Origin',(26.083405430742,16.3892898851325,70.)) ;
#43741 = CARTESIAN_POINT('',(26.1166952701541,12.5771375692369,70.)) ;
#43742 = CARTESIAN_POINT('',(24.3899570322854,15.3252257321018,70.)) ;
#43743 = CARTESIAN_POINT('Origin',(27.930034904975,13.4503959126443,70.)) ;
#43744 = CARTESIAN_POINT('Origin',(27.930034904975,13.4503959126443,70.)) ;
#43745 = CARTESIAN_POINT('Origin',(29.0764000913058,10.174272432645,70.)) ;
#43746 = CARTESIAN_POINT('',(28.2605715912239,6.45029104823255,70.)) ;
#43747 = CARTESIAN_POINT('',(27.188633430689,9.51371430873469,70.)) ;
#43748 = CARTESIAN_POINT('Origin',(30.2227652776365,6.89814895264576,70.)) ;
#43749 = CARTESIAN_POINT('Origin',(30.2227652776365,6.89814895264576,70.)) ;
#43750 = CARTESIAN_POINT('Origin',(30.6113826388183,3.44907447632287,70.)) ;
#43751 = CARTESIAN_POINT('',(28.6239582190318,3.22514552411626,70.)) ;
#43752 = CARTESIAN_POINT('',(0.,0.,0.)) ;
#43753 = CARTESIAN_POINT('',(0.,0.,0.)) ;
#43754 = CARTESIAN_POINT('',(-10.,0.,0.)) ;
#43755 = CARTESIAN_POINT('',(10.,0.,0.)) ;
#43756 = CARTESIAN_POINT('',(0.,0.,0.)) ;
#43757 = CARTESIAN_POINT('',(0.,0.,0.)) ;
#43758 = CARTESIAN_POINT('',(0.,0.,0.)) ;
#43759 = CARTESIAN_POINT('',(0.,0.,0.)) ;
#43760 = CARTESIAN_POINT('Origin',(-8.5,-22.,29.)) ;
#43761 = CARTESIAN_POINT('',(-9.15,-22.,30.9)) ;
#43762 = CARTESIAN_POINT('Origin',(-8.5,-22.,30.9)) ;
#43763 = CARTESIAN_POINT('',(-9.15,-22.,31.)) ;
#43764 = CARTESIAN_POINT('',(-9.15,-22.,29.)) ;
#43765 = CARTESIAN_POINT('Origin',(-8.5,-22.,31.)) ;
#43766 = CARTESIAN_POINT('Origin',(-8.5,-22.,29.)) ;
#43767 = CARTESIAN_POINT('',(-9.15,-22.,27.)) ;
#43768 = CARTESIAN_POINT('Origin',(-8.5,-22.,27.)) ;
#43769 = CARTESIAN_POINT('',(-9.15,-22.,27.1)) ;
#43770 = CARTESIAN_POINT('',(-9.15,-22.,29.)) ;
#43771 = CARTESIAN_POINT('Origin',(-8.5,-22.,27.1)) ;
#43772 = CARTESIAN_POINT('Origin',(-8.5,22.,29.)) ;
#43773 = CARTESIAN_POINT('',(-9.15,22.,30.9)) ;
#43774 = CARTESIAN_POINT('Origin',(-8.5,22.,30.9)) ;
#43775 = CARTESIAN_POINT('',(-9.15,22.,31.)) ;
#43776 = CARTESIAN_POINT('',(-9.15,22.,29.)) ;
#43777 = CARTESIAN_POINT('Origin',(-8.5,22.,31.)) ;
#43778 = CARTESIAN_POINT('Origin',(-8.5,22.,29.)) ;
#43779 = CARTESIAN_POINT('',(-9.15,22.,27.)) ;
#43780 = CARTESIAN_POINT('Origin',(-8.5,22.,27.)) ;
#43781 = CARTESIAN_POINT('',(-9.15,22.,27.1)) ;
#43782 = CARTESIAN_POINT('',(-9.15,22.,29.)) ;
#43783 = CARTESIAN_POINT('Origin',(-8.5,22.,27.1)) ;
#43784 = CARTESIAN_POINT('Origin',(8.5,-22.,29.)) ;
#43785 = CARTESIAN_POINT('',(7.85,-22.,30.9)) ;
#43786 = CARTESIAN_POINT('Origin',(8.5,-22.,30.9)) ;
#43787 = CARTESIAN_POINT('',(7.85,-22.,31.)) ;
#43788 = CARTESIAN_POINT('',(7.85,-22.,29.)) ;
#43789 = CARTESIAN_POINT('Origin',(8.5,-22.,31.)) ;
#43790 = CARTESIAN_POINT('Origin',(8.5,-22.,29.)) ;
#43791 = CARTESIAN_POINT('',(7.85,-22.,27.)) ;
#43792 = CARTESIAN_POINT('Origin',(8.5,-22.,27.)) ;
#43793 = CARTESIAN_POINT('',(7.85,-22.,27.1)) ;
#43794 = CARTESIAN_POINT('',(7.85,-22.,29.)) ;
#43795 = CARTESIAN_POINT('Origin',(8.5,-22.,27.1)) ;
#43796 = CARTESIAN_POINT('Origin',(-53.,0.,25.)) ;
#43797 = CARTESIAN_POINT('',(-55.1424285285629,-20.4,27.1)) ;
#43798 = CARTESIAN_POINT('',(-55.1424285285629,-23.6,27.1)) ;
#43799 = CARTESIAN_POINT('',(-55.1424285285629,0.,27.1)) ;
#43800 = CARTESIAN_POINT('',(-50.8575714714371,-23.6,27.1)) ;
#43801 = CARTESIAN_POINT('Origin',(-53.,-23.6,25.)) ;
#43802 = CARTESIAN_POINT('',(-50.8575714714371,-20.4,27.1)) ;
#43803 = CARTESIAN_POINT('',(-50.8575714714371,0.,27.1)) ;
#43804 = CARTESIAN_POINT('Origin',(-53.,-20.4,25.)) ;
#43805 = CARTESIAN_POINT('Origin',(34.6,-22.,29.)) ;
#43806 = CARTESIAN_POINT('',(34.6,-23.6,30.9)) ;
#43807 = CARTESIAN_POINT('',(34.6,-23.6,27.1)) ;
#43808 = CARTESIAN_POINT('',(34.6,-23.6,29.)) ;
#43809 = CARTESIAN_POINT('',(34.6,-20.4,30.9)) ;
#43810 = CARTESIAN_POINT('',(34.6,-22.,30.9)) ;
#43811 = CARTESIAN_POINT('',(34.6,-20.4,27.1)) ;
#43812 = CARTESIAN_POINT('',(34.6,-20.4,29.)) ;
#43813 = CARTESIAN_POINT('',(34.6,-22.,27.1)) ;
#43814 = CARTESIAN_POINT('Origin',(-10.5,-20.4,29.)) ;
#43815 = CARTESIAN_POINT('',(-10.5,-20.4,27.1)) ;
#43816 = CARTESIAN_POINT('',(-55.6,-20.4,30.9)) ;
#43817 = CARTESIAN_POINT('',(-10.5,-20.4,30.9)) ;
#43818 = CARTESIAN_POINT('',(-55.6,-20.4,27.1)) ;
#43819 = CARTESIAN_POINT('',(-55.6,-20.4,29.)) ;
#43820 = CARTESIAN_POINT('',(-10.5,-20.4,27.1)) ;
#43821 = CARTESIAN_POINT('Origin',(-55.6,-22.,29.)) ;
#43822 = CARTESIAN_POINT('',(-55.6,-23.6,30.9)) ;
#43823 = CARTESIAN_POINT('',(-55.6,-22.,30.9)) ;
#43824 = CARTESIAN_POINT('',(-55.6,-23.6,27.1)) ;
#43825 = CARTESIAN_POINT('',(-55.6,-23.6,29.)) ;
#43826 = CARTESIAN_POINT('',(-55.6,-22.,27.1)) ;
#43827 = CARTESIAN_POINT('Origin',(-10.5,-22.,27.1)) ;
#43828 = CARTESIAN_POINT('',(-10.5,-23.6,27.1)) ;
#43829 = CARTESIAN_POINT('Origin',(-10.5,-22.,30.9)) ;
#43830 = CARTESIAN_POINT('',(-10.5,-23.6,30.9)) ;
#43831 = CARTESIAN_POINT('Origin',(-10.5,-22.,27.1)) ;
#43832 = CARTESIAN_POINT('',(-10.5,-23.6,27.1)) ;
#43833 = CARTESIAN_POINT('Origin',(-10.5,-23.6,29.)) ;
#43834 = CARTESIAN_POINT('Origin',(8.5,22.,29.)) ;
#43835 = CARTESIAN_POINT('',(7.85,22.,30.9)) ;
#43836 = CARTESIAN_POINT('Origin',(8.5,22.,30.9)) ;
#43837 = CARTESIAN_POINT('',(7.85,22.,31.)) ;
#43838 = CARTESIAN_POINT('',(7.85,22.,29.)) ;
#43839 = CARTESIAN_POINT('Origin',(8.5,22.,31.)) ;
#43840 = CARTESIAN_POINT('Origin',(8.5,22.,29.)) ;
#43841 = CARTESIAN_POINT('',(7.85,22.,27.)) ;
#43842 = CARTESIAN_POINT('Origin',(8.5,22.,27.)) ;
#43843 = CARTESIAN_POINT('',(7.85,22.,27.1)) ;
#43844 = CARTESIAN_POINT('',(7.85,22.,29.)) ;
#43845 = CARTESIAN_POINT('Origin',(8.5,22.,27.1)) ;
#43846 = CARTESIAN_POINT('Origin',(-53.,0.,25.)) ;
#43847 = CARTESIAN_POINT('',(-55.1424285285629,23.6,27.1)) ;
#43848 = CARTESIAN_POINT('',(-55.1424285285629,20.4,27.1)) ;
#43849 = CARTESIAN_POINT('',(-55.1424285285629,0.,27.1)) ;
#43850 = CARTESIAN_POINT('',(-50.8575714714371,20.4,27.1)) ;
#43851 = CARTESIAN_POINT('Origin',(-53.,20.4,25.)) ;
#43852 = CARTESIAN_POINT('',(-50.8575714714371,23.6,27.1)) ;
#43853 = CARTESIAN_POINT('',(-50.8575714714371,0.,27.1)) ;
#43854 = CARTESIAN_POINT('Origin',(-53.,23.6,25.)) ;
#43855 = CARTESIAN_POINT('Origin',(34.6,22.,29.)) ;
#43856 = CARTESIAN_POINT('',(34.6,20.4,30.9)) ;
#43857 = CARTESIAN_POINT('',(34.6,20.4,27.1)) ;
#43858 = CARTESIAN_POINT('',(34.6,20.4,29.)) ;
#43859 = CARTESIAN_POINT('',(34.6,23.6,30.9)) ;
#43860 = CARTESIAN_POINT('',(34.6,22.,30.9)) ;
#43861 = CARTESIAN_POINT('',(34.6,23.6,27.1)) ;
#43862 = CARTESIAN_POINT('',(34.6,23.6,29.)) ;
#43863 = CARTESIAN_POINT('',(34.6,22.,27.1)) ;
#43864 = CARTESIAN_POINT('Origin',(-10.5,23.6,29.)) ;
#43865 = CARTESIAN_POINT('',(-10.5,23.6,27.1)) ;
#43866 = CARTESIAN_POINT('',(-55.6,23.6,30.9)) ;
#43867 = CARTESIAN_POINT('',(-10.5,23.6,30.9)) ;
#43868 = CARTESIAN_POINT('',(-55.6,23.6,27.1)) ;
#43869 = CARTESIAN_POINT('',(-55.6,23.6,29.)) ;
#43870 = CARTESIAN_POINT('',(-10.5,23.6,27.1)) ;
#43871 = CARTESIAN_POINT('Origin',(-55.6,22.,29.)) ;
#43872 = CARTESIAN_POINT('',(-55.6,20.4,30.9)) ;
#43873 = CARTESIAN_POINT('',(-55.6,22.,30.9)) ;
#43874 = CARTESIAN_POINT('',(-55.6,20.4,27.1)) ;
#43875 = CARTESIAN_POINT('',(-55.6,20.4,29.)) ;
#43876 = CARTESIAN_POINT('',(-55.6,22.,27.1)) ;
#43877 = CARTESIAN_POINT('Origin',(-10.5,22.,27.1)) ;
#43878 = CARTESIAN_POINT('',(-10.5,20.4,27.1)) ;
#43879 = CARTESIAN_POINT('Origin',(-10.5,22.,30.9)) ;
#43880 = CARTESIAN_POINT('',(-10.5,20.4,30.9)) ;
#43881 = CARTESIAN_POINT('Origin',(-10.5,22.,27.1)) ;
#43882 = CARTESIAN_POINT('',(-10.5,20.4,27.1)) ;
#43883 = CARTESIAN_POINT('Origin',(-10.5,20.4,29.)) ;
#43884 = CARTESIAN_POINT('Origin',(-53.,0.,90.)) ;
#43885 = CARTESIAN_POINT('',(-54.28,-4.8,90.)) ;
#43886 = CARTESIAN_POINT('Origin',(-53.,-4.8,90.)) ;
#43887 = CARTESIAN_POINT('',(-54.28,-4.,90.)) ;
#43888 = CARTESIAN_POINT('',(-54.28,0.,90.)) ;
#43889 = CARTESIAN_POINT('Origin',(-53.,-4.,90.)) ;
#43890 = CARTESIAN_POINT('Origin',(-53.,0.,90.)) ;
#43891 = CARTESIAN_POINT('',(-54.28,4.,90.)) ;
#43892 = CARTESIAN_POINT('Origin',(-53.,4.,90.)) ;
#43893 = CARTESIAN_POINT('',(-54.28,4.8,90.)) ;
#43894 = CARTESIAN_POINT('',(-54.28,0.,90.)) ;
#43895 = CARTESIAN_POINT('Origin',(-53.,4.8,90.)) ;
#43896 = CARTESIAN_POINT('Origin',(-21.92,-21.92,49.5)) ;
#43897 = CARTESIAN_POINT('',(-23.12,-21.92,31.)) ;
#43898 = CARTESIAN_POINT('Origin',(-21.92,-21.92,31.)) ;
#43899 = CARTESIAN_POINT('',(-23.12,-21.92,68.)) ;
#43900 = CARTESIAN_POINT('',(-23.12,-21.92,49.5)) ;
#43901 = CARTESIAN_POINT('Origin',(-21.92,-21.92,68.)) ;
#43902 = CARTESIAN_POINT('Origin',(-21.92,-21.92,49.5)) ;
#43903 = CARTESIAN_POINT('',(-23.42,-21.92,68.)) ;
#43904 = CARTESIAN_POINT('Origin',(-21.92,-21.92,68.)) ;
#43905 = CARTESIAN_POINT('',(-23.42,-21.92,31.)) ;
#43906 = CARTESIAN_POINT('',(-23.42,-21.92,49.5)) ;
#43907 = CARTESIAN_POINT('Origin',(-21.92,-21.92,31.)) ;
#43908 = CARTESIAN_POINT('Origin',(-21.92,-21.92,68.)) ;
#43909 = CARTESIAN_POINT('Origin',(-10.5,-22.,31.)) ;
#43910 = CARTESIAN_POINT('',(35.,-24.,31.)) ;
#43911 = CARTESIAN_POINT('',(35.,-20.,31.)) ;
#43912 = CARTESIAN_POINT('',(35.,-22.,31.)) ;
#43913 = CARTESIAN_POINT('',(-56.,-20.,31.)) ;
#43914 = CARTESIAN_POINT('',(-10.5,-20.,31.)) ;
#43915 = CARTESIAN_POINT('',(-56.,-24.,31.)) ;
#43916 = CARTESIAN_POINT('',(-56.,-22.,31.)) ;
#43917 = CARTESIAN_POINT('',(-50.,-24.,31.)) ;
#43918 = CARTESIAN_POINT('',(-31.75,-24.,31.)) ;
#43919 = CARTESIAN_POINT('',(-10.5,-24.,31.)) ;
#43920 = CARTESIAN_POINT('',(20.42,-21.92,31.)) ;
#43921 = CARTESIAN_POINT('Origin',(21.92,-21.92,31.)) ;
#43922 = CARTESIAN_POINT('Origin',(21.92,-21.92,49.5)) ;
#43923 = CARTESIAN_POINT('',(20.72,-21.92,31.)) ;
#43924 = CARTESIAN_POINT('Origin',(21.92,-21.92,31.)) ;
#43925 = CARTESIAN_POINT('',(20.72,-21.92,68.)) ;
#43926 = CARTESIAN_POINT('',(20.72,-21.92,49.5)) ;
#43927 = CARTESIAN_POINT('Origin',(21.92,-21.92,68.)) ;
#43928 = CARTESIAN_POINT('Origin',(21.92,-21.92,49.5)) ;
#43929 = CARTESIAN_POINT('',(20.42,-21.92,68.)) ;
#43930 = CARTESIAN_POINT('Origin',(21.92,-21.92,68.)) ;
#43931 = CARTESIAN_POINT('',(20.42,-21.92,49.5)) ;
#43932 = CARTESIAN_POINT('Origin',(21.92,-21.92,68.)) ;
#43933 = CARTESIAN_POINT('Origin',(-10.5,-22.,31.)) ;
#43934 = CARTESIAN_POINT('Origin',(22.,-20.4,13.8)) ;
#43935 = CARTESIAN_POINT('',(20.4,-20.4,27.)) ;
#43936 = CARTESIAN_POINT('',(23.6,-20.4,27.)) ;
#43937 = CARTESIAN_POINT('',(5.75,-20.4,27.)) ;
#43938 = CARTESIAN_POINT('',(20.4,-20.4,0.6)) ;
#43939 = CARTESIAN_POINT('',(20.4,-20.4,13.8)) ;
#43940 = CARTESIAN_POINT('',(23.6,-20.4,0.6)) ;
#43941 = CARTESIAN_POINT('',(22.,-20.4,0.6)) ;
#43942 = CARTESIAN_POINT('',(23.6,-20.4,13.8)) ;
#43943 = CARTESIAN_POINT('Origin',(23.6,-22.,13.8)) ;
#43944 = CARTESIAN_POINT('',(23.6,-23.6,27.)) ;
#43945 = CARTESIAN_POINT('',(23.6,-22.,27.)) ;
#43946 = CARTESIAN_POINT('',(23.6,-23.6,0.6)) ;
#43947 = CARTESIAN_POINT('',(23.6,-22.,0.6)) ;
#43948 = CARTESIAN_POINT('',(23.6,-23.6,13.8)) ;
#43949 = CARTESIAN_POINT('Origin',(22.,-23.6,13.8)) ;
#43950 = CARTESIAN_POINT('',(20.4,-23.6,27.)) ;
#43951 = CARTESIAN_POINT('',(5.75,-23.6,27.)) ;
#43952 = CARTESIAN_POINT('',(20.4,-23.6,0.6)) ;
#43953 = CARTESIAN_POINT('',(22.,-23.6,0.6)) ;
#43954 = CARTESIAN_POINT('',(20.4,-23.6,13.8)) ;
#43955 = CARTESIAN_POINT('Origin',(20.4,-22.,13.8)) ;
#43956 = CARTESIAN_POINT('',(20.4,-22.,27.)) ;
#43957 = CARTESIAN_POINT('',(20.4,-22.,0.6)) ;
#43958 = CARTESIAN_POINT('Origin',(22.,-22.,0.6)) ;
#43959 = CARTESIAN_POINT('',(24.,-20.,0.6)) ;
#43960 = CARTESIAN_POINT('',(24.,-24.,0.6)) ;
#43961 = CARTESIAN_POINT('',(24.,-22.,0.6)) ;
#43962 = CARTESIAN_POINT('',(20.,-24.,0.6)) ;
#43963 = CARTESIAN_POINT('',(22.,-24.,0.6)) ;
#43964 = CARTESIAN_POINT('',(20.,-20.,0.6)) ;
#43965 = CARTESIAN_POINT('',(20.,-22.,0.6)) ;
#43966 = CARTESIAN_POINT('',(22.,-20.,0.6)) ;
#43967 = CARTESIAN_POINT('Origin',(20.,-22.,13.8)) ;
#43968 = CARTESIAN_POINT('',(20.,-20.,27.)) ;
#43969 = CARTESIAN_POINT('',(20.,-20.,13.8)) ;
#43970 = CARTESIAN_POINT('',(20.,-24.,27.)) ;
#43971 = CARTESIAN_POINT('',(20.,-24.,13.8)) ;
#43972 = CARTESIAN_POINT('',(20.,-22.,27.)) ;
#43973 = CARTESIAN_POINT('Origin',(24.,-22.,13.8)) ;
#43974 = CARTESIAN_POINT('',(24.,-24.,27.)) ;
#43975 = CARTESIAN_POINT('',(24.,-24.,13.8)) ;
#43976 = CARTESIAN_POINT('',(24.,-20.,27.)) ;
#43977 = CARTESIAN_POINT('',(24.,-20.,13.8)) ;
#43978 = CARTESIAN_POINT('',(24.,-22.,27.)) ;
#43979 = CARTESIAN_POINT('Origin',(-10.5,-22.,27.)) ;
#43980 = CARTESIAN_POINT('',(-50.,-24.,27.)) ;
#43981 = CARTESIAN_POINT('',(-10.5,-24.,27.)) ;
#43982 = CARTESIAN_POINT('',(-50.7639320225002,-24.,27.)) ;
#43983 = CARTESIAN_POINT('',(-31.75,-24.,27.)) ;
#43984 = CARTESIAN_POINT('',(-50.7639320225002,-20.,27.)) ;
#43985 = CARTESIAN_POINT('',(-50.7639320225002,0.,27.)) ;
#43986 = CARTESIAN_POINT('',(-10.5,-20.,27.)) ;
#43987 = CARTESIAN_POINT('Origin',(-10.5,-22.,27.)) ;
#43988 = CARTESIAN_POINT('Origin',(-10.5,22.,27.)) ;
#43989 = CARTESIAN_POINT('',(-55.2360679774998,20.,27.)) ;
#43990 = CARTESIAN_POINT('',(-55.2360679774998,24.,27.)) ;
#43991 = CARTESIAN_POINT('',(-55.2360679774998,0.,27.)) ;
#43992 = CARTESIAN_POINT('',(-56.,20.,27.)) ;
#43993 = CARTESIAN_POINT('',(-10.5,20.,27.)) ;
#43994 = CARTESIAN_POINT('',(-56.,24.,27.)) ;
#43995 = CARTESIAN_POINT('',(-56.,22.,27.)) ;
#43996 = CARTESIAN_POINT('',(-31.75,24.,27.)) ;
#43997 = CARTESIAN_POINT('Origin',(-10.5,22.,31.)) ;
#43998 = CARTESIAN_POINT('',(20.72,21.92,31.)) ;
#43999 = CARTESIAN_POINT('Origin',(21.92,21.92,31.)) ;
#44000 = CARTESIAN_POINT('Origin',(-10.5,22.,27.)) ;
#44001 = CARTESIAN_POINT('',(24.,20.,27.)) ;
#44002 = CARTESIAN_POINT('',(24.,24.,27.)) ;
#44003 = CARTESIAN_POINT('',(24.,22.,27.)) ;
#44004 = CARTESIAN_POINT('',(35.,24.,27.)) ;
#44005 = CARTESIAN_POINT('',(-10.5,24.,27.)) ;
#44006 = CARTESIAN_POINT('',(35.,20.,27.)) ;
#44007 = CARTESIAN_POINT('',(35.,22.,27.)) ;
#44008 = CARTESIAN_POINT('',(-10.5,20.,27.)) ;
#44009 = CARTESIAN_POINT('Origin',(-10.5,20.,29.)) ;
#44010 = CARTESIAN_POINT('',(-50.7639320225002,20.,27.)) ;
#44011 = CARTESIAN_POINT('Origin',(-53.,20.,25.)) ;
#44012 = CARTESIAN_POINT('',(20.,20.,27.)) ;
#44013 = CARTESIAN_POINT('',(-10.5,20.,27.)) ;
#44014 = CARTESIAN_POINT('',(20.,20.,0.6)) ;
#44015 = CARTESIAN_POINT('',(20.,20.,13.8)) ;
#44016 = CARTESIAN_POINT('',(24.,20.,0.6)) ;
#44017 = CARTESIAN_POINT('',(22.,20.,0.6)) ;
#44018 = CARTESIAN_POINT('',(24.,20.,13.8)) ;
#44019 = CARTESIAN_POINT('',(35.,20.,31.)) ;
#44020 = CARTESIAN_POINT('',(35.,20.,29.)) ;
#44021 = CARTESIAN_POINT('',(-56.,20.,31.)) ;
#44022 = CARTESIAN_POINT('',(-10.5,20.,31.)) ;
#44023 = CARTESIAN_POINT('',(-56.,20.,29.)) ;
#44024 = CARTESIAN_POINT('Origin',(-10.5,24.,29.)) ;
#44025 = CARTESIAN_POINT('',(-50.,24.,31.)) ;
#44026 = CARTESIAN_POINT('',(-50.,24.,27.)) ;
#44027 = CARTESIAN_POINT('',(-50.,24.,43.3)) ;
#44028 = CARTESIAN_POINT('',(35.,24.,31.)) ;
#44029 = CARTESIAN_POINT('',(-10.5,24.,31.)) ;
#44030 = CARTESIAN_POINT('',(35.,24.,29.)) ;
#44031 = CARTESIAN_POINT('',(24.,24.,0.6)) ;
#44032 = CARTESIAN_POINT('',(24.,24.,13.8)) ;
#44033 = CARTESIAN_POINT('',(20.,24.,0.6)) ;
#44034 = CARTESIAN_POINT('',(22.,24.,0.6)) ;
#44035 = CARTESIAN_POINT('',(20.,24.,27.)) ;
#44036 = CARTESIAN_POINT('',(20.,24.,13.8)) ;
#44037 = CARTESIAN_POINT('',(-10.5,24.,27.)) ;
#44038 = CARTESIAN_POINT('Origin',(35.,22.,29.)) ;
#44039 = CARTESIAN_POINT('',(35.,22.,31.)) ;
#44040 = CARTESIAN_POINT('Origin',(-53.,24.,43.3)) ;
#44041 = CARTESIAN_POINT('',(-50.7639320225002,24.,27.)) ;
#44042 = CARTESIAN_POINT('',(-31.75,24.,27.)) ;
#44043 = CARTESIAN_POINT('',(-50.1715728752538,24.,26.)) ;
#44044 = CARTESIAN_POINT('Origin',(-53.,24.,25.)) ;
#44045 = CARTESIAN_POINT('',(-50.,24.,26.)) ;
#44046 = CARTESIAN_POINT('',(-53.,24.,26.)) ;
#44047 = CARTESIAN_POINT('',(-50.,24.,43.3)) ;
#44048 = CARTESIAN_POINT('Origin',(-53.,24.,43.3)) ;
#44049 = CARTESIAN_POINT('',(-56.,24.,26.)) ;
#44050 = CARTESIAN_POINT('',(-56.,24.,43.3)) ;
#44051 = CARTESIAN_POINT('',(-55.8284271247462,24.,26.)) ;
#44052 = CARTESIAN_POINT('',(-53.,24.,26.)) ;
#44053 = CARTESIAN_POINT('Origin',(-53.,24.,25.)) ;
#44054 = CARTESIAN_POINT('Origin',(-53.,0.,26.)) ;
#44055 = CARTESIAN_POINT('',(-50.1715728752538,-24.,26.)) ;
#44056 = CARTESIAN_POINT('',(-50.1715728752538,0.,26.)) ;
#44057 = CARTESIAN_POINT('',(-50.,-24.,26.)) ;
#44058 = CARTESIAN_POINT('',(-53.,-24.,26.)) ;
#44059 = CARTESIAN_POINT('',(-50.,0.,26.)) ;
#44060 = CARTESIAN_POINT('Origin',(-53.,0.,22.)) ;
#44061 = CARTESIAN_POINT('',(-50.4,-24.4,22.)) ;
#44062 = CARTESIAN_POINT('',(-55.6,-24.4,22.)) ;
#44063 = CARTESIAN_POINT('',(-53.,-24.4,22.)) ;
#44064 = CARTESIAN_POINT('',(-50.4,-29.6,22.)) ;
#44065 = CARTESIAN_POINT('',(-50.4,-13.5,22.)) ;
#44066 = CARTESIAN_POINT('',(-55.6,-29.6,22.)) ;
#44067 = CARTESIAN_POINT('',(-53.,-29.6,22.)) ;
#44068 = CARTESIAN_POINT('',(-55.6,-13.5,22.)) ;
#44069 = CARTESIAN_POINT('Origin',(-53.,0.,22.)) ;
#44070 = CARTESIAN_POINT('',(-50.4,29.6,22.)) ;
#44071 = CARTESIAN_POINT('',(-55.6,29.6,22.)) ;
#44072 = CARTESIAN_POINT('',(-53.,29.6,22.)) ;
#44073 = CARTESIAN_POINT('',(-50.4,24.4,22.)) ;
#44074 = CARTESIAN_POINT('',(-50.4,13.5,22.)) ;
#44075 = CARTESIAN_POINT('',(-55.6,24.4,22.)) ;
#44076 = CARTESIAN_POINT('',(-53.,24.4,22.)) ;
#44077 = CARTESIAN_POINT('',(-55.6,13.5,22.)) ;
#44078 = CARTESIAN_POINT('Origin',(-53.,0.,22.)) ;
#44079 = CARTESIAN_POINT('',(-50.,24.,22.)) ;
#44080 = CARTESIAN_POINT('',(-56.,24.,22.)) ;
#44081 = CARTESIAN_POINT('',(-53.,24.,22.)) ;
#44082 = CARTESIAN_POINT('',(-50.,-24.,22.)) ;
#44083 = CARTESIAN_POINT('',(-50.,0.,22.)) ;
#44084 = CARTESIAN_POINT('',(-56.,-24.,22.)) ;
#44085 = CARTESIAN_POINT('',(-53.,-24.,22.)) ;
#44086 = CARTESIAN_POINT('',(-56.,0.,22.)) ;
#44087 = CARTESIAN_POINT('Origin',(-53.,0.,26.)) ;
#44088 = CARTESIAN_POINT('',(-56.,-24.,26.)) ;
#44089 = CARTESIAN_POINT('',(-56.,0.,26.)) ;
#44090 = CARTESIAN_POINT('',(-55.8284271247462,-24.,26.)) ;
#44091 = CARTESIAN_POINT('',(-53.,-24.,26.)) ;
#44092 = CARTESIAN_POINT('',(-55.8284271247462,0.,26.)) ;
#44093 = CARTESIAN_POINT('Origin',(-53.,30.,43.3)) ;
#44094 = CARTESIAN_POINT('',(-56.,30.,86.)) ;
#44095 = CARTESIAN_POINT('',(-56.,30.,25.)) ;
#44096 = CARTESIAN_POINT('',(-56.,30.,43.3)) ;
#44097 = CARTESIAN_POINT('',(-50.,30.,86.)) ;
#44098 = CARTESIAN_POINT('',(-53.,30.,86.)) ;
#44099 = CARTESIAN_POINT('',(-50.,30.,25.)) ;
#44100 = CARTESIAN_POINT('',(-50.,30.,43.3)) ;
#44101 = CARTESIAN_POINT('Origin',(-53.,30.,25.)) ;
#44102 = CARTESIAN_POINT('Origin',(-53.,30.,43.3)) ;
#44103 = CARTESIAN_POINT('',(-50.,30.,0.600000000000001)) ;
#44104 = CARTESIAN_POINT('',(-50.,30.,43.3)) ;
#44105 = CARTESIAN_POINT('',(-56.,30.,0.600000000000001)) ;
#44106 = CARTESIAN_POINT('',(-53.,30.,0.600000000000001)) ;
#44107 = CARTESIAN_POINT('',(-56.,30.,43.3)) ;
#44108 = CARTESIAN_POINT('Origin',(-53.,30.,25.)) ;
#44109 = CARTESIAN_POINT('Origin',(-56.,27.,43.3)) ;
#44110 = CARTESIAN_POINT('',(-56.,-4.,82.)) ;
#44111 = CARTESIAN_POINT('',(-56.,-4.,86.)) ;
#44112 = CARTESIAN_POINT('',(-56.,-4.,65.65)) ;
#44113 = CARTESIAN_POINT('',(-56.,4.,86.)) ;
#44114 = CARTESIAN_POINT('',(-56.,27.,86.)) ;
#44115 = CARTESIAN_POINT('',(-56.,4.,82.)) ;
#44116 = CARTESIAN_POINT('',(-56.,4.,65.65)) ;
#44117 = CARTESIAN_POINT('',(-56.,4.8,82.)) ;
#44118 = CARTESIAN_POINT('',(-56.,15.7,82.)) ;
#44119 = CARTESIAN_POINT('',(-56.,4.8,86.)) ;
#44120 = CARTESIAN_POINT('',(-56.,4.8,65.65)) ;
#44121 = CARTESIAN_POINT('',(-56.,27.,86.)) ;
#44122 = CARTESIAN_POINT('',(-56.,24.,0.600000000000001)) ;
#44123 = CARTESIAN_POINT('',(-56.,27.,0.600000000000001)) ;
#44124 = CARTESIAN_POINT('',(-56.,24.,43.3)) ;
#44125 = CARTESIAN_POINT('',(-56.,-24.,0.600000000000001)) ;
#44126 = CARTESIAN_POINT('',(-56.,-24.,43.3)) ;
#44127 = CARTESIAN_POINT('',(-56.,-30.,0.600000000000001)) ;
#44128 = CARTESIAN_POINT('',(-56.,-27.,0.600000000000001)) ;
#44129 = CARTESIAN_POINT('',(-56.,-30.,25.)) ;
#44130 = CARTESIAN_POINT('',(-56.,-30.,43.3)) ;
#44131 = CARTESIAN_POINT('',(-56.,-30.,86.)) ;
#44132 = CARTESIAN_POINT('',(-56.,-30.,43.3)) ;
#44133 = CARTESIAN_POINT('',(-56.,-4.8,86.)) ;
#44134 = CARTESIAN_POINT('',(-56.,27.,86.)) ;
#44135 = CARTESIAN_POINT('',(-56.,-4.8,82.)) ;
#44136 = CARTESIAN_POINT('',(-56.,-4.8,65.65)) ;
#44137 = CARTESIAN_POINT('',(-56.,11.3,82.)) ;
#44138 = CARTESIAN_POINT('',(-56.,24.,80.)) ;
#44139 = CARTESIAN_POINT('',(-56.,24.,31.)) ;
#44140 = CARTESIAN_POINT('',(-56.,24.,43.3)) ;
#44141 = CARTESIAN_POINT('',(-56.,-24.,80.)) ;
#44142 = CARTESIAN_POINT('',(-56.,0.,80.)) ;
#44143 = CARTESIAN_POINT('',(-56.,-24.,43.3)) ;
#44144 = CARTESIAN_POINT('',(-56.,-20.,27.)) ;
#44145 = CARTESIAN_POINT('',(-56.,-20.,29.)) ;
#44146 = CARTESIAN_POINT('',(-56.,-24.,27.)) ;
#44147 = CARTESIAN_POINT('',(-56.,-22.,27.)) ;
#44148 = CARTESIAN_POINT('',(-56.,-24.,43.3)) ;
#44149 = CARTESIAN_POINT('',(-56.,22.,31.)) ;
#44150 = CARTESIAN_POINT('Origin',(-53.,-30.,43.3)) ;
#44151 = CARTESIAN_POINT('',(-50.,-30.,25.)) ;
#44152 = CARTESIAN_POINT('Origin',(-53.,-30.,25.)) ;
#44153 = CARTESIAN_POINT('',(-50.,-30.,86.)) ;
#44154 = CARTESIAN_POINT('',(-50.,-30.,43.3)) ;
#44155 = CARTESIAN_POINT('',(-53.,-30.,86.)) ;
#44156 = CARTESIAN_POINT('Origin',(-53.,24.,43.3)) ;
#44157 = CARTESIAN_POINT('',(-50.,24.,0.600000000000001)) ;
#44158 = CARTESIAN_POINT('',(-53.,24.,0.600000000000001)) ;
#44159 = CARTESIAN_POINT('',(-50.,24.,43.3)) ;
#44160 = CARTESIAN_POINT('Origin',(-53.,-24.,43.3)) ;
#44161 = CARTESIAN_POINT('',(-50.,-24.,0.600000000000001)) ;
#44162 = CARTESIAN_POINT('',(-50.,-24.,43.3)) ;
#44163 = CARTESIAN_POINT('',(-53.,-24.,0.600000000000001)) ;
#44164 = CARTESIAN_POINT('Origin',(-55.6,27.,43.3)) ;
#44165 = CARTESIAN_POINT('',(-55.6,24.4,0.600000000000001)) ;
#44166 = CARTESIAN_POINT('',(-55.6,24.4,43.3)) ;
#44167 = CARTESIAN_POINT('',(-55.6,29.6,0.600000000000001)) ;
#44168 = CARTESIAN_POINT('',(-55.6,27.,0.600000000000001)) ;
#44169 = CARTESIAN_POINT('',(-55.6,29.6,43.3)) ;
#44170 = CARTESIAN_POINT('Origin',(-53.,29.6,43.3)) ;
#44171 = CARTESIAN_POINT('',(-50.4,29.6,0.600000000000001)) ;
#44172 = CARTESIAN_POINT('',(-53.,29.6,0.600000000000001)) ;
#44173 = CARTESIAN_POINT('',(-50.4,29.6,43.3)) ;
#44174 = CARTESIAN_POINT('Origin',(-55.6,-27.,43.3)) ;
#44175 = CARTESIAN_POINT('',(-55.6,-29.6,0.600000000000001)) ;
#44176 = CARTESIAN_POINT('',(-55.6,-29.6,43.3)) ;
#44177 = CARTESIAN_POINT('',(-55.6,-24.4,0.600000000000001)) ;
#44178 = CARTESIAN_POINT('',(-55.6,-27.,0.600000000000001)) ;
#44179 = CARTESIAN_POINT('',(-55.6,-24.4,43.3)) ;
#44180 = CARTESIAN_POINT('Origin',(-53.,-24.4,43.3)) ;
#44181 = CARTESIAN_POINT('',(-50.4,-24.4,0.600000000000001)) ;
#44182 = CARTESIAN_POINT('',(-53.,-24.4,0.600000000000001)) ;
#44183 = CARTESIAN_POINT('',(-50.4,-24.4,43.3)) ;
#44184 = CARTESIAN_POINT('Origin',(-53.,27.,0.600000000000001)) ;
#44185 = CARTESIAN_POINT('',(-50.,27.,0.600000000000001)) ;
#44186 = CARTESIAN_POINT('',(-50.4,24.4,0.600000000000001)) ;
#44187 = CARTESIAN_POINT('',(-53.,24.4,0.600000000000001)) ;
#44188 = CARTESIAN_POINT('',(-50.4,27.,0.600000000000001)) ;
#44189 = CARTESIAN_POINT('Origin',(-53.,27.,86.)) ;
#44190 = CARTESIAN_POINT('',(-50.,4.8,86.)) ;
#44191 = CARTESIAN_POINT('',(-53.,4.8,86.)) ;
#44192 = CARTESIAN_POINT('',(-50.,27.,86.)) ;
#44193 = CARTESIAN_POINT('Origin',(-53.,30.,43.3)) ;
#44194 = CARTESIAN_POINT('',(-55.6,30.,25.)) ;
#44195 = CARTESIAN_POINT('Origin',(-53.,30.,25.)) ;
#44196 = CARTESIAN_POINT('Origin',(-53.,-30.,43.3)) ;
#44197 = CARTESIAN_POINT('',(-55.6,-30.,25.)) ;
#44198 = CARTESIAN_POINT('Origin',(-53.,-30.,25.)) ;
#44199 = CARTESIAN_POINT('Origin',(-53.,-27.,0.600000000000001)) ;
#44200 = CARTESIAN_POINT('',(-50.,-30.,0.600000000000001)) ;
#44201 = CARTESIAN_POINT('',(-50.,-27.,0.600000000000001)) ;
#44202 = CARTESIAN_POINT('',(-53.,-30.,0.600000000000001)) ;
#44203 = CARTESIAN_POINT('',(-50.4,-29.6,0.600000000000001)) ;
#44204 = CARTESIAN_POINT('',(-53.,-29.6,0.600000000000001)) ;
#44205 = CARTESIAN_POINT('',(-50.4,-27.,0.600000000000001)) ;
#44206 = CARTESIAN_POINT('Origin',(-53.,0.,80.)) ;
#44207 = CARTESIAN_POINT('',(-50.,24.,80.)) ;
#44208 = CARTESIAN_POINT('',(-53.,24.,80.)) ;
#44209 = CARTESIAN_POINT('',(-50.,-24.,80.)) ;
#44210 = CARTESIAN_POINT('',(-50.,0.,80.)) ;
#44211 = CARTESIAN_POINT('',(-53.,-24.,80.)) ;
#44212 = CARTESIAN_POINT('Origin',(-53.,24.,43.3)) ;
#44213 = CARTESIAN_POINT('',(-31.75,24.,31.)) ;
#44214 = CARTESIAN_POINT('',(-50.,24.,43.3)) ;
#44215 = CARTESIAN_POINT('Origin',(-53.,-30.,43.3)) ;
#44216 = CARTESIAN_POINT('',(-50.,-30.,43.3)) ;
#44217 = CARTESIAN_POINT('Origin',(-53.,-30.,25.)) ;
#44218 = CARTESIAN_POINT('Origin',(-53.,24.4,43.3)) ;
#44219 = CARTESIAN_POINT('',(-50.4,24.4,43.3)) ;
#44220 = CARTESIAN_POINT('Origin',(-50.4,27.,43.3)) ;
#44221 = CARTESIAN_POINT('Origin',(-53.,-29.6,43.3)) ;
#44222 = CARTESIAN_POINT('',(-50.4,-29.6,43.3)) ;
#44223 = CARTESIAN_POINT('Origin',(-50.4,-27.,43.3)) ;
#44224 = CARTESIAN_POINT('Origin',(-53.,43.,25.)) ;
#44225 = CARTESIAN_POINT('',(-56.,43.,25.)) ;
#44226 = CARTESIAN_POINT('Origin',(-53.,43.,25.)) ;
#44227 = CARTESIAN_POINT('',(-55.6,43.,25.)) ;
#44228 = CARTESIAN_POINT('Origin',(-53.,43.,25.)) ;
#44229 = CARTESIAN_POINT('Origin',(-53.,-43.,25.)) ;
#44230 = CARTESIAN_POINT('',(-56.,-43.,25.)) ;
#44231 = CARTESIAN_POINT('Origin',(-53.,-43.,25.)) ;
#44232 = CARTESIAN_POINT('',(-55.6,-43.,25.)) ;
#44233 = CARTESIAN_POINT('Origin',(-53.,-43.,25.)) ;
#44234 = CARTESIAN_POINT('Origin',(-53.,0.,25.)) ;
#44235 = CARTESIAN_POINT('',(-56.,0.,25.)) ;
#44236 = CARTESIAN_POINT('Origin',(-53.,0.,25.)) ;
#44237 = CARTESIAN_POINT('',(-56.,0.,25.)) ;
#44238 = CARTESIAN_POINT('Origin',(-53.,0.,25.)) ;
#44239 = CARTESIAN_POINT('',(-55.6,0.,25.)) ;
#44240 = CARTESIAN_POINT('Origin',(-53.,0.,25.)) ;
#44241 = CARTESIAN_POINT('',(-55.6,0.,25.)) ;
#44242 = CARTESIAN_POINT('Origin',(-53.,27.,86.)) ;
#44243 = CARTESIAN_POINT('',(-50.,-4.,86.)) ;
#44244 = CARTESIAN_POINT('',(-53.,-4.,86.)) ;
#44245 = CARTESIAN_POINT('',(-50.,4.,86.)) ;
#44246 = CARTESIAN_POINT('',(-50.,27.,86.)) ;
#44247 = CARTESIAN_POINT('',(-53.,4.,86.)) ;
#44248 = CARTESIAN_POINT('Origin',(-49.,4.4,88.)) ;
#44249 = CARTESIAN_POINT('',(-49.,4.,94.)) ;
#44250 = CARTESIAN_POINT('',(-49.,4.,82.)) ;
#44251 = CARTESIAN_POINT('',(-49.,4.,88.)) ;
#44252 = CARTESIAN_POINT('',(-49.,4.8,82.)) ;
#44253 = CARTESIAN_POINT('',(-49.,4.4,82.)) ;
#44254 = CARTESIAN_POINT('',(-49.,4.8,94.)) ;
#44255 = CARTESIAN_POINT('',(-49.,4.8,88.)) ;
#44256 = CARTESIAN_POINT('',(-49.,4.4,94.)) ;
#44257 = CARTESIAN_POINT('Origin',(-57.,4.4,88.)) ;
#44258 = CARTESIAN_POINT('',(-57.,4.8,94.)) ;
#44259 = CARTESIAN_POINT('',(-57.,4.8,82.)) ;
#44260 = CARTESIAN_POINT('',(-57.,4.8,88.)) ;
#44261 = CARTESIAN_POINT('',(-57.,4.,82.)) ;
#44262 = CARTESIAN_POINT('',(-57.,4.4,82.)) ;
#44263 = CARTESIAN_POINT('',(-57.,4.,94.)) ;
#44264 = CARTESIAN_POINT('',(-57.,4.,88.)) ;
#44265 = CARTESIAN_POINT('',(-57.,4.4,94.)) ;
#44266 = CARTESIAN_POINT('Origin',(-53.,4.4,94.)) ;
#44267 = CARTESIAN_POINT('',(-53.,4.8,94.)) ;
#44268 = CARTESIAN_POINT('',(-53.,4.,94.)) ;
#44269 = CARTESIAN_POINT('Origin',(-53.,4.4,82.)) ;
#44270 = CARTESIAN_POINT('',(-50.,4.8,82.)) ;
#44271 = CARTESIAN_POINT('',(-50.,4.,82.)) ;
#44272 = CARTESIAN_POINT('',(-50.,15.7,82.)) ;
#44273 = CARTESIAN_POINT('',(-53.,4.8,82.)) ;
#44274 = CARTESIAN_POINT('',(-53.,4.,82.)) ;
#44275 = CARTESIAN_POINT('Origin',(-53.,4.4,82.)) ;
#44276 = CARTESIAN_POINT('',(-53.,4.,82.)) ;
#44277 = CARTESIAN_POINT('',(-53.,4.8,82.)) ;
#44278 = CARTESIAN_POINT('Origin',(-53.,4.,88.)) ;
#44279 = CARTESIAN_POINT('',(-50.,4.,65.65)) ;
#44280 = CARTESIAN_POINT('Origin',(-53.,4.8,88.)) ;
#44281 = CARTESIAN_POINT('',(-50.,4.8,65.65)) ;
#44282 = CARTESIAN_POINT('Origin',(-10.5,22.,27.)) ;
#44283 = CARTESIAN_POINT('',(20.4,23.6,27.)) ;
#44284 = CARTESIAN_POINT('',(23.6,23.6,27.)) ;
#44285 = CARTESIAN_POINT('',(5.75,23.6,27.)) ;
#44286 = CARTESIAN_POINT('',(23.6,20.4,27.)) ;
#44287 = CARTESIAN_POINT('',(23.6,22.,27.)) ;
#44288 = CARTESIAN_POINT('',(20.4,20.4,27.)) ;
#44289 = CARTESIAN_POINT('',(5.75,20.4,27.)) ;
#44290 = CARTESIAN_POINT('',(20.4,22.,27.)) ;
#44291 = CARTESIAN_POINT('Origin',(-10.5,22.,27.)) ;
#44292 = CARTESIAN_POINT('',(20.,22.,27.)) ;
#44293 = CARTESIAN_POINT('',(-50.7639320225002,0.,27.)) ;
#44294 = CARTESIAN_POINT('Origin',(24.,22.,13.8)) ;
#44295 = CARTESIAN_POINT('',(24.,22.,0.6)) ;
#44296 = CARTESIAN_POINT('Origin',(20.,22.,13.8)) ;
#44297 = CARTESIAN_POINT('',(20.,22.,0.6)) ;
#44298 = CARTESIAN_POINT('Origin',(22.,22.,0.6)) ;
#44299 = CARTESIAN_POINT('',(20.4,20.4,0.6)) ;
#44300 = CARTESIAN_POINT('',(23.6,20.4,0.6)) ;
#44301 = CARTESIAN_POINT('',(22.,20.4,0.6)) ;
#44302 = CARTESIAN_POINT('',(23.6,23.6,0.6)) ;
#44303 = CARTESIAN_POINT('',(23.6,22.,0.6)) ;
#44304 = CARTESIAN_POINT('',(20.4,23.6,0.6)) ;
#44305 = CARTESIAN_POINT('',(22.,23.6,0.6)) ;
#44306 = CARTESIAN_POINT('',(20.4,22.,0.6)) ;
#44307 = CARTESIAN_POINT('Origin',(20.4,22.,13.8)) ;
#44308 = CARTESIAN_POINT('',(20.4,20.4,13.8)) ;
#44309 = CARTESIAN_POINT('',(20.4,23.6,13.8)) ;
#44310 = CARTESIAN_POINT('Origin',(22.,20.4,13.8)) ;
#44311 = CARTESIAN_POINT('',(23.6,20.4,13.8)) ;
#44312 = CARTESIAN_POINT('Origin',(23.6,22.,13.8)) ;
#44313 = CARTESIAN_POINT('',(23.6,23.6,13.8)) ;
#44314 = CARTESIAN_POINT('Origin',(22.,23.6,13.8)) ;
#44315 = CARTESIAN_POINT('Origin',(-10.5,22.,31.)) ;
#44316 = CARTESIAN_POINT('',(-23.12,21.92,31.)) ;
#44317 = CARTESIAN_POINT('Origin',(-21.92,21.92,31.)) ;
#44318 = CARTESIAN_POINT('Origin',(21.92,21.92,68.)) ;
#44319 = CARTESIAN_POINT('',(20.42,21.92,68.)) ;
#44320 = CARTESIAN_POINT('Origin',(21.92,21.92,68.)) ;
#44321 = CARTESIAN_POINT('',(20.72,21.92,68.)) ;
#44322 = CARTESIAN_POINT('Origin',(21.92,21.92,68.)) ;
#44323 = CARTESIAN_POINT('Origin',(21.92,21.92,49.5)) ;
#44324 = CARTESIAN_POINT('',(20.42,21.92,31.)) ;
#44325 = CARTESIAN_POINT('',(20.42,21.92,49.5)) ;
#44326 = CARTESIAN_POINT('Origin',(21.92,21.92,31.)) ;
#44327 = CARTESIAN_POINT('Origin',(21.92,21.92,49.5)) ;
#44328 = CARTESIAN_POINT('',(20.72,21.92,49.5)) ;
#44329 = CARTESIAN_POINT('Origin',(-10.5,22.,31.)) ;
#44330 = CARTESIAN_POINT('',(-23.42,21.92,31.)) ;
#44331 = CARTESIAN_POINT('Origin',(-21.92,21.92,31.)) ;
#44332 = CARTESIAN_POINT('Origin',(-21.92,21.92,68.)) ;
#44333 = CARTESIAN_POINT('',(-23.42,21.92,68.)) ;
#44334 = CARTESIAN_POINT('Origin',(-21.92,21.92,68.)) ;
#44335 = CARTESIAN_POINT('',(-23.12,21.92,68.)) ;
#44336 = CARTESIAN_POINT('Origin',(-21.92,21.92,68.)) ;
#44337 = CARTESIAN_POINT('Origin',(-21.92,21.92,49.5)) ;
#44338 = CARTESIAN_POINT('',(-23.42,21.92,49.5)) ;
#44339 = CARTESIAN_POINT('Origin',(-21.92,21.92,49.5)) ;
#44340 = CARTESIAN_POINT('',(-23.12,21.92,49.5)) ;
#44341 = CARTESIAN_POINT('Origin',(-53.,0.,25.)) ;
#44342 = CARTESIAN_POINT('',(-55.2360679774998,-24.,27.)) ;
#44343 = CARTESIAN_POINT('',(-55.2360679774998,-20.,27.)) ;
#44344 = CARTESIAN_POINT('',(-55.2360679774998,0.,27.)) ;
#44345 = CARTESIAN_POINT('Origin',(-53.,-20.,25.)) ;
#44346 = CARTESIAN_POINT('Origin',(-53.,-24.,25.)) ;
#44347 = CARTESIAN_POINT('Origin',(-53.,-24.,25.)) ;
#44348 = CARTESIAN_POINT('Origin',(-53.,-24.,43.3)) ;
#44349 = CARTESIAN_POINT('',(-31.75,-24.,27.)) ;
#44350 = CARTESIAN_POINT('Origin',(-53.,-24.,43.3)) ;
#44351 = CARTESIAN_POINT('',(-50.,-24.,43.3)) ;
#44352 = CARTESIAN_POINT('Origin',(-53.,-24.,43.3)) ;
#44353 = CARTESIAN_POINT('',(-50.,-24.,43.3)) ;
#44354 = CARTESIAN_POINT('Origin',(35.,-22.,29.)) ;
#44355 = CARTESIAN_POINT('',(35.,-24.,27.)) ;
#44356 = CARTESIAN_POINT('',(35.,-24.,29.)) ;
#44357 = CARTESIAN_POINT('',(35.,-20.,27.)) ;
#44358 = CARTESIAN_POINT('',(35.,-22.,27.)) ;
#44359 = CARTESIAN_POINT('',(35.,-20.,29.)) ;
#44360 = CARTESIAN_POINT('Origin',(-10.5,-20.,29.)) ;
#44361 = CARTESIAN_POINT('',(-10.5,-20.,27.)) ;
#44362 = CARTESIAN_POINT('',(-10.5,-20.,27.)) ;
#44363 = CARTESIAN_POINT('Origin',(-10.5,-22.,31.)) ;
#44364 = CARTESIAN_POINT('Origin',(-10.5,-22.,27.)) ;
#44365 = CARTESIAN_POINT('Origin',(-10.5,-22.,27.)) ;
#44366 = CARTESIAN_POINT('',(-10.5,-24.,27.)) ;
#44367 = CARTESIAN_POINT('Origin',(-10.5,-24.,29.)) ;
#44368 = CARTESIAN_POINT('',(-50.,-24.,43.3)) ;
#44369 = CARTESIAN_POINT('Origin',(-53.,27.,86.)) ;
#44370 = CARTESIAN_POINT('',(-50.,-4.8,86.)) ;
#44371 = CARTESIAN_POINT('',(-53.,-4.8,86.)) ;
#44372 = CARTESIAN_POINT('',(-50.,27.,86.)) ;
#44373 = CARTESIAN_POINT('Origin',(-50.,27.,43.3)) ;
#44374 = CARTESIAN_POINT('',(-50.,-4.,82.)) ;
#44375 = CARTESIAN_POINT('',(-50.,-4.,65.65)) ;
#44376 = CARTESIAN_POINT('',(-50.,-4.8,82.)) ;
#44377 = CARTESIAN_POINT('',(-50.,11.3,82.)) ;
#44378 = CARTESIAN_POINT('',(-50.,-4.8,65.65)) ;
#44379 = CARTESIAN_POINT('Origin',(-49.,-4.4,88.)) ;
#44380 = CARTESIAN_POINT('',(-49.,-4.8,94.)) ;
#44381 = CARTESIAN_POINT('',(-49.,-4.8,82.)) ;
#44382 = CARTESIAN_POINT('',(-49.,-4.8,88.)) ;
#44383 = CARTESIAN_POINT('',(-49.,-4.,82.)) ;
#44384 = CARTESIAN_POINT('',(-49.,-4.4,82.)) ;
#44385 = CARTESIAN_POINT('',(-49.,-4.,94.)) ;
#44386 = CARTESIAN_POINT('',(-49.,-4.,88.)) ;
#44387 = CARTESIAN_POINT('',(-49.,-4.4,94.)) ;
#44388 = CARTESIAN_POINT('Origin',(-57.,-4.4,88.)) ;
#44389 = CARTESIAN_POINT('',(-57.,-4.,94.)) ;
#44390 = CARTESIAN_POINT('',(-57.,-4.,82.)) ;
#44391 = CARTESIAN_POINT('',(-57.,-4.,88.)) ;
#44392 = CARTESIAN_POINT('',(-57.,-4.8,82.)) ;
#44393 = CARTESIAN_POINT('',(-57.,-4.4,82.)) ;
#44394 = CARTESIAN_POINT('',(-57.,-4.8,94.)) ;
#44395 = CARTESIAN_POINT('',(-57.,-4.8,88.)) ;
#44396 = CARTESIAN_POINT('',(-57.,-4.4,94.)) ;
#44397 = CARTESIAN_POINT('Origin',(-53.,-4.8,88.)) ;
#44398 = CARTESIAN_POINT('',(-53.,-4.8,82.)) ;
#44399 = CARTESIAN_POINT('',(-53.,-4.8,94.)) ;
#44400 = CARTESIAN_POINT('',(-53.,-4.8,82.)) ;
#44401 = CARTESIAN_POINT('Origin',(-53.,-4.4,82.)) ;
#44402 = CARTESIAN_POINT('',(-53.,-4.,82.)) ;
#44403 = CARTESIAN_POINT('Origin',(-53.,-4.4,94.)) ;
#44404 = CARTESIAN_POINT('',(-53.,-4.,94.)) ;
#44405 = CARTESIAN_POINT('Origin',(-53.,-4.,88.)) ;
#44406 = CARTESIAN_POINT('',(-53.,-4.,82.)) ;
#44407 = CARTESIAN_POINT('Origin',(-53.,-4.4,82.)) ;
#44408 = CARTESIAN_POINT('Origin',(-53.,0.,25.)) ;
#44409 = CARTESIAN_POINT('',(-50.4,24.4,26.4966629547096)) ;
#44410 = CARTESIAN_POINT('',(-55.6,24.4,26.4966629547096)) ;
#44411 = CARTESIAN_POINT('Origin',(-53.,24.4,25.)) ;
#44412 = CARTESIAN_POINT('',(-50.4,29.6,26.4966629547096)) ;
#44413 = CARTESIAN_POINT('',(-50.4,0.,26.4966629547096)) ;
#44414 = CARTESIAN_POINT('',(-55.6,29.6,26.4966629547096)) ;
#44415 = CARTESIAN_POINT('Origin',(-53.,29.6,25.)) ;
#44416 = CARTESIAN_POINT('',(-55.6,0.,26.4966629547096)) ;
#44417 = CARTESIAN_POINT('Origin',(-55.6,27.,43.3)) ;
#44418 = CARTESIAN_POINT('',(-55.6,29.6,80.)) ;
#44419 = CARTESIAN_POINT('',(-55.6,29.6,43.3)) ;
#44420 = CARTESIAN_POINT('',(-55.6,24.4,80.)) ;
#44421 = CARTESIAN_POINT('',(-55.6,13.5,80.)) ;
#44422 = CARTESIAN_POINT('',(-55.6,24.4,43.3)) ;
#44423 = CARTESIAN_POINT('Origin',(-53.,29.6,43.3)) ;
#44424 = CARTESIAN_POINT('',(-50.4,29.6,80.)) ;
#44425 = CARTESIAN_POINT('',(-50.4,29.6,43.3)) ;
#44426 = CARTESIAN_POINT('',(-53.,29.6,80.)) ;
#44427 = CARTESIAN_POINT('Origin',(-50.4,27.,43.3)) ;
#44428 = CARTESIAN_POINT('',(-50.4,24.4,80.)) ;
#44429 = CARTESIAN_POINT('',(-50.4,24.4,43.3)) ;
#44430 = CARTESIAN_POINT('',(-50.4,13.5,80.)) ;
#44431 = CARTESIAN_POINT('Origin',(-53.,24.4,43.3)) ;
#44432 = CARTESIAN_POINT('',(-53.,24.4,80.)) ;
#44433 = CARTESIAN_POINT('Origin',(-53.,0.,80.)) ;
#44434 = CARTESIAN_POINT('Origin',(-53.,0.,80.)) ;
#44435 = CARTESIAN_POINT('',(-50.4,-24.4,80.)) ;
#44436 = CARTESIAN_POINT('',(-55.6,-24.4,80.)) ;
#44437 = CARTESIAN_POINT('',(-53.,-24.4,80.)) ;
#44438 = CARTESIAN_POINT('',(-50.4,-29.6,80.)) ;
#44439 = CARTESIAN_POINT('',(-50.4,-13.5,80.)) ;
#44440 = CARTESIAN_POINT('',(-55.6,-29.6,80.)) ;
#44441 = CARTESIAN_POINT('',(-53.,-29.6,80.)) ;
#44442 = CARTESIAN_POINT('',(-55.6,-13.5,80.)) ;
#44443 = CARTESIAN_POINT('Origin',(-53.,-29.6,43.3)) ;
#44444 = CARTESIAN_POINT('',(-50.4,-29.6,26.4966629547096)) ;
#44445 = CARTESIAN_POINT('',(-55.6,-29.6,26.4966629547096)) ;
#44446 = CARTESIAN_POINT('Origin',(-53.,-29.6,25.)) ;
#44447 = CARTESIAN_POINT('',(-55.6,-29.6,43.3)) ;
#44448 = CARTESIAN_POINT('',(-50.4,-29.6,43.3)) ;
#44449 = CARTESIAN_POINT('Origin',(-50.4,-27.,43.3)) ;
#44450 = CARTESIAN_POINT('',(-50.4,-24.4,26.4966629547096)) ;
#44451 = CARTESIAN_POINT('',(-50.4,0.,26.4966629547096)) ;
#44452 = CARTESIAN_POINT('',(-50.4,-24.4,43.3)) ;
#44453 = CARTESIAN_POINT('Origin',(-53.,-24.4,43.3)) ;
#44454 = CARTESIAN_POINT('',(-55.6,-24.4,26.4966629547096)) ;
#44455 = CARTESIAN_POINT('Origin',(-53.,-24.4,25.)) ;
#44456 = CARTESIAN_POINT('',(-55.6,-24.4,43.3)) ;
#44457 = CARTESIAN_POINT('Origin',(-55.6,-27.,43.3)) ;
#44458 = CARTESIAN_POINT('',(-55.6,0.,26.4966629547096)) ;
#44459 = CARTESIAN_POINT('Origin',(-53.,0.,25.)) ;
#44460 = CARTESIAN_POINT('Origin',(-10.5,23.6,29.)) ;
#44461 = CARTESIAN_POINT('',(-54.5329709716756,23.6,27.1)) ;
#44462 = CARTESIAN_POINT('',(-51.4670290283244,23.6,27.1)) ;
#44463 = CARTESIAN_POINT('Origin',(-53.,23.6,25.)) ;
#44464 = CARTESIAN_POINT('',(-10.5,23.6,27.1)) ;
#44465 = CARTESIAN_POINT('Origin',(-10.5,20.4,29.)) ;
#44466 = CARTESIAN_POINT('',(-51.4670290283244,20.4,27.1)) ;
#44467 = CARTESIAN_POINT('',(-54.5329709716756,20.4,27.1)) ;
#44468 = CARTESIAN_POINT('Origin',(-53.,20.4,25.)) ;
#44469 = CARTESIAN_POINT('',(-10.5,20.4,27.1)) ;
#44470 = CARTESIAN_POINT('Origin',(-10.5,22.,27.1)) ;
#44471 = CARTESIAN_POINT('',(-51.4670290283244,0.,27.1)) ;
#44472 = CARTESIAN_POINT('',(-54.5329709716756,0.,27.1)) ;
#44473 = CARTESIAN_POINT('Origin',(-53.,0.,25.)) ;
#44474 = CARTESIAN_POINT('Origin',(-53.,0.,22.4)) ;
#44475 = CARTESIAN_POINT('',(-51.5033370452904,24.,22.4)) ;
#44476 = CARTESIAN_POINT('',(-50.4,24.,22.4)) ;
#44477 = CARTESIAN_POINT('',(-53.,24.,22.4)) ;
#44478 = CARTESIAN_POINT('',(-51.5033370452904,-24.,22.4)) ;
#44479 = CARTESIAN_POINT('',(-51.5033370452904,0.,22.4)) ;
#44480 = CARTESIAN_POINT('',(-50.4,-24.,22.4)) ;
#44481 = CARTESIAN_POINT('',(-53.,-24.,22.4)) ;
#44482 = CARTESIAN_POINT('',(-50.4,0.,22.4)) ;
#44483 = CARTESIAN_POINT('Origin',(-50.4,0.,24.)) ;
#44484 = CARTESIAN_POINT('',(-50.4,24.,23.5033370452904)) ;
#44485 = CARTESIAN_POINT('',(-50.4,24.,33.65)) ;
#44486 = CARTESIAN_POINT('',(-50.4,-24.,23.5033370452904)) ;
#44487 = CARTESIAN_POINT('',(-50.4,-24.,33.65)) ;
#44488 = CARTESIAN_POINT('',(-50.4,0.,23.5033370452904)) ;
#44489 = CARTESIAN_POINT('Origin',(-53.,24.,43.3)) ;
#44490 = CARTESIAN_POINT('Origin',(-53.,24.,25.)) ;
#44491 = CARTESIAN_POINT('Origin',(-53.,-24.,43.3)) ;
#44492 = CARTESIAN_POINT('Origin',(-53.,-24.,25.)) ;
#44493 = CARTESIAN_POINT('Origin',(-53.,0.,25.)) ;
#44494 = CARTESIAN_POINT('Origin',(-53.,29.6,43.3)) ;
#44495 = CARTESIAN_POINT('',(-55.6,29.6,22.4)) ;
#44496 = CARTESIAN_POINT('',(-54.4966629547096,29.6,22.4)) ;
#44497 = CARTESIAN_POINT('',(-53.,29.6,22.4)) ;
#44498 = CARTESIAN_POINT('',(-55.6,29.6,23.5033370452904)) ;
#44499 = CARTESIAN_POINT('Origin',(-53.,29.6,25.)) ;
#44500 = CARTESIAN_POINT('',(-55.6,29.6,43.3)) ;
#44501 = CARTESIAN_POINT('Origin',(-55.6,27.,43.3)) ;
#44502 = CARTESIAN_POINT('',(-55.6,24.4,22.4)) ;
#44503 = CARTESIAN_POINT('',(-55.6,13.5,22.4)) ;
#44504 = CARTESIAN_POINT('',(-55.6,24.4,23.5033370452904)) ;
#44505 = CARTESIAN_POINT('',(-55.6,0.,23.5033370452904)) ;
#44506 = CARTESIAN_POINT('',(-55.6,24.4,43.3)) ;
#44507 = CARTESIAN_POINT('Origin',(-53.,24.4,43.3)) ;
#44508 = CARTESIAN_POINT('',(-54.4966629547096,24.4,22.4)) ;
#44509 = CARTESIAN_POINT('',(-53.,24.4,22.4)) ;
#44510 = CARTESIAN_POINT('Origin',(-53.,24.4,25.)) ;
#44511 = CARTESIAN_POINT('Origin',(-53.,0.,25.)) ;
#44512 = CARTESIAN_POINT('',(-54.4966629547096,0.,22.4)) ;
#44513 = CARTESIAN_POINT('Origin',(-53.,0.,22.4)) ;
#44514 = CARTESIAN_POINT('Origin',(-53.,0.,22.4)) ;
#44515 = CARTESIAN_POINT('',(-55.6,24.,22.4)) ;
#44516 = CARTESIAN_POINT('',(-54.4966629547096,24.,22.4)) ;
#44517 = CARTESIAN_POINT('',(-53.,24.,22.4)) ;
#44518 = CARTESIAN_POINT('',(-55.6,-24.,22.4)) ;
#44519 = CARTESIAN_POINT('',(-55.6,0.,22.4)) ;
#44520 = CARTESIAN_POINT('',(-54.4966629547096,-24.,22.4)) ;
#44521 = CARTESIAN_POINT('',(-53.,-24.,22.4)) ;
#44522 = CARTESIAN_POINT('',(-54.4966629547096,0.,22.4)) ;
#44523 = CARTESIAN_POINT('Origin',(-55.6,0.,24.)) ;
#44524 = CARTESIAN_POINT('',(-55.6,24.,23.5033370452904)) ;
#44525 = CARTESIAN_POINT('',(-55.6,24.,33.65)) ;
#44526 = CARTESIAN_POINT('',(-55.6,-24.,23.5033370452904)) ;
#44527 = CARTESIAN_POINT('',(-55.6,0.,23.5033370452904)) ;
#44528 = CARTESIAN_POINT('',(-55.6,-24.,33.65)) ;
#44529 = CARTESIAN_POINT('Origin',(-53.,24.,43.3)) ;
#44530 = CARTESIAN_POINT('Origin',(-53.,24.,25.)) ;
#44531 = CARTESIAN_POINT('Origin',(-53.,-24.,43.3)) ;
#44532 = CARTESIAN_POINT('Origin',(-53.,-24.,25.)) ;
#44533 = CARTESIAN_POINT('Origin',(-53.,0.,25.)) ;
#44534 = CARTESIAN_POINT('Origin',(-53.,29.6,43.3)) ;
#44535 = CARTESIAN_POINT('',(-51.5033370452904,29.6,22.4)) ;
#44536 = CARTESIAN_POINT('',(-50.4,29.6,22.4)) ;
#44537 = CARTESIAN_POINT('',(-53.,29.6,22.4)) ;
#44538 = CARTESIAN_POINT('',(-50.4,29.6,23.5033370452904)) ;
#44539 = CARTESIAN_POINT('',(-50.4,29.6,43.3)) ;
#44540 = CARTESIAN_POINT('Origin',(-53.,29.6,25.)) ;
#44541 = CARTESIAN_POINT('Origin',(-53.,24.4,43.3)) ;
#44542 = CARTESIAN_POINT('',(-50.4,24.4,22.4)) ;
#44543 = CARTESIAN_POINT('',(-51.5033370452904,24.4,22.4)) ;
#44544 = CARTESIAN_POINT('',(-53.,24.4,22.4)) ;
#44545 = CARTESIAN_POINT('',(-50.4,24.4,23.5033370452904)) ;
#44546 = CARTESIAN_POINT('Origin',(-53.,24.4,25.)) ;
#44547 = CARTESIAN_POINT('',(-50.4,24.4,43.3)) ;
#44548 = CARTESIAN_POINT('Origin',(-53.,0.,25.)) ;
#44549 = CARTESIAN_POINT('',(-51.5033370452904,0.,22.4)) ;
#44550 = CARTESIAN_POINT('',(-50.4,0.,23.5033370452904)) ;
#44551 = CARTESIAN_POINT('Origin',(-50.4,27.,43.3)) ;
#44552 = CARTESIAN_POINT('',(-50.4,13.5,22.4)) ;
#44553 = CARTESIAN_POINT('Origin',(-53.,0.,22.4)) ;
#44554 = CARTESIAN_POINT('Origin',(-53.,0.,22.4)) ;
#44555 = CARTESIAN_POINT('',(-54.4966629547096,-29.6,22.4)) ;
#44556 = CARTESIAN_POINT('',(-55.6,-29.6,22.4)) ;
#44557 = CARTESIAN_POINT('',(-53.,-29.6,22.4)) ;
#44558 = CARTESIAN_POINT('',(-54.4966629547096,-24.4,22.4)) ;
#44559 = CARTESIAN_POINT('',(-54.4966629547096,0.,22.4)) ;
#44560 = CARTESIAN_POINT('',(-55.6,-24.4,22.4)) ;
#44561 = CARTESIAN_POINT('',(-53.,-24.4,22.4)) ;
#44562 = CARTESIAN_POINT('',(-55.6,-13.5,22.4)) ;
#44563 = CARTESIAN_POINT('Origin',(-53.,0.,25.)) ;
#44564 = CARTESIAN_POINT('',(-55.6,-29.6,23.5033370452904)) ;
#44565 = CARTESIAN_POINT('Origin',(-53.,-29.6,25.)) ;
#44566 = CARTESIAN_POINT('',(-55.6,-24.4,23.5033370452904)) ;
#44567 = CARTESIAN_POINT('',(-55.6,0.,23.5033370452904)) ;
#44568 = CARTESIAN_POINT('Origin',(-53.,-24.4,25.)) ;
#44569 = CARTESIAN_POINT('Origin',(-53.,-29.6,43.3)) ;
#44570 = CARTESIAN_POINT('',(-55.6,-29.6,43.3)) ;
#44571 = CARTESIAN_POINT('Origin',(-55.6,-27.,43.3)) ;
#44572 = CARTESIAN_POINT('',(-55.6,-24.4,43.3)) ;
#44573 = CARTESIAN_POINT('Origin',(-53.,-24.4,43.3)) ;
#44574 = CARTESIAN_POINT('Origin',(-53.,-24.4,43.3)) ;
#44575 = CARTESIAN_POINT('',(-51.5033370452904,-24.4,22.4)) ;
#44576 = CARTESIAN_POINT('',(-50.4,-24.4,22.4)) ;
#44577 = CARTESIAN_POINT('',(-53.,-24.4,22.4)) ;
#44578 = CARTESIAN_POINT('',(-50.4,-24.4,23.5033370452904)) ;
#44579 = CARTESIAN_POINT('',(-50.4,-24.4,43.3)) ;
#44580 = CARTESIAN_POINT('Origin',(-53.,-24.4,25.)) ;
#44581 = CARTESIAN_POINT('Origin',(-53.,-29.6,43.3)) ;
#44582 = CARTESIAN_POINT('',(-50.4,-29.6,22.4)) ;
#44583 = CARTESIAN_POINT('',(-51.5033370452904,-29.6,22.4)) ;
#44584 = CARTESIAN_POINT('',(-53.,-29.6,22.4)) ;
#44585 = CARTESIAN_POINT('',(-50.4,-29.6,23.5033370452904)) ;
#44586 = CARTESIAN_POINT('Origin',(-53.,-29.6,25.)) ;
#44587 = CARTESIAN_POINT('',(-50.4,-29.6,43.3)) ;
#44588 = CARTESIAN_POINT('Origin',(-53.,0.,25.)) ;
#44589 = CARTESIAN_POINT('',(-51.5033370452904,0.,22.4)) ;
#44590 = CARTESIAN_POINT('',(-50.4,0.,23.5033370452904)) ;
#44591 = CARTESIAN_POINT('Origin',(-50.4,-27.,43.3)) ;
#44592 = CARTESIAN_POINT('',(-50.4,-13.5,22.4)) ;
#44593 = CARTESIAN_POINT('Origin',(-53.,0.,22.4)) ;
#44594 = CARTESIAN_POINT('Origin',(-53.,0.,25.6)) ;
#44595 = CARTESIAN_POINT('',(-55.5298221281347,29.6,25.6)) ;
#44596 = CARTESIAN_POINT('',(-55.5298221281347,24.4,25.6)) ;
#44597 = CARTESIAN_POINT('',(-55.5298221281347,0.,25.6)) ;
#44598 = CARTESIAN_POINT('',(-50.4701778718653,29.6,25.6)) ;
#44599 = CARTESIAN_POINT('',(-53.,29.6,25.6)) ;
#44600 = CARTESIAN_POINT('',(-50.4701778718653,24.4,25.6)) ;
#44601 = CARTESIAN_POINT('',(-50.4701778718653,0.,25.6)) ;
#44602 = CARTESIAN_POINT('',(-53.,24.4,25.6)) ;
#44603 = CARTESIAN_POINT('Origin',(-53.,24.4,43.3)) ;
#44604 = CARTESIAN_POINT('Origin',(-53.,24.4,25.)) ;
#44605 = CARTESIAN_POINT('Origin',(-53.,29.6,43.3)) ;
#44606 = CARTESIAN_POINT('Origin',(-53.,29.6,25.)) ;
#44607 = CARTESIAN_POINT('Origin',(-53.,0.,25.)) ;
#44608 = CARTESIAN_POINT('Origin',(-53.,0.,25.)) ;
#44609 = CARTESIAN_POINT('',(-50.4701778718653,-29.6,25.6)) ;
#44610 = CARTESIAN_POINT('',(-50.4701778718653,-24.4,25.6)) ;
#44611 = CARTESIAN_POINT('',(-50.4701778718653,0.,25.6)) ;
#44612 = CARTESIAN_POINT('',(-55.5298221281347,-24.4,25.6)) ;
#44613 = CARTESIAN_POINT('Origin',(-53.,-24.4,25.)) ;
#44614 = CARTESIAN_POINT('',(-55.5298221281347,-29.6,25.6)) ;
#44615 = CARTESIAN_POINT('',(-55.5298221281347,0.,25.6)) ;
#44616 = CARTESIAN_POINT('Origin',(-53.,-29.6,25.)) ;
#44617 = CARTESIAN_POINT('Origin',(-53.,-29.6,43.3)) ;
#44618 = CARTESIAN_POINT('',(-53.,-29.6,25.6)) ;
#44619 = CARTESIAN_POINT('Origin',(-53.,-24.4,43.3)) ;
#44620 = CARTESIAN_POINT('',(-53.,-24.4,25.6)) ;
#44621 = CARTESIAN_POINT('Origin',(-53.,0.,25.6)) ;
#44622 = CARTESIAN_POINT('Origin',(-53.,0.,26.)) ;
#44623 = CARTESIAN_POINT('',(-50.6,-29.6,26.)) ;
#44624 = CARTESIAN_POINT('',(-55.4,-29.6,26.)) ;
#44625 = CARTESIAN_POINT('',(-53.,-29.6,26.)) ;
#44626 = CARTESIAN_POINT('',(-50.6,-24.4,26.)) ;
#44627 = CARTESIAN_POINT('',(-50.6,0.,26.)) ;
#44628 = CARTESIAN_POINT('',(-55.4,-24.4,26.)) ;
#44629 = CARTESIAN_POINT('',(-53.,-24.4,26.)) ;
#44630 = CARTESIAN_POINT('',(-55.4,0.,26.)) ;
#44631 = CARTESIAN_POINT('Origin',(-53.,-24.4,43.3)) ;
#44632 = CARTESIAN_POINT('Origin',(-53.,-24.4,25.)) ;
#44633 = CARTESIAN_POINT('Origin',(-53.,-29.6,43.3)) ;
#44634 = CARTESIAN_POINT('Origin',(-53.,-29.6,25.)) ;
#44635 = CARTESIAN_POINT('Origin',(-53.,0.,25.)) ;
#44636 = CARTESIAN_POINT('Origin',(-53.,0.,25.)) ;
#44637 = CARTESIAN_POINT('',(-50.4701778718653,-24.,25.6)) ;
#44638 = CARTESIAN_POINT('',(-50.4701778718653,24.,25.6)) ;
#44639 = CARTESIAN_POINT('',(-50.4701778718653,0.,25.6)) ;
#44640 = CARTESIAN_POINT('',(-55.5298221281347,24.,25.6)) ;
#44641 = CARTESIAN_POINT('Origin',(-53.,24.,25.)) ;
#44642 = CARTESIAN_POINT('',(-55.5298221281347,-24.,25.6)) ;
#44643 = CARTESIAN_POINT('',(-55.5298221281347,0.,25.6)) ;
#44644 = CARTESIAN_POINT('Origin',(-53.,-24.,25.)) ;
#44645 = CARTESIAN_POINT('Origin',(-53.,24.,43.3)) ;
#44646 = CARTESIAN_POINT('',(-53.,24.,25.6)) ;
#44647 = CARTESIAN_POINT('Origin',(-53.,-24.,43.3)) ;
#44648 = CARTESIAN_POINT('',(-53.,-24.,25.6)) ;
#44649 = CARTESIAN_POINT('Origin',(-53.,0.,25.6)) ;
#44650 = CARTESIAN_POINT('Origin',(-53.,0.,26.)) ;
#44651 = CARTESIAN_POINT('',(-55.4,24.4,26.)) ;
#44652 = CARTESIAN_POINT('',(-55.4,29.6,26.)) ;
#44653 = CARTESIAN_POINT('',(-55.4,0.,26.)) ;
#44654 = CARTESIAN_POINT('',(-50.6,24.4,26.)) ;
#44655 = CARTESIAN_POINT('',(-53.,24.4,26.)) ;
#44656 = CARTESIAN_POINT('',(-50.6,29.6,26.)) ;
#44657 = CARTESIAN_POINT('',(-50.6,0.,26.)) ;
#44658 = CARTESIAN_POINT('',(-53.,29.6,26.)) ;
#44659 = CARTESIAN_POINT('Origin',(-53.,24.4,43.3)) ;
#44660 = CARTESIAN_POINT('Origin',(-53.,24.4,25.)) ;
#44661 = CARTESIAN_POINT('Origin',(-53.,0.,25.)) ;
#44662 = CARTESIAN_POINT('Origin',(-53.,29.6,25.)) ;
#44663 = CARTESIAN_POINT('Origin',(-53.,29.6,43.3)) ;
#44664 = CARTESIAN_POINT('Origin',(-53.,29.6,43.3)) ;
#44665 = CARTESIAN_POINT('',(-50.4,29.6,85.6)) ;
#44666 = CARTESIAN_POINT('',(-55.6,29.6,85.6)) ;
#44667 = CARTESIAN_POINT('',(-53.,29.6,85.6)) ;
#44668 = CARTESIAN_POINT('',(-55.6,29.6,80.4)) ;
#44669 = CARTESIAN_POINT('',(-55.6,29.6,43.3)) ;
#44670 = CARTESIAN_POINT('',(-50.4,29.6,80.4)) ;
#44671 = CARTESIAN_POINT('',(-53.,29.6,80.4)) ;
#44672 = CARTESIAN_POINT('',(-50.4,29.6,43.3)) ;
#44673 = CARTESIAN_POINT('Origin',(-55.6,27.,43.3)) ;
#44674 = CARTESIAN_POINT('',(-55.6,24.4,85.6)) ;
#44675 = CARTESIAN_POINT('',(-55.6,13.5,85.6)) ;
#44676 = CARTESIAN_POINT('',(-55.6,24.4,80.4)) ;
#44677 = CARTESIAN_POINT('',(-55.6,24.4,43.3)) ;
#44678 = CARTESIAN_POINT('',(-55.6,13.5,80.4)) ;
#44679 = CARTESIAN_POINT('Origin',(-50.4,27.,43.3)) ;
#44680 = CARTESIAN_POINT('',(-50.4,24.4,85.6)) ;
#44681 = CARTESIAN_POINT('',(-50.4,13.5,85.6)) ;
#44682 = CARTESIAN_POINT('',(-50.4,24.4,80.4)) ;
#44683 = CARTESIAN_POINT('',(-50.4,13.5,80.4)) ;
#44684 = CARTESIAN_POINT('',(-50.4,24.4,43.3)) ;
#44685 = CARTESIAN_POINT('Origin',(-53.,24.4,43.3)) ;
#44686 = CARTESIAN_POINT('',(-53.,24.4,85.6)) ;
#44687 = CARTESIAN_POINT('',(-53.,24.4,80.4)) ;
#44688 = CARTESIAN_POINT('Origin',(-53.,0.,80.4)) ;
#44689 = CARTESIAN_POINT('Origin',(-53.,0.,85.6)) ;
#44690 = CARTESIAN_POINT('Origin',(-53.,0.,85.6)) ;
#44691 = CARTESIAN_POINT('',(-55.6,-29.6,85.6)) ;
#44692 = CARTESIAN_POINT('',(-50.4,-29.6,85.6)) ;
#44693 = CARTESIAN_POINT('',(-53.,-29.6,85.6)) ;
#44694 = CARTESIAN_POINT('',(-55.6,-24.4,85.6)) ;
#44695 = CARTESIAN_POINT('',(-55.6,-13.5,85.6)) ;
#44696 = CARTESIAN_POINT('',(-50.4,-24.4,85.6)) ;
#44697 = CARTESIAN_POINT('',(-53.,-24.4,85.6)) ;
#44698 = CARTESIAN_POINT('',(-50.4,-13.5,85.6)) ;
#44699 = CARTESIAN_POINT('Origin',(-53.,0.,80.4)) ;
#44700 = CARTESIAN_POINT('',(-50.4,-29.6,80.4)) ;
#44701 = CARTESIAN_POINT('',(-55.6,-29.6,80.4)) ;
#44702 = CARTESIAN_POINT('',(-53.,-29.6,80.4)) ;
#44703 = CARTESIAN_POINT('',(-50.4,-24.4,80.4)) ;
#44704 = CARTESIAN_POINT('',(-50.4,-13.5,80.4)) ;
#44705 = CARTESIAN_POINT('',(-55.6,-24.4,80.4)) ;
#44706 = CARTESIAN_POINT('',(-53.,-24.4,80.4)) ;
#44707 = CARTESIAN_POINT('',(-55.6,-13.5,80.4)) ;
#44708 = CARTESIAN_POINT('Origin',(-53.,-29.6,43.3)) ;
#44709 = CARTESIAN_POINT('',(-50.4,-29.6,43.3)) ;
#44710 = CARTESIAN_POINT('',(-55.6,-29.6,43.3)) ;
#44711 = CARTESIAN_POINT('Origin',(-50.4,-27.,43.3)) ;
#44712 = CARTESIAN_POINT('',(-50.4,-24.4,43.3)) ;
#44713 = CARTESIAN_POINT('Origin',(-55.6,-27.,43.3)) ;
#44714 = CARTESIAN_POINT('',(-55.6,-24.4,43.3)) ;
#44715 = CARTESIAN_POINT('Origin',(-53.,-24.4,43.3)) ;
#44716 = CARTESIAN_POINT('Origin',(-53.,-4.8,88.)) ;
#44717 = CARTESIAN_POINT('',(-55.6,-4.8,82.)) ;
#44718 = CARTESIAN_POINT('',(-55.6,-4.8,85.6)) ;
#44719 = CARTESIAN_POINT('',(-55.6,-4.8,85.5)) ;
#44720 = CARTESIAN_POINT('',(-50.4,-4.8,82.)) ;
#44721 = CARTESIAN_POINT('',(-53.,-4.8,82.)) ;
#44722 = CARTESIAN_POINT('',(-50.4,-4.8,85.6)) ;
#44723 = CARTESIAN_POINT('',(-50.4,-4.8,85.5)) ;
#44724 = CARTESIAN_POINT('',(-53.,-4.8,85.6)) ;
#44725 = CARTESIAN_POINT('Origin',(-53.,-4.4,82.)) ;
#44726 = CARTESIAN_POINT('',(-55.6,-4.,82.)) ;
#44727 = CARTESIAN_POINT('',(-55.6,-2.2,82.)) ;
#44728 = CARTESIAN_POINT('',(-50.4,-4.,82.)) ;
#44729 = CARTESIAN_POINT('',(-53.,-4.,82.)) ;
#44730 = CARTESIAN_POINT('',(-50.4,-2.2,82.)) ;
#44731 = CARTESIAN_POINT('Origin',(-53.,-4.,88.)) ;
#44732 = CARTESIAN_POINT('',(-55.6,-4.,85.6)) ;
#44733 = CARTESIAN_POINT('',(-55.6,-4.,85.5)) ;
#44734 = CARTESIAN_POINT('',(-50.4,-4.,85.6)) ;
#44735 = CARTESIAN_POINT('',(-53.,-4.,85.6)) ;
#44736 = CARTESIAN_POINT('',(-50.4,-4.,85.5)) ;
#44737 = CARTESIAN_POINT('Origin',(-50.4,0.,83.)) ;
#44738 = CARTESIAN_POINT('',(-50.4,4.,85.6)) ;
#44739 = CARTESIAN_POINT('',(-50.4,0.,85.6)) ;
#44740 = CARTESIAN_POINT('',(-50.4,4.,82.)) ;
#44741 = CARTESIAN_POINT('',(-50.4,4.,85.5)) ;
#44742 = CARTESIAN_POINT('',(-50.4,4.8,82.)) ;
#44743 = CARTESIAN_POINT('',(-50.4,2.2,82.)) ;
#44744 = CARTESIAN_POINT('',(-50.4,4.8,85.6)) ;
#44745 = CARTESIAN_POINT('',(-50.4,4.8,85.5)) ;
#44746 = CARTESIAN_POINT('',(-50.4,24.,85.6)) ;
#44747 = CARTESIAN_POINT('',(-50.4,0.,85.6)) ;
#44748 = CARTESIAN_POINT('',(-50.4,24.,80.4)) ;
#44749 = CARTESIAN_POINT('',(-50.4,24.,63.15)) ;
#44750 = CARTESIAN_POINT('',(-50.4,-24.,80.4)) ;
#44751 = CARTESIAN_POINT('',(-50.4,0.,80.4)) ;
#44752 = CARTESIAN_POINT('',(-50.4,-24.,85.6)) ;
#44753 = CARTESIAN_POINT('',(-50.4,-24.,63.15)) ;
#44754 = CARTESIAN_POINT('',(-50.4,0.,85.6)) ;
#44755 = CARTESIAN_POINT('Origin',(-53.,0.,85.6)) ;
#44756 = CARTESIAN_POINT('',(-55.6,4.,85.6)) ;
#44757 = CARTESIAN_POINT('',(-55.6,0.,85.6)) ;
#44758 = CARTESIAN_POINT('',(-53.,4.,85.6)) ;
#44759 = CARTESIAN_POINT('Origin',(-53.,0.,85.6)) ;
#44760 = CARTESIAN_POINT('',(-55.6,-24.,85.6)) ;
#44761 = CARTESIAN_POINT('',(-53.,-24.,85.6)) ;
#44762 = CARTESIAN_POINT('',(-55.6,0.,85.6)) ;
#44763 = CARTESIAN_POINT('Origin',(-55.6,0.,83.)) ;
#44764 = CARTESIAN_POINT('',(-55.6,-24.,80.4)) ;
#44765 = CARTESIAN_POINT('',(-55.6,-24.,63.15)) ;
#44766 = CARTESIAN_POINT('',(-55.6,24.,80.4)) ;
#44767 = CARTESIAN_POINT('',(-55.6,0.,80.4)) ;
#44768 = CARTESIAN_POINT('',(-55.6,24.,85.6)) ;
#44769 = CARTESIAN_POINT('',(-55.6,24.,63.15)) ;
#44770 = CARTESIAN_POINT('',(-55.6,4.8,85.6)) ;
#44771 = CARTESIAN_POINT('',(-55.6,0.,85.6)) ;
#44772 = CARTESIAN_POINT('',(-55.6,4.8,82.)) ;
#44773 = CARTESIAN_POINT('',(-55.6,4.8,85.5)) ;
#44774 = CARTESIAN_POINT('',(-55.6,4.,82.)) ;
#44775 = CARTESIAN_POINT('',(-55.6,2.2,82.)) ;
#44776 = CARTESIAN_POINT('',(-55.6,4.,85.5)) ;
#44777 = CARTESIAN_POINT('Origin',(-53.,0.,80.4)) ;
#44778 = CARTESIAN_POINT('',(-53.,24.,80.4)) ;
#44779 = CARTESIAN_POINT('',(-53.,-24.,80.4)) ;
#44780 = CARTESIAN_POINT('Origin',(-53.,-24.,43.3)) ;
#44781 = CARTESIAN_POINT('Origin',(-53.,24.,43.3)) ;
#44782 = CARTESIAN_POINT('',(-53.,24.,85.6)) ;
#44783 = CARTESIAN_POINT('Origin',(-53.,0.,85.6)) ;
#44784 = CARTESIAN_POINT('',(-53.,4.8,85.6)) ;
#44785 = CARTESIAN_POINT('Origin',(-53.,4.8,88.)) ;
#44786 = CARTESIAN_POINT('',(-53.,4.8,82.)) ;
#44787 = CARTESIAN_POINT('Origin',(-53.,4.4,82.)) ;
#44788 = CARTESIAN_POINT('',(-53.,4.,82.)) ;
#44789 = CARTESIAN_POINT('Origin',(-53.,4.,88.)) ;
#44790 = CARTESIAN_POINT('Origin',(-53.,0.,25.)) ;
#44791 = CARTESIAN_POINT('',(-54.5329709716756,-23.6,27.1)) ;
#44792 = CARTESIAN_POINT('',(-54.5329709716756,-20.4,27.1)) ;
#44793 = CARTESIAN_POINT('',(-54.5329709716756,0.,27.1)) ;
#44794 = CARTESIAN_POINT('',(-51.4670290283244,-20.4,27.1)) ;
#44795 = CARTESIAN_POINT('Origin',(-53.,-20.4,25.)) ;
#44796 = CARTESIAN_POINT('',(-51.4670290283244,-23.6,27.1)) ;
#44797 = CARTESIAN_POINT('',(-51.4670290283244,0.,27.1)) ;
#44798 = CARTESIAN_POINT('Origin',(-53.,-23.6,25.)) ;
#44799 = CARTESIAN_POINT('Origin',(-10.5,-22.,27.1)) ;
#44800 = CARTESIAN_POINT('',(-10.5,-20.4,27.1)) ;
#44801 = CARTESIAN_POINT('',(-10.5,-23.6,27.1)) ;
#44802 = CARTESIAN_POINT('Origin',(-10.5,-23.6,29.)) ;
#44803 = CARTESIAN_POINT('Origin',(-10.5,-20.4,29.)) ;
#44804 = CARTESIAN_POINT('Origin',(-10.5,-20.,29.)) ;
#44805 = CARTESIAN_POINT('',(-51.3386752274164,-20.,27.)) ;
#44806 = CARTESIAN_POINT('',(-54.6613247725836,-20.,27.)) ;
#44807 = CARTESIAN_POINT('Origin',(-53.,-20.,25.)) ;
#44808 = CARTESIAN_POINT('',(-10.5,-20.,27.)) ;
#44809 = CARTESIAN_POINT('Origin',(-10.5,-22.,27.)) ;
#44810 = CARTESIAN_POINT('',(-51.3386752274164,-24.,27.)) ;
#44811 = CARTESIAN_POINT('',(-51.3386752274164,0.,27.)) ;
#44812 = CARTESIAN_POINT('',(-54.6613247725836,-24.,27.)) ;
#44813 = CARTESIAN_POINT('',(-31.75,-24.,27.)) ;
#44814 = CARTESIAN_POINT('',(-54.6613247725836,0.,27.)) ;
#44815 = CARTESIAN_POINT('Origin',(-53.,0.,25.)) ;
#44816 = CARTESIAN_POINT('',(-55.4,-24.,26.)) ;
#44817 = CARTESIAN_POINT('Origin',(-53.,-24.,25.)) ;
#44818 = CARTESIAN_POINT('',(-55.4,24.,26.)) ;
#44819 = CARTESIAN_POINT('',(-55.4,0.,26.)) ;
#44820 = CARTESIAN_POINT('',(-54.6613247725836,24.,27.)) ;
#44821 = CARTESIAN_POINT('Origin',(-53.,24.,25.)) ;
#44822 = CARTESIAN_POINT('',(-54.6613247725836,20.,27.)) ;
#44823 = CARTESIAN_POINT('',(-54.6613247725836,0.,27.)) ;
#44824 = CARTESIAN_POINT('',(-51.3386752274164,20.,27.)) ;
#44825 = CARTESIAN_POINT('Origin',(-53.,20.,25.)) ;
#44826 = CARTESIAN_POINT('',(-51.3386752274164,24.,27.)) ;
#44827 = CARTESIAN_POINT('',(-51.3386752274164,0.,27.)) ;
#44828 = CARTESIAN_POINT('',(-50.6,24.,26.)) ;
#44829 = CARTESIAN_POINT('Origin',(-53.,24.,25.)) ;
#44830 = CARTESIAN_POINT('',(-50.6,-24.,26.)) ;
#44831 = CARTESIAN_POINT('',(-50.6,0.,26.)) ;
#44832 = CARTESIAN_POINT('Origin',(-53.,-24.,25.)) ;
#44833 = CARTESIAN_POINT('Origin',(-10.5,20.,29.)) ;
#44834 = CARTESIAN_POINT('',(-10.5,20.,27.)) ;
#44835 = CARTESIAN_POINT('Origin',(-10.5,22.,27.)) ;
#44836 = CARTESIAN_POINT('',(-31.75,24.,27.)) ;
#44837 = CARTESIAN_POINT('Origin',(-53.,24.,43.3)) ;
#44838 = CARTESIAN_POINT('',(-53.,24.,26.)) ;
#44839 = CARTESIAN_POINT('Origin',(-53.,-24.,43.3)) ;
#44840 = CARTESIAN_POINT('',(-53.,-24.,26.)) ;
#44841 = CARTESIAN_POINT('Origin',(-53.,0.,26.)) ;
#44842 = CARTESIAN_POINT('',(0.,0.,0.)) ;
#44843 = CARTESIAN_POINT('Origin',(0.,0.,0.6)) ;
#44844 = CARTESIAN_POINT('',(5.,-5.,0.6)) ;
#44845 = CARTESIAN_POINT('',(5.,5.,0.6)) ;
#44846 = CARTESIAN_POINT('',(5.,0.,0.6)) ;
#44847 = CARTESIAN_POINT('',(-5.,5.,0.6)) ;
#44848 = CARTESIAN_POINT('',(0.,5.,0.6)) ;
#44849 = CARTESIAN_POINT('',(-5.,-5.,0.6)) ;
#44850 = CARTESIAN_POINT('',(-5.,0.,0.6)) ;
#44851 = CARTESIAN_POINT('',(0.,-5.,0.6)) ;
#44852 = CARTESIAN_POINT('Origin',(0.,0.,0.)) ;
#44853 = CARTESIAN_POINT('',(5.,5.,0.)) ;
#44854 = CARTESIAN_POINT('',(5.,-5.,0.)) ;
#44855 = CARTESIAN_POINT('',(5.,0.,0.)) ;
#44856 = CARTESIAN_POINT('',(-5.,-5.,0.)) ;
#44857 = CARTESIAN_POINT('',(0.,-5.,0.)) ;
#44858 = CARTESIAN_POINT('',(-5.,5.,0.)) ;
#44859 = CARTESIAN_POINT('',(-5.,0.,0.)) ;
#44860 = CARTESIAN_POINT('',(0.,5.,0.)) ;
#44861 = CARTESIAN_POINT('Origin',(0.,-5.,0.3)) ;
#44862 = CARTESIAN_POINT('',(-5.,-5.,0.3)) ;
#44863 = CARTESIAN_POINT('',(5.,-5.,0.3)) ;
#44864 = CARTESIAN_POINT('Origin',(-5.,0.,0.3)) ;
#44865 = CARTESIAN_POINT('',(-5.,5.,0.3)) ;
#44866 = CARTESIAN_POINT('Origin',(0.,5.,0.3)) ;
#44867 = CARTESIAN_POINT('',(5.,5.,0.3)) ;
#44868 = CARTESIAN_POINT('Origin',(5.,0.,0.3)) ;
#44869 = CARTESIAN_POINT('',(0.,0.,0.)) ;
#44870 = CARTESIAN_POINT('Origin',(0.,8.5,0.)) ;
#44871 = CARTESIAN_POINT('',(0.35,8.5,-1.3555441711726)) ;
#44872 = CARTESIAN_POINT('',(-0.35,8.5,-1.3555441711726)) ;
#44873 = CARTESIAN_POINT('Ctrl Pts',(0.35,8.5,-1.3555441711726)) ;
#44874 = CARTESIAN_POINT('Ctrl Pts',(0.35,8.54415229373744,-1.3555441711726)) ;
#44875 = CARTESIAN_POINT('Ctrl Pts',(0.341137668931484,8.59111259780368,-1.3579260221299)) ;
#44876 = CARTESIAN_POINT('Ctrl Pts',(0.305362394790648,8.67728573976065,-1.36641567222626)) ;
#44877 = CARTESIAN_POINT('Ctrl Pts',(0.278458987739036,8.71651575909155,-1.37238871180719)) ;
#44878 = CARTESIAN_POINT('Ctrl Pts',(0.216520089475035,8.77845465735555,-1.38351326633711)) ;
#44879 = CARTESIAN_POINT('Ctrl Pts',(0.177288266610716,8.80536144075754,-1.38940376323118)) ;
#44880 = CARTESIAN_POINT('Ctrl Pts',(0.0911087295357738,8.84113917986052,
-1.39770281034285)) ;
#44881 = CARTESIAN_POINT('Ctrl Pts',(0.0441461204601329,8.85,-1.4)) ;
#44882 = CARTESIAN_POINT('Ctrl Pts',(-0.0441461204601329,8.85,-1.4)) ;
#44883 = CARTESIAN_POINT('Ctrl Pts',(-0.0911087295357738,8.84113917986052,
-1.39770281034285)) ;
#44884 = CARTESIAN_POINT('Ctrl Pts',(-0.177288266610716,8.80536144075754,
-1.38940376323118)) ;
#44885 = CARTESIAN_POINT('Ctrl Pts',(-0.216520089475035,8.77845465735555,
-1.38351326633711)) ;
#44886 = CARTESIAN_POINT('Ctrl Pts',(-0.278458987739036,8.71651575909155,
-1.37238871180719)) ;
#44887 = CARTESIAN_POINT('Ctrl Pts',(-0.305362394790648,8.67728573976065,
-1.36641567222626)) ;
#44888 = CARTESIAN_POINT('Ctrl Pts',(-0.341137668931484,8.59111259780368,
-1.3579260221299)) ;
#44889 = CARTESIAN_POINT('Ctrl Pts',(-0.35,8.54415229373744,-1.3555441711726)) ;
#44890 = CARTESIAN_POINT('Ctrl Pts',(-0.35,8.5,-1.3555441711726)) ;
#44891 = CARTESIAN_POINT('Ctrl Pts',(-0.35,8.5,-1.3555441711726)) ;
#44892 = CARTESIAN_POINT('Ctrl Pts',(-0.35,8.45584770626256,-1.3555441711726)) ;
#44893 = CARTESIAN_POINT('Ctrl Pts',(-0.341137668931484,8.40888740219632,
-1.3579260221299)) ;
#44894 = CARTESIAN_POINT('Ctrl Pts',(-0.305362394790648,8.32271426023935,
-1.36641567222626)) ;
#44895 = CARTESIAN_POINT('Ctrl Pts',(-0.278458987739036,8.28348424090845,
-1.37238871180719)) ;
#44896 = CARTESIAN_POINT('Ctrl Pts',(-0.216520089475035,8.22154534264445,
-1.38351326633711)) ;
#44897 = CARTESIAN_POINT('Ctrl Pts',(-0.177288266610716,8.19463855924246,
-1.38940376323118)) ;
#44898 = CARTESIAN_POINT('Ctrl Pts',(-0.0911087295357738,8.15886082013948,
-1.39770281034285)) ;
#44899 = CARTESIAN_POINT('Ctrl Pts',(-0.044146120460133,8.15,-1.4)) ;
#44900 = CARTESIAN_POINT('Ctrl Pts',(0.0441461204601329,8.15,-1.4)) ;
#44901 = CARTESIAN_POINT('Ctrl Pts',(0.0911087295357739,8.15886082013948,
-1.39770281034285)) ;
#44902 = CARTESIAN_POINT('Ctrl Pts',(0.177288266610716,8.19463855924246,-1.38940376323118)) ;
#44903 = CARTESIAN_POINT('Ctrl Pts',(0.216520089475035,8.22154534264445,-1.38351326633711)) ;
#44904 = CARTESIAN_POINT('Ctrl Pts',(0.278458987739037,8.28348424090845,-1.37238871180719)) ;
#44905 = CARTESIAN_POINT('Ctrl Pts',(0.305362394790648,8.32271426023935,-1.36641567222626)) ;
#44906 = CARTESIAN_POINT('Ctrl Pts',(0.341137668931484,8.40888740219632,-1.3579260221299)) ;
#44907 = CARTESIAN_POINT('Ctrl Pts',(0.35,8.45584770626257,-1.3555441711726)) ;
#44908 = CARTESIAN_POINT('Ctrl Pts',(0.35,8.5,-1.3555441711726)) ;
#44909 = CARTESIAN_POINT('',(-0.35,8.5,1.3555441711726)) ;
#44910 = CARTESIAN_POINT('',(-0.35,8.5,0.)) ;
#44911 = CARTESIAN_POINT('',(0.35,8.5,1.3555441711726)) ;
#44912 = CARTESIAN_POINT('Ctrl Pts',(0.35,8.5,1.3555441711726)) ;
#44913 = CARTESIAN_POINT('Ctrl Pts',(0.35,8.45584770626256,1.3555441711726)) ;
#44914 = CARTESIAN_POINT('Ctrl Pts',(0.341137668931484,8.40888740219632,1.3579260221299)) ;
#44915 = CARTESIAN_POINT('Ctrl Pts',(0.305362394790648,8.32271426023935,1.36641567222626)) ;
#44916 = CARTESIAN_POINT('Ctrl Pts',(0.278458987739037,8.28348424090845,1.37238871180719)) ;
#44917 = CARTESIAN_POINT('Ctrl Pts',(0.216520089475035,8.22154534264445,1.38351326633711)) ;
#44918 = CARTESIAN_POINT('Ctrl Pts',(0.177288266610716,8.19463855924246,1.38940376323118)) ;
#44919 = CARTESIAN_POINT('Ctrl Pts',(0.0911087295357738,8.15886082013948,
1.39770281034285)) ;
#44920 = CARTESIAN_POINT('Ctrl Pts',(0.0441461204601329,8.15,1.4)) ;
#44921 = CARTESIAN_POINT('Ctrl Pts',(-0.044146120460133,8.15,1.4)) ;
#44922 = CARTESIAN_POINT('Ctrl Pts',(-0.0911087295357739,8.15886082013948,
1.39770281034285)) ;
#44923 = CARTESIAN_POINT('Ctrl Pts',(-0.177288266610716,8.19463855924246,
1.38940376323118)) ;
#44924 = CARTESIAN_POINT('Ctrl Pts',(-0.216520089475035,8.22154534264445,
1.38351326633711)) ;
#44925 = CARTESIAN_POINT('Ctrl Pts',(-0.278458987739036,8.28348424090845,
1.37238871180719)) ;
#44926 = CARTESIAN_POINT('Ctrl Pts',(-0.305362394790648,8.32271426023935,
1.36641567222626)) ;
#44927 = CARTESIAN_POINT('Ctrl Pts',(-0.341137668931484,8.40888740219632,
1.3579260221299)) ;
#44928 = CARTESIAN_POINT('Ctrl Pts',(-0.35,8.45584770626256,1.3555441711726)) ;
#44929 = CARTESIAN_POINT('Ctrl Pts',(-0.35,8.5,1.3555441711726)) ;
#44930 = CARTESIAN_POINT('Ctrl Pts',(-0.35,8.5,1.3555441711726)) ;
#44931 = CARTESIAN_POINT('Ctrl Pts',(-0.35,8.54415229373744,1.3555441711726)) ;
#44932 = CARTESIAN_POINT('Ctrl Pts',(-0.341137668931484,8.59111259780368,
1.3579260221299)) ;
#44933 = CARTESIAN_POINT('Ctrl Pts',(-0.305362394790648,8.67728573976065,
1.36641567222626)) ;
#44934 = CARTESIAN_POINT('Ctrl Pts',(-0.278458987739036,8.71651575909155,
1.37238871180719)) ;
#44935 = CARTESIAN_POINT('Ctrl Pts',(-0.216520089475035,8.77845465735555,
1.38351326633711)) ;
#44936 = CARTESIAN_POINT('Ctrl Pts',(-0.177288266610716,8.80536144075754,
1.38940376323118)) ;
#44937 = CARTESIAN_POINT('Ctrl Pts',(-0.0911087295357738,8.84113917986052,
1.39770281034285)) ;
#44938 = CARTESIAN_POINT('Ctrl Pts',(-0.0441461204601329,8.85,1.4)) ;
#44939 = CARTESIAN_POINT('Ctrl Pts',(0.0441461204601329,8.85,1.4)) ;
#44940 = CARTESIAN_POINT('Ctrl Pts',(0.0911087295357738,8.84113917986052,
1.39770281034285)) ;
#44941 = CARTESIAN_POINT('Ctrl Pts',(0.177288266610716,8.80536144075754,1.38940376323118)) ;
#44942 = CARTESIAN_POINT('Ctrl Pts',(0.216520089475035,8.77845465735555,1.38351326633711)) ;
#44943 = CARTESIAN_POINT('Ctrl Pts',(0.278458987739036,8.71651575909155,1.37238871180719)) ;
#44944 = CARTESIAN_POINT('Ctrl Pts',(0.305362394790648,8.67728573976065,1.36641567222626)) ;
#44945 = CARTESIAN_POINT('Ctrl Pts',(0.341137668931484,8.59111259780368,1.3579260221299)) ;
#44946 = CARTESIAN_POINT('Ctrl Pts',(0.35,8.54415229373743,1.3555441711726)) ;
#44947 = CARTESIAN_POINT('Ctrl Pts',(0.35,8.5,1.3555441711726)) ;
#44948 = CARTESIAN_POINT('Origin',(0.,0.,0.)) ;
#44949 = CARTESIAN_POINT('',(-2.25,0.,2.75545529808154E-16)) ;
#44950 = CARTESIAN_POINT('Origin',(0.,0.,0.)) ;
#44951 = CARTESIAN_POINT('',(-1.4,0.,1.71450551880629E-16)) ;
#44952 = CARTESIAN_POINT('Origin',(0.,0.,0.)) ;
#44953 = CARTESIAN_POINT('Origin',(0.,-0.3,0.)) ;
#44954 = CARTESIAN_POINT('',(-2.25,-0.6,2.75545529808154E-16)) ;
#44955 = CARTESIAN_POINT('',(-2.25,-0.3,2.75545529808154E-16)) ;
#44956 = CARTESIAN_POINT('Origin',(0.,-0.6,0.)) ;
#44957 = CARTESIAN_POINT('Origin',(0.,-0.6,0.)) ;
#44958 = CARTESIAN_POINT('Origin',(0.,4.75,0.)) ;
#44959 = CARTESIAN_POINT('',(-1.4,9.5,1.71450551880629E-16)) ;
#44960 = CARTESIAN_POINT('Origin',(0.,9.5,0.)) ;
#44961 = CARTESIAN_POINT('',(-1.4,4.75,1.71450551880629E-16)) ;
#44962 = CARTESIAN_POINT('Origin',(0.,9.5,0.)) ;
#44963 = CARTESIAN_POINT('',(0.,0.,0.)) ;
#44964 = CARTESIAN_POINT('Origin',(0.,6.2,0.)) ;
#44965 = CARTESIAN_POINT('',(0.35,6.2,-1.2)) ;
#44966 = CARTESIAN_POINT('',(-0.35,6.2,-1.2)) ;
#44967 = CARTESIAN_POINT('Ctrl Pts',(0.35,6.2,-1.2)) ;
#44968 = CARTESIAN_POINT('Ctrl Pts',(0.35,6.24420771528532,-1.2)) ;
#44969 = CARTESIAN_POINT('Ctrl Pts',(0.341116483481416,6.29118921098472,-1.20269809843758)) ;
#44970 = CARTESIAN_POINT('Ctrl Pts',(0.305327067985986,6.37734520909255,-1.21227824404827)) ;
#44971 = CARTESIAN_POINT('Ctrl Pts',(0.278432902947626,6.41654184388296,-1.21900443594306)) ;
#44972 = CARTESIAN_POINT('Ctrl Pts',(0.216548759315801,6.47842598751478,-1.23150431818794)) ;
#44973 = CARTESIAN_POINT('Ctrl Pts',(0.17734928463595,6.50532552372056,-1.23811350479585)) ;
#44974 = CARTESIAN_POINT('Ctrl Pts',(0.0911830720846971,6.54111888486695,
-1.24742272978092)) ;
#44975 = CARTESIAN_POINT('Ctrl Pts',(0.0441978361366672,6.55,-1.25)) ;
#44976 = CARTESIAN_POINT('Ctrl Pts',(-0.0441978361366672,6.55,-1.25)) ;
#44977 = CARTESIAN_POINT('Ctrl Pts',(-0.0911830720846971,6.54111888486695,
-1.24742272978092)) ;
#44978 = CARTESIAN_POINT('Ctrl Pts',(-0.17734928463595,6.50532552372056,-1.23811350479585)) ;
#44979 = CARTESIAN_POINT('Ctrl Pts',(-0.216548759315801,6.47842598751478,
-1.23150431818794)) ;
#44980 = CARTESIAN_POINT('Ctrl Pts',(-0.278432902947626,6.41654184388296,
-1.21900443594306)) ;
#44981 = CARTESIAN_POINT('Ctrl Pts',(-0.305327067985986,6.37734520909255,
-1.21227824404827)) ;
#44982 = CARTESIAN_POINT('Ctrl Pts',(-0.341116483481416,6.29118921098472,
-1.20269809843758)) ;
#44983 = CARTESIAN_POINT('Ctrl Pts',(-0.35,6.24420771528531,-1.2)) ;
#44984 = CARTESIAN_POINT('Ctrl Pts',(-0.35,6.2,-1.2)) ;
#44985 = CARTESIAN_POINT('Ctrl Pts',(-0.35,6.2,-1.2)) ;
#44986 = CARTESIAN_POINT('Ctrl Pts',(-0.35,6.15579228471469,-1.2)) ;
#44987 = CARTESIAN_POINT('Ctrl Pts',(-0.341116483481416,6.10881078901528,
-1.20269809843758)) ;
#44988 = CARTESIAN_POINT('Ctrl Pts',(-0.305327067985986,6.02265479090746,
-1.21227824404827)) ;
#44989 = CARTESIAN_POINT('Ctrl Pts',(-0.278432902947626,5.98345815611704,
-1.21900443594306)) ;
#44990 = CARTESIAN_POINT('Ctrl Pts',(-0.216548759315801,5.92157401248522,
-1.23150431818794)) ;
#44991 = CARTESIAN_POINT('Ctrl Pts',(-0.17734928463595,5.89467447627944,-1.23811350479585)) ;
#44992 = CARTESIAN_POINT('Ctrl Pts',(-0.0911830720846975,5.85888111513305,
-1.24742272978092)) ;
#44993 = CARTESIAN_POINT('Ctrl Pts',(-0.0441978361366672,5.85,-1.25)) ;
#44994 = CARTESIAN_POINT('Ctrl Pts',(0.0441978361366673,5.85,-1.25)) ;
#44995 = CARTESIAN_POINT('Ctrl Pts',(0.0911830720846976,5.85888111513305,
-1.24742272978092)) ;
#44996 = CARTESIAN_POINT('Ctrl Pts',(0.177349284635951,5.89467447627944,-1.23811350479585)) ;
#44997 = CARTESIAN_POINT('Ctrl Pts',(0.216548759315801,5.92157401248522,-1.23150431818794)) ;
#44998 = CARTESIAN_POINT('Ctrl Pts',(0.278432902947626,5.98345815611704,-1.21900443594306)) ;
#44999 = CARTESIAN_POINT('Ctrl Pts',(0.305327067985986,6.02265479090746,-1.21227824404827)) ;
#45000 = CARTESIAN_POINT('Ctrl Pts',(0.341116483481416,6.10881078901528,-1.20269809843758)) ;
#45001 = CARTESIAN_POINT('Ctrl Pts',(0.35,6.15579228471469,-1.2)) ;
#45002 = CARTESIAN_POINT('Ctrl Pts',(0.35,6.2,-1.2)) ;
#45003 = CARTESIAN_POINT('',(-0.35,6.2,1.2)) ;
#45004 = CARTESIAN_POINT('',(-0.35,6.2,0.)) ;
#45005 = CARTESIAN_POINT('',(0.35,6.2,1.2)) ;
#45006 = CARTESIAN_POINT('Ctrl Pts',(0.35,6.2,1.2)) ;
#45007 = CARTESIAN_POINT('Ctrl Pts',(0.35,6.15579228471469,1.2)) ;
#45008 = CARTESIAN_POINT('Ctrl Pts',(0.341116483481416,6.10881078901528,1.20269809843758)) ;
#45009 = CARTESIAN_POINT('Ctrl Pts',(0.305327067985986,6.02265479090746,1.21227824404827)) ;
#45010 = CARTESIAN_POINT('Ctrl Pts',(0.278432902947626,5.98345815611704,1.21900443594306)) ;
#45011 = CARTESIAN_POINT('Ctrl Pts',(0.216548759315801,5.92157401248522,1.23150431818794)) ;
#45012 = CARTESIAN_POINT('Ctrl Pts',(0.177349284635951,5.89467447627944,1.23811350479585)) ;
#45013 = CARTESIAN_POINT('Ctrl Pts',(0.0911830720846975,5.85888111513305,
1.24742272978092)) ;
#45014 = CARTESIAN_POINT('Ctrl Pts',(0.0441978361366673,5.85,1.25)) ;
#45015 = CARTESIAN_POINT('Ctrl Pts',(-0.0441978361366672,5.85,1.25)) ;
#45016 = CARTESIAN_POINT('Ctrl Pts',(-0.0911830720846974,5.85888111513305,
1.24742272978092)) ;
#45017 = CARTESIAN_POINT('Ctrl Pts',(-0.17734928463595,5.89467447627944,1.23811350479585)) ;
#45018 = CARTESIAN_POINT('Ctrl Pts',(-0.216548759315801,5.92157401248522,
1.23150431818794)) ;
#45019 = CARTESIAN_POINT('Ctrl Pts',(-0.278432902947626,5.98345815611704,
1.21900443594306)) ;
#45020 = CARTESIAN_POINT('Ctrl Pts',(-0.305327067985986,6.02265479090746,
1.21227824404827)) ;
#45021 = CARTESIAN_POINT('Ctrl Pts',(-0.341116483481416,6.10881078901528,
1.20269809843758)) ;
#45022 = CARTESIAN_POINT('Ctrl Pts',(-0.35,6.15579228471469,1.2)) ;
#45023 = CARTESIAN_POINT('Ctrl Pts',(-0.35,6.2,1.2)) ;
#45024 = CARTESIAN_POINT('Ctrl Pts',(-0.35,6.2,1.2)) ;
#45025 = CARTESIAN_POINT('Ctrl Pts',(-0.35,6.24420771528531,1.2)) ;
#45026 = CARTESIAN_POINT('Ctrl Pts',(-0.341116483481416,6.29118921098472,
1.20269809843758)) ;
#45027 = CARTESIAN_POINT('Ctrl Pts',(-0.305327067985986,6.37734520909255,
1.21227824404827)) ;
#45028 = CARTESIAN_POINT('Ctrl Pts',(-0.278432902947626,6.41654184388296,
1.21900443594306)) ;
#45029 = CARTESIAN_POINT('Ctrl Pts',(-0.216548759315801,6.47842598751478,
1.23150431818794)) ;
#45030 = CARTESIAN_POINT('Ctrl Pts',(-0.177349284635951,6.50532552372056,
1.23811350479585)) ;
#45031 = CARTESIAN_POINT('Ctrl Pts',(-0.0911830720846972,6.54111888486695,
1.24742272978092)) ;
#45032 = CARTESIAN_POINT('Ctrl Pts',(-0.0441978361366672,6.55,1.25)) ;
#45033 = CARTESIAN_POINT('Ctrl Pts',(0.0441978361366672,6.55,1.25)) ;
#45034 = CARTESIAN_POINT('Ctrl Pts',(0.091183072084697,6.54111888486695,1.24742272978092)) ;
#45035 = CARTESIAN_POINT('Ctrl Pts',(0.17734928463595,6.50532552372056,1.23811350479585)) ;
#45036 = CARTESIAN_POINT('Ctrl Pts',(0.216548759315801,6.47842598751478,1.23150431818794)) ;
#45037 = CARTESIAN_POINT('Ctrl Pts',(0.278432902947626,6.41654184388296,1.21900443594306)) ;
#45038 = CARTESIAN_POINT('Ctrl Pts',(0.305327067985986,6.37734520909255,1.21227824404827)) ;
#45039 = CARTESIAN_POINT('Ctrl Pts',(0.341116483481416,6.29118921098472,1.20269809843758)) ;
#45040 = CARTESIAN_POINT('Ctrl Pts',(0.35,6.24420771528531,1.2)) ;
#45041 = CARTESIAN_POINT('Ctrl Pts',(0.35,6.2,1.2)) ;
#45042 = CARTESIAN_POINT('Origin',(0.,-7.,0.)) ;
#45043 = CARTESIAN_POINT('',(-2.,-7.,2.44929359829471E-16)) ;
#45044 = CARTESIAN_POINT('Origin',(0.,-7.,0.)) ;
#45045 = CARTESIAN_POINT('',(-1.25,-7.,1.53080849893419E-16)) ;
#45046 = CARTESIAN_POINT('Origin',(0.,-7.,0.)) ;
#45047 = CARTESIAN_POINT('Origin',(0.,-7.3,0.)) ;
#45048 = CARTESIAN_POINT('',(-2.,-7.6,2.44929359829471E-16)) ;
#45049 = CARTESIAN_POINT('',(-2.,-7.3,2.44929359829471E-16)) ;
#45050 = CARTESIAN_POINT('Origin',(0.,-7.6,0.)) ;
#45051 = CARTESIAN_POINT('Origin',(0.,-7.6,0.)) ;
#45052 = CARTESIAN_POINT('Origin',(0.,0.,0.)) ;
#45053 = CARTESIAN_POINT('',(-1.25,7.,1.53080849893419E-16)) ;
#45054 = CARTESIAN_POINT('Origin',(0.,7.,0.)) ;
#45055 = CARTESIAN_POINT('',(-1.25,0.,1.53080849893419E-16)) ;
#45056 = CARTESIAN_POINT('Origin',(0.,7.,0.)) ;
#45057 = CARTESIAN_POINT('',(0.,0.,0.)) ;
#45058 = CARTESIAN_POINT('',(-53.,27.,0.)) ;
#45059 = CARTESIAN_POINT('',(-53.,-27.,0.)) ;
#45060 = CARTESIAN_POINT('',(22.,22.,0.)) ;
#45061 = CARTESIAN_POINT('',(22.,-22.,0.)) ;
#45062 = CARTESIAN_POINT('',(-53.,43.,25.)) ;
#45063 = CARTESIAN_POINT('',(-53.,-43.,25.)) ;
#45064 = CARTESIAN_POINT('',(-53.,0.,90.)) ;
#45065 = CARTESIAN_POINT('',(0.,0.,0.)) ;
#45066 = CARTESIAN_POINT('',(0.,0.,0.)) ;
#45067 = CARTESIAN_POINT('Origin',(-8.5,-22.,31.5)) ;
#45068 = CARTESIAN_POINT('',(-9.15,-22.,31.)) ;
#45069 = CARTESIAN_POINT('Origin',(-8.5,-22.,31.)) ;
#45070 = CARTESIAN_POINT('',(-9.15,-22.,32.)) ;
#45071 = CARTESIAN_POINT('',(-9.15,-22.,31.5)) ;
#45072 = CARTESIAN_POINT('Origin',(-8.5,-22.,32.)) ;
#45073 = CARTESIAN_POINT('Origin',(-8.5,22.,31.5)) ;
#45074 = CARTESIAN_POINT('',(-9.15,22.,31.)) ;
#45075 = CARTESIAN_POINT('Origin',(-8.5,22.,31.)) ;
#45076 = CARTESIAN_POINT('',(-9.15,22.,32.)) ;
#45077 = CARTESIAN_POINT('',(-9.15,22.,31.5)) ;
#45078 = CARTESIAN_POINT('Origin',(-8.5,22.,32.)) ;
#45079 = CARTESIAN_POINT('Origin',(8.5,-22.,31.5)) ;
#45080 = CARTESIAN_POINT('',(7.85,-22.,31.)) ;
#45081 = CARTESIAN_POINT('Origin',(8.5,-22.,31.)) ;
#45082 = CARTESIAN_POINT('',(7.85,-22.,32.)) ;
#45083 = CARTESIAN_POINT('',(7.85,-22.,31.5)) ;
#45084 = CARTESIAN_POINT('Origin',(8.5,-22.,32.)) ;
#45085 = CARTESIAN_POINT('Origin',(8.5,22.,31.5)) ;
#45086 = CARTESIAN_POINT('',(7.85,22.,31.)) ;
#45087 = CARTESIAN_POINT('Origin',(8.5,22.,31.)) ;
#45088 = CARTESIAN_POINT('',(7.85,22.,32.)) ;
#45089 = CARTESIAN_POINT('',(7.85,22.,31.5)) ;
#45090 = CARTESIAN_POINT('Origin',(8.5,22.,32.)) ;
#45091 = CARTESIAN_POINT('Origin',(-11.,-10.,41.05)) ;
#45092 = CARTESIAN_POINT('',(-11.,-9.575,40.)) ;
#45093 = CARTESIAN_POINT('',(-11.,-9.575,42.)) ;
#45094 = CARTESIAN_POINT('',(-11.,-9.575,41.05)) ;
#45095 = CARTESIAN_POINT('',(-11.,-10.425,40.)) ;
#45096 = CARTESIAN_POINT('Origin',(-11.,-10.,40.)) ;
#45097 = CARTESIAN_POINT('',(-11.,-10.425,42.)) ;
#45098 = CARTESIAN_POINT('',(-11.,-10.425,41.05)) ;
#45099 = CARTESIAN_POINT('Origin',(-11.,-10.,42.)) ;
#45100 = CARTESIAN_POINT('Origin',(-11.,-10.,40.)) ;
#45101 = CARTESIAN_POINT('',(-11.,-5.,40.)) ;
#45102 = CARTESIAN_POINT('Origin',(0.,0.,42.)) ;
#45103 = CARTESIAN_POINT('',(-11.,-11.,42.)) ;
#45104 = CARTESIAN_POINT('',(-11.,0.,42.)) ;
#45105 = CARTESIAN_POINT('',(0.,-11.,42.)) ;
#45106 = CARTESIAN_POINT('',(0.,-11.,42.)) ;
#45107 = CARTESIAN_POINT('',(-2.5,-8.5,42.)) ;
#45108 = CARTESIAN_POINT('Origin',(0.,-8.5,42.)) ;
#45109 = CARTESIAN_POINT('',(-1.79965394597392,-6.76470588235294,42.)) ;
#45110 = CARTESIAN_POINT('Origin',(0.,-8.5,42.)) ;
#45111 = CARTESIAN_POINT('',(-7.,-8.57252759403147E-16,42.)) ;
#45112 = CARTESIAN_POINT('Origin',(0.,0.,42.)) ;
#45113 = CARTESIAN_POINT('',(1.79965394597392,-6.76470588235294,42.)) ;
#45114 = CARTESIAN_POINT('Origin',(0.,0.,42.)) ;
#45115 = CARTESIAN_POINT('Origin',(0.,-8.5,42.)) ;
#45116 = CARTESIAN_POINT('',(11.,-11.,42.)) ;
#45117 = CARTESIAN_POINT('',(0.,-11.,42.)) ;
#45118 = CARTESIAN_POINT('',(11.,-10.425,42.)) ;
#45119 = CARTESIAN_POINT('',(11.,0.,42.)) ;
#45120 = CARTESIAN_POINT('',(11.,-9.575,42.)) ;
#45121 = CARTESIAN_POINT('Origin',(11.,-10.,42.)) ;
#45122 = CARTESIAN_POINT('',(11.,9.575,42.)) ;
#45123 = CARTESIAN_POINT('',(11.,0.,42.)) ;
#45124 = CARTESIAN_POINT('',(11.,10.425,42.)) ;
#45125 = CARTESIAN_POINT('Origin',(11.,10.,42.)) ;
#45126 = CARTESIAN_POINT('',(11.,11.,42.)) ;
#45127 = CARTESIAN_POINT('',(11.,0.,42.)) ;
#45128 = CARTESIAN_POINT('',(-11.,11.,42.)) ;
#45129 = CARTESIAN_POINT('',(0.,11.,42.)) ;
#45130 = CARTESIAN_POINT('',(-11.,10.425,42.)) ;
#45131 = CARTESIAN_POINT('',(-11.,0.,42.)) ;
#45132 = CARTESIAN_POINT('',(-11.,9.575,42.)) ;
#45133 = CARTESIAN_POINT('Origin',(-11.,10.,42.)) ;
#45134 = CARTESIAN_POINT('',(-11.,0.,42.)) ;
#45135 = CARTESIAN_POINT('Origin',(-11.,10.,40.)) ;
#45136 = CARTESIAN_POINT('',(-11.,9.575,40.)) ;
#45137 = CARTESIAN_POINT('',(-11.,10.425,40.)) ;
#45138 = CARTESIAN_POINT('',(-11.,5.,40.)) ;
#45139 = CARTESIAN_POINT('Origin',(-11.,10.,40.)) ;
#45140 = CARTESIAN_POINT('Origin',(-11.,10.,41.05)) ;
#45141 = CARTESIAN_POINT('',(-11.,9.575,41.05)) ;
#45142 = CARTESIAN_POINT('',(-11.,10.425,41.05)) ;
#45143 = CARTESIAN_POINT('Origin',(-11.,0.,34.)) ;
#45144 = CARTESIAN_POINT('',(-11.,11.,32.)) ;
#45145 = CARTESIAN_POINT('',(-11.,11.,34.)) ;
#45146 = CARTESIAN_POINT('',(-11.,25.,32.)) ;
#45147 = CARTESIAN_POINT('',(-11.,18.,32.)) ;
#45148 = CARTESIAN_POINT('',(-11.,25.,31.)) ;
#45149 = CARTESIAN_POINT('',(-11.,25.,31.5)) ;
#45150 = CARTESIAN_POINT('',(-11.,11.,31.)) ;
#45151 = CARTESIAN_POINT('',(-11.,18.,31.)) ;
#45152 = CARTESIAN_POINT('',(-11.,11.,26.)) ;
#45153 = CARTESIAN_POINT('',(-11.,11.,34.)) ;
#45154 = CARTESIAN_POINT('',(-11.,-11.,26.)) ;
#45155 = CARTESIAN_POINT('',(-11.,0.,26.)) ;
#45156 = CARTESIAN_POINT('',(-11.,-11.,31.)) ;
#45157 = CARTESIAN_POINT('',(-11.,-11.,34.)) ;
#45158 = CARTESIAN_POINT('',(-11.,-25.,31.)) ;
#45159 = CARTESIAN_POINT('',(-11.,-18.,31.)) ;
#45160 = CARTESIAN_POINT('',(-11.,-25.,32.)) ;
#45161 = CARTESIAN_POINT('',(-11.,-25.,31.5)) ;
#45162 = CARTESIAN_POINT('',(-11.,-11.,32.)) ;
#45163 = CARTESIAN_POINT('',(-11.,-18.,32.)) ;
#45164 = CARTESIAN_POINT('',(-11.,-11.,34.)) ;
#45165 = CARTESIAN_POINT('',(-11.,-4.28626379701574E-16,37.5)) ;
#45166 = CARTESIAN_POINT('Origin',(-11.,0.,34.)) ;
#45167 = CARTESIAN_POINT('Origin',(11.,-10.,40.)) ;
#45168 = CARTESIAN_POINT('',(11.,-9.575,40.)) ;
#45169 = CARTESIAN_POINT('',(11.,-10.425,40.)) ;
#45170 = CARTESIAN_POINT('',(11.,-5.,40.)) ;
#45171 = CARTESIAN_POINT('Origin',(11.,-10.,40.)) ;
#45172 = CARTESIAN_POINT('Origin',(11.,-10.,41.05)) ;
#45173 = CARTESIAN_POINT('',(11.,-9.575,41.05)) ;
#45174 = CARTESIAN_POINT('',(11.,-10.425,41.05)) ;
#45175 = CARTESIAN_POINT('Origin',(11.,0.,34.)) ;
#45176 = CARTESIAN_POINT('',(11.,-11.,32.)) ;
#45177 = CARTESIAN_POINT('',(11.,-11.,34.)) ;
#45178 = CARTESIAN_POINT('',(11.,-25.,32.)) ;
#45179 = CARTESIAN_POINT('',(11.,-18.,32.)) ;
#45180 = CARTESIAN_POINT('',(11.,-25.,31.)) ;
#45181 = CARTESIAN_POINT('',(11.,-25.,31.5)) ;
#45182 = CARTESIAN_POINT('',(11.,-11.,31.)) ;
#45183 = CARTESIAN_POINT('',(11.,-18.,31.)) ;
#45184 = CARTESIAN_POINT('',(11.,-11.,26.)) ;
#45185 = CARTESIAN_POINT('',(11.,-11.,34.)) ;
#45186 = CARTESIAN_POINT('',(11.,11.,26.)) ;
#45187 = CARTESIAN_POINT('',(11.,0.,26.)) ;
#45188 = CARTESIAN_POINT('',(11.,11.,31.)) ;
#45189 = CARTESIAN_POINT('',(11.,11.,34.)) ;
#45190 = CARTESIAN_POINT('',(11.,25.,31.)) ;
#45191 = CARTESIAN_POINT('',(11.,18.,31.)) ;
#45192 = CARTESIAN_POINT('',(11.,25.,32.)) ;
#45193 = CARTESIAN_POINT('',(11.,25.,31.5)) ;
#45194 = CARTESIAN_POINT('',(11.,11.,32.)) ;
#45195 = CARTESIAN_POINT('',(11.,18.,32.)) ;
#45196 = CARTESIAN_POINT('',(11.,11.,34.)) ;
#45197 = CARTESIAN_POINT('',(11.,10.425,40.)) ;
#45198 = CARTESIAN_POINT('',(11.,10.425,41.05)) ;
#45199 = CARTESIAN_POINT('',(11.,9.575,40.)) ;
#45200 = CARTESIAN_POINT('',(11.,5.,40.)) ;
#45201 = CARTESIAN_POINT('',(11.,9.575,41.05)) ;
#45202 = CARTESIAN_POINT('',(11.,7.,39.)) ;
#45203 = CARTESIAN_POINT('Origin',(11.,7.,38.)) ;
#45204 = CARTESIAN_POINT('Origin',(11.,10.,40.)) ;
#45205 = CARTESIAN_POINT('Origin',(11.,10.,40.)) ;
#45206 = CARTESIAN_POINT('Origin',(11.,10.,41.05)) ;
#45207 = CARTESIAN_POINT('Origin',(10.95,7.,38.)) ;
#45208 = CARTESIAN_POINT('',(10.,7.,38.5)) ;
#45209 = CARTESIAN_POINT('Origin',(10.,7.,38.)) ;
#45210 = CARTESIAN_POINT('',(11.8,7.,38.5)) ;
#45211 = CARTESIAN_POINT('',(10.95,7.,38.5)) ;
#45212 = CARTESIAN_POINT('Origin',(11.8,7.,38.)) ;
#45213 = CARTESIAN_POINT('Origin',(10.,7.,38.)) ;
#45214 = CARTESIAN_POINT('Origin',(11.4,7.,38.)) ;
#45215 = CARTESIAN_POINT('',(11.8,7.,39.)) ;
#45216 = CARTESIAN_POINT('Origin',(11.8,7.,38.)) ;
#45217 = CARTESIAN_POINT('',(11.4,7.,39.)) ;
#45218 = CARTESIAN_POINT('Origin',(11.8,7.,38.)) ;
#45219 = CARTESIAN_POINT('Origin',(0.,0.,24.)) ;
#45220 = CARTESIAN_POINT('',(9.5,-0.200997512422418,23.)) ;
#45221 = CARTESIAN_POINT('',(10.5,-0.200997512422418,23.)) ;
#45222 = CARTESIAN_POINT('',(0.,-0.200997512422418,23.)) ;
#45223 = CARTESIAN_POINT('',(9.5,0.200997512422418,23.)) ;
#45224 = CARTESIAN_POINT('Origin',(9.5,0.,24.)) ;
#45225 = CARTESIAN_POINT('',(10.5,0.200997512422418,23.)) ;
#45226 = CARTESIAN_POINT('',(0.,0.200997512422418,23.)) ;
#45227 = CARTESIAN_POINT('Origin',(10.5,0.,24.)) ;
#45228 = CARTESIAN_POINT('Origin',(0.,0.,24.)) ;
#45229 = CARTESIAN_POINT('',(-10.5,-0.200997512422418,23.)) ;
#45230 = CARTESIAN_POINT('',(-9.5,-0.200997512422418,23.)) ;
#45231 = CARTESIAN_POINT('',(0.,-0.200997512422418,23.)) ;
#45232 = CARTESIAN_POINT('',(-10.5,0.200997512422418,23.)) ;
#45233 = CARTESIAN_POINT('Origin',(-10.5,0.,24.)) ;
#45234 = CARTESIAN_POINT('',(-9.5,0.200997512422418,23.)) ;
#45235 = CARTESIAN_POINT('',(0.,0.200997512422418,23.)) ;
#45236 = CARTESIAN_POINT('Origin',(-9.5,0.,24.)) ;
#45237 = CARTESIAN_POINT('Origin',(-10.5,0.,24.5)) ;
#45238 = CARTESIAN_POINT('',(-10.5,-2.,23.)) ;
#45239 = CARTESIAN_POINT('',(-10.5,0.,23.)) ;
#45240 = CARTESIAN_POINT('',(-10.5,-2.,26.)) ;
#45241 = CARTESIAN_POINT('',(-10.5,-2.,24.5)) ;
#45242 = CARTESIAN_POINT('',(-10.5,2.,26.)) ;
#45243 = CARTESIAN_POINT('',(-10.5,0.,26.)) ;
#45244 = CARTESIAN_POINT('',(-10.5,2.,23.)) ;
#45245 = CARTESIAN_POINT('',(-10.5,2.,24.5)) ;
#45246 = CARTESIAN_POINT('',(-10.5,0.,23.)) ;
#45247 = CARTESIAN_POINT('Origin',(-10.,0.,23.)) ;
#45248 = CARTESIAN_POINT('',(-9.5,-2.,23.)) ;
#45249 = CARTESIAN_POINT('',(-9.5,0.,23.)) ;
#45250 = CARTESIAN_POINT('',(-10.,-2.,23.)) ;
#45251 = CARTESIAN_POINT('Origin',(-10.,0.,23.)) ;
#45252 = CARTESIAN_POINT('',(-9.5,2.,23.)) ;
#45253 = CARTESIAN_POINT('',(-10.,2.,23.)) ;
#45254 = CARTESIAN_POINT('',(-9.5,0.,23.)) ;
#45255 = CARTESIAN_POINT('Origin',(9.5,0.,24.5)) ;
#45256 = CARTESIAN_POINT('',(9.5,-2.,23.)) ;
#45257 = CARTESIAN_POINT('',(9.5,0.,23.)) ;
#45258 = CARTESIAN_POINT('',(9.5,-2.,26.)) ;
#45259 = CARTESIAN_POINT('',(9.5,-2.,24.5)) ;
#45260 = CARTESIAN_POINT('',(9.5,2.,26.)) ;
#45261 = CARTESIAN_POINT('',(9.5,0.,26.)) ;
#45262 = CARTESIAN_POINT('',(9.5,2.,23.)) ;
#45263 = CARTESIAN_POINT('',(9.5,2.,24.5)) ;
#45264 = CARTESIAN_POINT('',(9.5,0.,23.)) ;
#45265 = CARTESIAN_POINT('Origin',(10.,0.,23.)) ;
#45266 = CARTESIAN_POINT('',(10.5,-2.,23.)) ;
#45267 = CARTESIAN_POINT('',(10.5,0.,23.)) ;
#45268 = CARTESIAN_POINT('',(10.,-2.,23.)) ;
#45269 = CARTESIAN_POINT('Origin',(10.,0.,23.)) ;
#45270 = CARTESIAN_POINT('',(10.5,2.,23.)) ;
#45271 = CARTESIAN_POINT('',(10.,2.,23.)) ;
#45272 = CARTESIAN_POINT('',(10.5,0.,23.)) ;
#45273 = CARTESIAN_POINT('Origin',(-10.,-2.,24.5)) ;
#45274 = CARTESIAN_POINT('',(-9.5,-2.,26.)) ;
#45275 = CARTESIAN_POINT('',(-9.5,-2.,24.5)) ;
#45276 = CARTESIAN_POINT('',(-5.,-2.,26.)) ;
#45277 = CARTESIAN_POINT('Origin',(-10.,2.,24.5)) ;
#45278 = CARTESIAN_POINT('',(-9.5,2.,26.)) ;
#45279 = CARTESIAN_POINT('',(-9.5,2.,24.5)) ;
#45280 = CARTESIAN_POINT('',(-5.,2.,26.)) ;
#45281 = CARTESIAN_POINT('Origin',(-9.5,0.,24.5)) ;
#45282 = CARTESIAN_POINT('',(-9.5,0.,26.)) ;
#45283 = CARTESIAN_POINT('Origin',(10.,-2.,24.5)) ;
#45284 = CARTESIAN_POINT('',(10.5,-2.,26.)) ;
#45285 = CARTESIAN_POINT('',(10.5,-2.,24.5)) ;
#45286 = CARTESIAN_POINT('',(5.,-2.,26.)) ;
#45287 = CARTESIAN_POINT('Origin',(10.,2.,24.5)) ;
#45288 = CARTESIAN_POINT('',(10.5,2.,26.)) ;
#45289 = CARTESIAN_POINT('',(10.5,2.,24.5)) ;
#45290 = CARTESIAN_POINT('',(5.,2.,26.)) ;
#45291 = CARTESIAN_POINT('Origin',(10.5,0.,24.5)) ;
#45292 = CARTESIAN_POINT('',(10.5,0.,26.)) ;
#45293 = CARTESIAN_POINT('Origin',(0.,0.,42.1)) ;
#45294 = CARTESIAN_POINT('',(1.79965394597392,-6.76470588235294,42.1)) ;
#45295 = CARTESIAN_POINT('',(-1.79965394597392,-6.76470588235294,42.1)) ;
#45296 = CARTESIAN_POINT('Origin',(0.,-8.5,42.1)) ;
#45297 = CARTESIAN_POINT('Origin',(0.,0.,42.1)) ;
#45298 = CARTESIAN_POINT('Origin',(0.,0.,34.)) ;
#45299 = CARTESIAN_POINT('',(-7.,-8.57252759403147E-16,26.)) ;
#45300 = CARTESIAN_POINT('Origin',(0.,0.,26.)) ;
#45301 = CARTESIAN_POINT('',(-7.,-8.57252759403147E-16,34.)) ;
#45302 = CARTESIAN_POINT('',(-1.79965394597392,-6.76470588235294,34.)) ;
#45303 = CARTESIAN_POINT('',(1.79965394597392,-6.76470588235294,34.)) ;
#45304 = CARTESIAN_POINT('Origin',(0.,-8.5,43.)) ;
#45305 = CARTESIAN_POINT('',(-2.5,-8.5,44.)) ;
#45306 = CARTESIAN_POINT('Origin',(0.,-8.5,44.)) ;
#45307 = CARTESIAN_POINT('',(-2.5,-8.5,43.)) ;
#45308 = CARTESIAN_POINT('Origin',(0.,-8.5,42.05)) ;
#45309 = CARTESIAN_POINT('',(-1.02,-8.5,40.)) ;
#45310 = CARTESIAN_POINT('Origin',(0.,-8.5,40.)) ;
#45311 = CARTESIAN_POINT('',(-1.02,-8.5,44.)) ;
#45312 = CARTESIAN_POINT('',(-1.02,-8.5,42.05)) ;
#45313 = CARTESIAN_POINT('Origin',(0.,-8.5,44.)) ;
#45314 = CARTESIAN_POINT('Origin',(0.,-8.5,40.)) ;
#45315 = CARTESIAN_POINT('Origin',(0.,-8.5,44.)) ;
#45316 = CARTESIAN_POINT('Origin',(0.,-11.55,37.)) ;
#45317 = CARTESIAN_POINT('',(-1.51,-13.,37.)) ;
#45318 = CARTESIAN_POINT('Origin',(0.,-13.,37.)) ;
#45319 = CARTESIAN_POINT('',(-1.51,-10.,37.)) ;
#45320 = CARTESIAN_POINT('',(-1.51,-11.55,37.)) ;
#45321 = CARTESIAN_POINT('Origin',(0.,-10.,37.)) ;
#45322 = CARTESIAN_POINT('Origin',(0.,-10.,37.)) ;
#45323 = CARTESIAN_POINT('Origin',(0.,-12.,37.)) ;
#45324 = CARTESIAN_POINT('',(-3.,-11.,37.)) ;
#45325 = CARTESIAN_POINT('Origin',(0.,-11.,37.)) ;
#45326 = CARTESIAN_POINT('',(-3.,-13.,37.)) ;
#45327 = CARTESIAN_POINT('',(-3.,-12.,37.)) ;
#45328 = CARTESIAN_POINT('Origin',(0.,-13.,37.)) ;
#45329 = CARTESIAN_POINT('Origin',(0.,-13.,37.)) ;
#45330 = CARTESIAN_POINT('Origin',(-12.05,0.,34.)) ;
#45331 = CARTESIAN_POINT('',(-14.,-2.16762483449082E-16,35.77)) ;
#45332 = CARTESIAN_POINT('Origin',(-14.,0.,34.)) ;
#45333 = CARTESIAN_POINT('',(-10.,-2.16762483449082E-16,35.77)) ;
#45334 = CARTESIAN_POINT('',(-12.05,-2.16762483449082E-16,35.77)) ;
#45335 = CARTESIAN_POINT('Origin',(-10.,0.,34.)) ;
#45336 = CARTESIAN_POINT('Origin',(-10.,0.,34.)) ;
#45337 = CARTESIAN_POINT('Origin',(-12.5,0.,34.)) ;
#45338 = CARTESIAN_POINT('',(-14.,-4.28626379701574E-16,37.5)) ;
#45339 = CARTESIAN_POINT('',(-12.5,-4.28626379701574E-16,37.5)) ;
#45340 = CARTESIAN_POINT('Origin',(-14.,0.,34.)) ;
#45341 = CARTESIAN_POINT('Origin',(-14.,0.,34.)) ;
#45342 = CARTESIAN_POINT('Origin',(-8.5,-18.,32.)) ;
#45343 = CARTESIAN_POINT('',(-6.,-25.,32.)) ;
#45344 = CARTESIAN_POINT('',(-6.,-11.,32.)) ;
#45345 = CARTESIAN_POINT('',(-6.,-18.,32.)) ;
#45346 = CARTESIAN_POINT('',(-4.25,-11.,32.)) ;
#45347 = CARTESIAN_POINT('',(-8.5,-25.,32.)) ;
#45348 = CARTESIAN_POINT('Origin',(-8.5,-18.,31.)) ;
#45349 = CARTESIAN_POINT('',(-6.,-11.,31.)) ;
#45350 = CARTESIAN_POINT('',(-6.,-25.,31.)) ;
#45351 = CARTESIAN_POINT('',(-6.,-18.,31.)) ;
#45352 = CARTESIAN_POINT('',(-8.5,-25.,31.)) ;
#45353 = CARTESIAN_POINT('',(-4.25,-11.,31.)) ;
#45354 = CARTESIAN_POINT('Origin',(-8.5,-25.,31.5)) ;
#45355 = CARTESIAN_POINT('',(-6.,-25.,31.5)) ;
#45356 = CARTESIAN_POINT('Origin',(-6.,-18.,31.5)) ;
#45357 = CARTESIAN_POINT('',(-6.,-11.,32.75)) ;
#45358 = CARTESIAN_POINT('Origin',(0.,-11.,34.)) ;
#45359 = CARTESIAN_POINT('',(0.,-11.,26.)) ;
#45360 = CARTESIAN_POINT('',(6.,-11.,31.)) ;
#45361 = CARTESIAN_POINT('',(4.25,-11.,31.)) ;
#45362 = CARTESIAN_POINT('',(6.,-11.,32.)) ;
#45363 = CARTESIAN_POINT('',(6.,-11.,32.75)) ;
#45364 = CARTESIAN_POINT('',(4.25,-11.,32.)) ;
#45365 = CARTESIAN_POINT('Origin',(-8.5,18.,32.)) ;
#45366 = CARTESIAN_POINT('',(-6.,11.,32.)) ;
#45367 = CARTESIAN_POINT('',(-6.,25.,32.)) ;
#45368 = CARTESIAN_POINT('',(-6.,18.,32.)) ;
#45369 = CARTESIAN_POINT('',(-8.5,25.,32.)) ;
#45370 = CARTESIAN_POINT('',(-4.25,11.,32.)) ;
#45371 = CARTESIAN_POINT('Origin',(-8.5,18.,31.)) ;
#45372 = CARTESIAN_POINT('',(-6.,25.,31.)) ;
#45373 = CARTESIAN_POINT('',(-6.,11.,31.)) ;
#45374 = CARTESIAN_POINT('',(-6.,18.,31.)) ;
#45375 = CARTESIAN_POINT('',(-4.25,11.,31.)) ;
#45376 = CARTESIAN_POINT('',(-8.5,25.,31.)) ;
#45377 = CARTESIAN_POINT('Origin',(-8.5,25.,31.5)) ;
#45378 = CARTESIAN_POINT('',(-6.,25.,31.5)) ;
#45379 = CARTESIAN_POINT('Origin',(-6.,18.,31.5)) ;
#45380 = CARTESIAN_POINT('',(-6.,11.,32.75)) ;
#45381 = CARTESIAN_POINT('Origin',(8.5,-18.,32.)) ;
#45382 = CARTESIAN_POINT('',(6.,-25.,32.)) ;
#45383 = CARTESIAN_POINT('',(6.,-18.,32.)) ;
#45384 = CARTESIAN_POINT('',(8.5,-25.,32.)) ;
#45385 = CARTESIAN_POINT('Origin',(8.5,-18.,31.)) ;
#45386 = CARTESIAN_POINT('',(6.,-25.,31.)) ;
#45387 = CARTESIAN_POINT('',(8.5,-25.,31.)) ;
#45388 = CARTESIAN_POINT('',(6.,-18.,31.)) ;
#45389 = CARTESIAN_POINT('Origin',(8.5,-25.,31.5)) ;
#45390 = CARTESIAN_POINT('',(6.,-25.,31.5)) ;
#45391 = CARTESIAN_POINT('Origin',(6.,-18.,31.5)) ;
#45392 = CARTESIAN_POINT('Origin',(8.5,18.,32.)) ;
#45393 = CARTESIAN_POINT('',(6.,25.,32.)) ;
#45394 = CARTESIAN_POINT('',(8.5,25.,32.)) ;
#45395 = CARTESIAN_POINT('',(6.,11.,32.)) ;
#45396 = CARTESIAN_POINT('',(6.,18.,32.)) ;
#45397 = CARTESIAN_POINT('',(4.25,11.,32.)) ;
#45398 = CARTESIAN_POINT('Origin',(8.5,18.,31.)) ;
#45399 = CARTESIAN_POINT('',(6.,11.,31.)) ;
#45400 = CARTESIAN_POINT('',(4.25,11.,31.)) ;
#45401 = CARTESIAN_POINT('',(6.,25.,31.)) ;
#45402 = CARTESIAN_POINT('',(6.,18.,31.)) ;
#45403 = CARTESIAN_POINT('',(8.5,25.,31.)) ;
#45404 = CARTESIAN_POINT('Origin',(6.,18.,31.5)) ;
#45405 = CARTESIAN_POINT('',(6.,25.,31.5)) ;
#45406 = CARTESIAN_POINT('',(6.,11.,32.75)) ;
#45407 = CARTESIAN_POINT('Origin',(8.5,25.,31.5)) ;
#45408 = CARTESIAN_POINT('Origin',(0.,11.,34.)) ;
#45409 = CARTESIAN_POINT('',(0.,11.,26.)) ;
#45410 = CARTESIAN_POINT('Origin',(0.,0.,26.)) ;
#45411 = CARTESIAN_POINT('',(0.,0.,0.)) ;
#45412 = CARTESIAN_POINT('Origin',(11.45,7.,38.)) ;
#45413 = CARTESIAN_POINT('',(11.8,7.,38.49)) ;
#45414 = CARTESIAN_POINT('Origin',(11.8,7.,38.)) ;
#45415 = CARTESIAN_POINT('',(11.1,7.,38.49)) ;
#45416 = CARTESIAN_POINT('',(11.45,7.,38.49)) ;
#45417 = CARTESIAN_POINT('Origin',(11.1,7.,38.)) ;
#45418 = CARTESIAN_POINT('Origin',(11.1,7.,38.)) ;
#45419 = CARTESIAN_POINT('Origin',(12.1,7.60621778264911,38.35)) ;
#45420 = CARTESIAN_POINT('',(11.8,7.80829037686548,38.)) ;
#45421 = CARTESIAN_POINT('',(12.4,7.80829037686548,38.)) ;
#45422 = CARTESIAN_POINT('',(12.1,7.80829037686548,38.)) ;
#45423 = CARTESIAN_POINT('',(11.8,7.40414518843273,38.7)) ;
#45424 = CARTESIAN_POINT('',(11.8,7.60621778264911,38.35)) ;
#45425 = CARTESIAN_POINT('',(12.4,7.40414518843273,38.7)) ;
#45426 = CARTESIAN_POINT('',(12.1,7.40414518843273,38.7)) ;
#45427 = CARTESIAN_POINT('',(12.4,7.60621778264911,38.35)) ;
#45428 = CARTESIAN_POINT('Origin',(12.1,6.39378221735089,37.65)) ;
#45429 = CARTESIAN_POINT('',(11.8,6.19170962313452,38.)) ;
#45430 = CARTESIAN_POINT('',(12.4,6.19170962313452,38.)) ;
#45431 = CARTESIAN_POINT('',(12.1,6.19170962313452,38.)) ;
#45432 = CARTESIAN_POINT('',(11.8,6.59585481156727,37.3)) ;
#45433 = CARTESIAN_POINT('',(11.8,6.39378221735089,37.65)) ;
#45434 = CARTESIAN_POINT('',(12.4,6.59585481156727,37.3)) ;
#45435 = CARTESIAN_POINT('',(12.1,6.59585481156727,37.3)) ;
#45436 = CARTESIAN_POINT('',(12.4,6.39378221735089,37.65)) ;
#45437 = CARTESIAN_POINT('Origin',(11.8,7.,38.)) ;
#45438 = CARTESIAN_POINT('',(11.8,7.40414518843273,37.3)) ;
#45439 = CARTESIAN_POINT('',(11.8,7.60621778264911,37.65)) ;
#45440 = CARTESIAN_POINT('',(11.8,7.,37.3)) ;
#45441 = CARTESIAN_POINT('',(11.8,6.59585481156727,38.7)) ;
#45442 = CARTESIAN_POINT('',(11.8,6.39378221735089,38.35)) ;
#45443 = CARTESIAN_POINT('',(11.8,7.,38.7)) ;
#45444 = CARTESIAN_POINT('Origin',(12.1,7.60621778264911,37.65)) ;
#45445 = CARTESIAN_POINT('',(12.4,7.40414518843273,37.3)) ;
#45446 = CARTESIAN_POINT('',(12.1,7.40414518843273,37.3)) ;
#45447 = CARTESIAN_POINT('',(12.4,7.60621778264911,37.65)) ;
#45448 = CARTESIAN_POINT('Origin',(12.1,6.39378221735089,38.35)) ;
#45449 = CARTESIAN_POINT('',(12.4,6.59585481156727,38.7)) ;
#45450 = CARTESIAN_POINT('',(12.1,6.59585481156727,38.7)) ;
#45451 = CARTESIAN_POINT('',(12.4,6.39378221735089,38.35)) ;
#45452 = CARTESIAN_POINT('Origin',(12.1,7.,37.3)) ;
#45453 = CARTESIAN_POINT('',(12.4,7.,37.3)) ;
#45454 = CARTESIAN_POINT('Origin',(12.1,7.,38.7)) ;
#45455 = CARTESIAN_POINT('',(12.4,7.,38.7)) ;
#45456 = CARTESIAN_POINT('Origin',(12.4,7.,38.)) ;
#45457 = CARTESIAN_POINT('',(0.,0.,0.)) ;
#45458 = CARTESIAN_POINT('Origin',(-47.2,0.,34.)) ;
#45459 = CARTESIAN_POINT('',(-47.2,-1.72409396495667,33.7)) ;
#45460 = CARTESIAN_POINT('',(-47.2,-1.52069063257456,33.7)) ;
#45461 = CARTESIAN_POINT('',(-47.2,-0.875,33.7)) ;
#45462 = CARTESIAN_POINT('',(-47.2,-1.175,32.7031287650657)) ;
#45463 = CARTESIAN_POINT('Origin',(-47.2,0.,34.)) ;
#45464 = CARTESIAN_POINT('',(-47.2,-1.175,32.7844555433772)) ;
#45465 = CARTESIAN_POINT('',(-47.2,-1.175,33.2422277716886)) ;
#45466 = CARTESIAN_POINT('',(-47.2,-0.961744079250633,32.7844555433772)) ;
#45467 = CARTESIAN_POINT('',(-47.2,-0.4375,32.7844555433772)) ;
#45468 = CARTESIAN_POINT('Origin',(-47.2,0.,34.)) ;
#45469 = CARTESIAN_POINT('Origin',(-47.2,0.,34.)) ;
#45470 = CARTESIAN_POINT('',(-47.2,-1.52069063257456,34.3)) ;
#45471 = CARTESIAN_POINT('',(-47.2,-1.72409396495667,34.3)) ;
#45472 = CARTESIAN_POINT('',(-47.2,-0.875,34.3)) ;
#45473 = CARTESIAN_POINT('',(-47.2,-0.961744079250633,35.2155444566228)) ;
#45474 = CARTESIAN_POINT('Origin',(-47.2,0.,34.)) ;
#45475 = CARTESIAN_POINT('',(-47.2,-1.175,35.2155444566228)) ;
#45476 = CARTESIAN_POINT('',(-47.2,-0.4375,35.2155444566228)) ;
#45477 = CARTESIAN_POINT('',(-47.2,-1.175,35.2968712349343)) ;
#45478 = CARTESIAN_POINT('',(-47.2,-1.175,34.7577722283114)) ;
#45479 = CARTESIAN_POINT('Origin',(-47.2,0.,34.)) ;
#45480 = CARTESIAN_POINT('Origin',(-47.2,0.,34.)) ;
#45481 = CARTESIAN_POINT('',(-47.2,-0.575,35.4394009170485)) ;
#45482 = CARTESIAN_POINT('',(-47.2,-0.575,35.6528384676066)) ;
#45483 = CARTESIAN_POINT('',(-47.2,-0.575,34.7577722283114)) ;
#45484 = CARTESIAN_POINT('',(-47.2,0.575,35.4394009170485)) ;
#45485 = CARTESIAN_POINT('Origin',(-47.2,0.,34.)) ;
#45486 = CARTESIAN_POINT('',(-47.2,0.575,35.6528384676066)) ;
#45487 = CARTESIAN_POINT('',(-47.2,0.575,34.7577722283114)) ;
#45488 = CARTESIAN_POINT('Origin',(-47.2,0.,34.)) ;
#45489 = CARTESIAN_POINT('Origin',(-47.2,0.,34.)) ;
#45490 = CARTESIAN_POINT('',(-47.2,0.961744079250633,35.2155444566228)) ;
#45491 = CARTESIAN_POINT('',(-47.2,1.175,35.2155444566228)) ;
#45492 = CARTESIAN_POINT('',(-47.2,0.4375,35.2155444566228)) ;
#45493 = CARTESIAN_POINT('',(-47.2,1.52069063257456,34.3)) ;
#45494 = CARTESIAN_POINT('Origin',(-47.2,0.,34.)) ;
#45495 = CARTESIAN_POINT('',(-47.2,1.72409396495667,34.3)) ;
#45496 = CARTESIAN_POINT('',(-47.2,0.875,34.3)) ;
#45497 = CARTESIAN_POINT('',(-47.2,1.175,35.2968712349343)) ;
#45498 = CARTESIAN_POINT('Origin',(-47.2,0.,34.)) ;
#45499 = CARTESIAN_POINT('',(-47.2,1.175,34.7577722283114)) ;
#45500 = CARTESIAN_POINT('Origin',(-47.2,0.,34.)) ;
#45501 = CARTESIAN_POINT('',(-47.2,1.52069063257456,33.7)) ;
#45502 = CARTESIAN_POINT('',(-47.2,1.72409396495667,33.7)) ;
#45503 = CARTESIAN_POINT('',(-47.2,0.875,33.7)) ;
#45504 = CARTESIAN_POINT('',(-47.2,0.961744079250633,32.7844555433772)) ;
#45505 = CARTESIAN_POINT('Origin',(-47.2,0.,34.)) ;
#45506 = CARTESIAN_POINT('',(-47.2,1.175,32.7844555433772)) ;
#45507 = CARTESIAN_POINT('',(-47.2,0.4375,32.7844555433772)) ;
#45508 = CARTESIAN_POINT('',(-47.2,1.175,32.7031287650657)) ;
#45509 = CARTESIAN_POINT('',(-47.2,1.175,33.2422277716886)) ;
#45510 = CARTESIAN_POINT('Origin',(-47.2,0.,34.)) ;
#45511 = CARTESIAN_POINT('Origin',(-47.2,0.,34.)) ;
#45512 = CARTESIAN_POINT('',(-47.2,0.575,32.5605990829515)) ;
#45513 = CARTESIAN_POINT('',(-47.2,0.575,32.3471615323934)) ;
#45514 = CARTESIAN_POINT('',(-47.2,0.575,33.2422277716886)) ;
#45515 = CARTESIAN_POINT('',(-47.2,-0.575000000000001,32.5605990829515)) ;
#45516 = CARTESIAN_POINT('Origin',(-47.2,0.,34.)) ;
#45517 = CARTESIAN_POINT('',(-47.2,-0.575000000000001,32.3471615323934)) ;
#45518 = CARTESIAN_POINT('',(-47.2,-0.575000000000001,33.2422277716886)) ;
#45519 = CARTESIAN_POINT('Origin',(-47.2,0.,34.)) ;
#45520 = CARTESIAN_POINT('Origin',(-46.9,0.,34.)) ;
#45521 = CARTESIAN_POINT('',(-46.6,0.961744079250633,35.2155444566228)) ;
#45522 = CARTESIAN_POINT('',(-46.9,0.961744079250633,35.2155444566228)) ;
#45523 = CARTESIAN_POINT('',(-46.6,1.52069063257456,34.3)) ;
#45524 = CARTESIAN_POINT('Origin',(-46.6,0.,34.)) ;
#45525 = CARTESIAN_POINT('',(-46.9,1.52069063257456,34.3)) ;
#45526 = CARTESIAN_POINT('Origin',(-46.9,0.,34.)) ;
#45527 = CARTESIAN_POINT('',(-46.6,-0.575,35.4394009170485)) ;
#45528 = CARTESIAN_POINT('',(-46.9,-0.575,35.4394009170485)) ;
#45529 = CARTESIAN_POINT('',(-46.6,0.575,35.4394009170485)) ;
#45530 = CARTESIAN_POINT('Origin',(-46.6,0.,34.)) ;
#45531 = CARTESIAN_POINT('',(-46.9,0.575,35.4394009170485)) ;
#45532 = CARTESIAN_POINT('Origin',(-46.9,0.,34.)) ;
#45533 = CARTESIAN_POINT('',(-46.6,-1.52069063257456,33.7)) ;
#45534 = CARTESIAN_POINT('',(-46.9,-1.52069063257456,33.7)) ;
#45535 = CARTESIAN_POINT('',(-46.6,-0.961744079250633,32.7844555433772)) ;
#45536 = CARTESIAN_POINT('',(-46.9,-0.961744079250633,32.7844555433772)) ;
#45537 = CARTESIAN_POINT('Origin',(-46.6,0.,34.)) ;
#45538 = CARTESIAN_POINT('Origin',(-46.9,0.,34.)) ;
#45539 = CARTESIAN_POINT('',(-46.6,-1.52069063257456,34.3)) ;
#45540 = CARTESIAN_POINT('',(-46.9,-1.52069063257456,34.3)) ;
#45541 = CARTESIAN_POINT('',(-46.6,-0.961744079250633,35.2155444566228)) ;
#45542 = CARTESIAN_POINT('Origin',(-46.6,0.,34.)) ;
#45543 = CARTESIAN_POINT('',(-46.9,-0.961744079250633,35.2155444566228)) ;
#45544 = CARTESIAN_POINT('Origin',(-46.9,0.,34.)) ;
#45545 = CARTESIAN_POINT('',(-46.6,1.52069063257456,33.7)) ;
#45546 = CARTESIAN_POINT('',(-46.9,1.52069063257456,33.7)) ;
#45547 = CARTESIAN_POINT('',(-46.6,0.961744079250633,32.7844555433772)) ;
#45548 = CARTESIAN_POINT('Origin',(-46.6,0.,34.)) ;
#45549 = CARTESIAN_POINT('',(-46.9,0.961744079250633,32.7844555433772)) ;
#45550 = CARTESIAN_POINT('Origin',(-46.9,0.,34.)) ;
#45551 = CARTESIAN_POINT('',(-46.6,0.575,32.5605990829515)) ;
#45552 = CARTESIAN_POINT('',(-46.9,0.575,32.5605990829515)) ;
#45553 = CARTESIAN_POINT('',(-46.6,-0.575000000000001,32.5605990829515)) ;
#45554 = CARTESIAN_POINT('Origin',(-46.6,0.,34.)) ;
#45555 = CARTESIAN_POINT('',(-46.9,-0.575000000000001,32.5605990829515)) ;
#45556 = CARTESIAN_POINT('Origin',(-46.6,0.,34.)) ;
#45557 = CARTESIAN_POINT('',(-46.6,-1.72409396495667,33.7)) ;
#45558 = CARTESIAN_POINT('',(-46.6,-0.875,33.7)) ;
#45559 = CARTESIAN_POINT('',(-46.6,-1.175,32.7844555433772)) ;
#45560 = CARTESIAN_POINT('',(-46.6,-0.4375,32.7844555433772)) ;
#45561 = CARTESIAN_POINT('',(-46.6,-1.175,32.7031287650657)) ;
#45562 = CARTESIAN_POINT('',(-46.6,-1.175,33.2422277716886)) ;
#45563 = CARTESIAN_POINT('Origin',(-46.6,0.,34.)) ;
#45564 = CARTESIAN_POINT('Origin',(-46.6,0.,34.)) ;
#45565 = CARTESIAN_POINT('',(-46.6,-0.575,35.6528384676066)) ;
#45566 = CARTESIAN_POINT('',(-46.6,-0.575,34.7577722283114)) ;
#45567 = CARTESIAN_POINT('',(-46.6,-2.14313189850787E-16,35.75)) ;
#45568 = CARTESIAN_POINT('Origin',(-46.6,0.,34.)) ;
#45569 = CARTESIAN_POINT('',(-46.6,0.575,35.6528384676066)) ;
#45570 = CARTESIAN_POINT('Origin',(-46.6,0.,34.)) ;
#45571 = CARTESIAN_POINT('',(-46.6,0.575,34.7577722283114)) ;
#45572 = CARTESIAN_POINT('Origin',(-46.6,0.,34.)) ;
#45573 = CARTESIAN_POINT('',(-46.6,1.175,35.2155444566228)) ;
#45574 = CARTESIAN_POINT('',(-46.6,0.4375,35.2155444566228)) ;
#45575 = CARTESIAN_POINT('',(-46.6,1.175,35.2968712349343)) ;
#45576 = CARTESIAN_POINT('',(-46.6,1.175,34.7577722283114)) ;
#45577 = CARTESIAN_POINT('',(-46.6,1.72409396495667,34.3)) ;
#45578 = CARTESIAN_POINT('Origin',(-46.6,0.,34.)) ;
#45579 = CARTESIAN_POINT('',(-46.6,0.875,34.3)) ;
#45580 = CARTESIAN_POINT('Origin',(-46.6,0.,34.)) ;
#45581 = CARTESIAN_POINT('',(-46.6,1.72409396495667,33.7)) ;
#45582 = CARTESIAN_POINT('',(-46.6,0.875,33.7)) ;
#45583 = CARTESIAN_POINT('',(-46.6,1.175,32.7031287650657)) ;
#45584 = CARTESIAN_POINT('Origin',(-46.6,0.,34.)) ;
#45585 = CARTESIAN_POINT('',(-46.6,1.175,32.7844555433772)) ;
#45586 = CARTESIAN_POINT('',(-46.6,1.175,33.2422277716886)) ;
#45587 = CARTESIAN_POINT('',(-46.6,0.4375,32.7844555433772)) ;
#45588 = CARTESIAN_POINT('Origin',(-46.6,0.,34.)) ;
#45589 = CARTESIAN_POINT('',(-46.6,-1.72409396495667,34.3)) ;
#45590 = CARTESIAN_POINT('',(-46.6,-0.875,34.3)) ;
#45591 = CARTESIAN_POINT('',(-46.6,-1.175,35.2968712349343)) ;
#45592 = CARTESIAN_POINT('Origin',(-46.6,0.,34.)) ;
#45593 = CARTESIAN_POINT('',(-46.6,-1.175,35.2155444566228)) ;
#45594 = CARTESIAN_POINT('',(-46.6,-1.175,34.7577722283114)) ;
#45595 = CARTESIAN_POINT('',(-46.6,-0.4375,35.2155444566228)) ;
#45596 = CARTESIAN_POINT('Origin',(-46.6,0.,34.)) ;
#45597 = CARTESIAN_POINT('',(-46.6,0.575,32.3471615323934)) ;
#45598 = CARTESIAN_POINT('',(-46.6,0.575,33.2422277716886)) ;
#45599 = CARTESIAN_POINT('',(-46.6,-0.575000000000001,32.3471615323934)) ;
#45600 = CARTESIAN_POINT('Origin',(-46.6,0.,34.)) ;
#45601 = CARTESIAN_POINT('',(-46.6,-0.575000000000001,33.2422277716886)) ;
#45602 = CARTESIAN_POINT('Origin',(-48.,0.575,32.4844555433772)) ;
#45603 = CARTESIAN_POINT('',(-52.,0.575,32.3471615323934)) ;
#45604 = CARTESIAN_POINT('',(-45.,0.575,32.3471615323934)) ;
#45605 = CARTESIAN_POINT('',(-52.,0.575,32.7844555433772)) ;
#45606 = CARTESIAN_POINT('',(-52.,0.575,33.2422277716886)) ;
#45607 = CARTESIAN_POINT('',(-44.,0.575,32.7844555433772)) ;
#45608 = CARTESIAN_POINT('',(-48.,0.575,32.7844555433772)) ;
#45609 = CARTESIAN_POINT('',(-44.,0.575,32.3471615323934)) ;
#45610 = CARTESIAN_POINT('',(-44.,0.575,32.4844555433772)) ;
#45611 = CARTESIAN_POINT('',(-45.,0.575,32.3471615323934)) ;
#45612 = CARTESIAN_POINT('Origin',(-48.,-1.75,34.3)) ;
#45613 = CARTESIAN_POINT('',(-52.,-1.72409396495667,34.3)) ;
#45614 = CARTESIAN_POINT('',(-45.,-1.72409396495667,34.3)) ;
#45615 = CARTESIAN_POINT('',(-52.,-1.45,34.3)) ;
#45616 = CARTESIAN_POINT('',(-52.,-0.875,34.3)) ;
#45617 = CARTESIAN_POINT('',(-44.,-1.45,34.3)) ;
#45618 = CARTESIAN_POINT('',(-48.,-1.45,34.3)) ;
#45619 = CARTESIAN_POINT('',(-44.,-1.72409396495667,34.3)) ;
#45620 = CARTESIAN_POINT('',(-44.,-1.75,34.3)) ;
#45621 = CARTESIAN_POINT('',(-45.,-1.72409396495667,34.3)) ;
#45622 = CARTESIAN_POINT('Origin',(-48.,-1.175,35.5155444566228)) ;
#45623 = CARTESIAN_POINT('',(-52.,-1.175,35.2155444566228)) ;
#45624 = CARTESIAN_POINT('',(-48.,-1.175,35.2155444566228)) ;
#45625 = CARTESIAN_POINT('',(-52.,-1.175,35.2968712349343)) ;
#45626 = CARTESIAN_POINT('',(-52.,-1.175,34.7577722283114)) ;
#45627 = CARTESIAN_POINT('',(-45.,-1.175,35.2968712349343)) ;
#45628 = CARTESIAN_POINT('Origin',(-48.,0.875,32.7844555433772)) ;
#45629 = CARTESIAN_POINT('',(-44.,1.175,32.7844555433772)) ;
#45630 = CARTESIAN_POINT('',(-48.,1.175,32.7844555433772)) ;
#45631 = CARTESIAN_POINT('',(-44.,0.875,32.7844555433772)) ;
#45632 = CARTESIAN_POINT('',(-52.,1.175,32.7844555433772)) ;
#45633 = CARTESIAN_POINT('',(-52.,0.4375,32.7844555433772)) ;
#45634 = CARTESIAN_POINT('',(-48.,1.175,32.7844555433772)) ;
#45635 = CARTESIAN_POINT('Origin',(-48.,1.175,32.4844555433772)) ;
#45636 = CARTESIAN_POINT('',(-44.,1.175,32.7031287650657)) ;
#45637 = CARTESIAN_POINT('',(-45.,1.175,32.7031287650657)) ;
#45638 = CARTESIAN_POINT('',(-44.,1.175,32.4844555433772)) ;
#45639 = CARTESIAN_POINT('Origin',(-48.,1.175,32.4844555433772)) ;
#45640 = CARTESIAN_POINT('',(-52.,1.175,32.7031287650657)) ;
#45641 = CARTESIAN_POINT('',(-52.,1.175,33.2422277716886)) ;
#45642 = CARTESIAN_POINT('',(-45.,1.175,32.7031287650657)) ;
#45643 = CARTESIAN_POINT('Origin',(-48.,-1.75,33.7)) ;
#45644 = CARTESIAN_POINT('',(-44.,-1.72409396495667,33.7)) ;
#45645 = CARTESIAN_POINT('',(-45.,-1.72409396495667,33.7)) ;
#45646 = CARTESIAN_POINT('',(-44.,-1.45,33.7)) ;
#45647 = CARTESIAN_POINT('',(-44.,-1.75,33.7)) ;
#45648 = CARTESIAN_POINT('',(-52.,-1.45,33.7)) ;
#45649 = CARTESIAN_POINT('',(-48.,-1.45,33.7)) ;
#45650 = CARTESIAN_POINT('',(-52.,-1.72409396495667,33.7)) ;
#45651 = CARTESIAN_POINT('',(-52.,-0.875,33.7)) ;
#45652 = CARTESIAN_POINT('',(-45.,-1.72409396495667,33.7)) ;
#45653 = CARTESIAN_POINT('Origin',(-48.,-1.175,32.4844555433772)) ;
#45654 = CARTESIAN_POINT('',(-44.,-1.175,32.7844555433772)) ;
#45655 = CARTESIAN_POINT('',(-48.,-1.175,32.7844555433772)) ;
#45656 = CARTESIAN_POINT('',(-44.,-1.175,32.7031287650657)) ;
#45657 = CARTESIAN_POINT('',(-44.,-1.175,32.4844555433772)) ;
#45658 = CARTESIAN_POINT('',(-45.,-1.175,32.7031287650657)) ;
#45659 = CARTESIAN_POINT('Origin',(-48.,1.75,34.3)) ;
#45660 = CARTESIAN_POINT('',(-44.,1.72409396495667,34.3)) ;
#45661 = CARTESIAN_POINT('',(-45.,1.72409396495667,34.3)) ;
#45662 = CARTESIAN_POINT('',(-44.,1.45,34.3)) ;
#45663 = CARTESIAN_POINT('',(-44.,1.75,34.3)) ;
#45664 = CARTESIAN_POINT('',(-52.,1.45,34.3)) ;
#45665 = CARTESIAN_POINT('',(-48.,1.45,34.3)) ;
#45666 = CARTESIAN_POINT('',(-52.,1.72409396495667,34.3)) ;
#45667 = CARTESIAN_POINT('',(-52.,0.875,34.3)) ;
#45668 = CARTESIAN_POINT('',(-45.,1.72409396495667,34.3)) ;
#45669 = CARTESIAN_POINT('Origin',(-48.,1.175,35.5155444566228)) ;
#45670 = CARTESIAN_POINT('',(-44.,1.175,35.2155444566228)) ;
#45671 = CARTESIAN_POINT('',(-48.,1.175,35.2155444566228)) ;
#45672 = CARTESIAN_POINT('',(-44.,1.175,35.2968712349343)) ;
#45673 = CARTESIAN_POINT('',(-44.,1.175,35.5155444566228)) ;
#45674 = CARTESIAN_POINT('',(-45.,1.175,35.2968712349343)) ;
#45675 = CARTESIAN_POINT('Origin',(-48.,1.175,35.5155444566228)) ;
#45676 = CARTESIAN_POINT('',(-52.,1.175,35.2968712349343)) ;
#45677 = CARTESIAN_POINT('',(-45.,1.175,35.2968712349343)) ;
#45678 = CARTESIAN_POINT('',(-52.,1.175,35.2155444566228)) ;
#45679 = CARTESIAN_POINT('',(-52.,1.175,34.7577722283114)) ;
#45680 = CARTESIAN_POINT('',(-48.,1.175,35.2155444566228)) ;
#45681 = CARTESIAN_POINT('Origin',(-48.,0.575,35.5155444566228)) ;
#45682 = CARTESIAN_POINT('',(-44.,0.575,35.6528384676066)) ;
#45683 = CARTESIAN_POINT('',(-45.,0.575,35.6528384676066)) ;
#45684 = CARTESIAN_POINT('',(-44.,0.575,35.2155444566228)) ;
#45685 = CARTESIAN_POINT('',(-44.,0.575,35.5155444566228)) ;
#45686 = CARTESIAN_POINT('',(-52.,0.575,35.2155444566228)) ;
#45687 = CARTESIAN_POINT('',(-48.,0.575,35.2155444566228)) ;
#45688 = CARTESIAN_POINT('',(-52.,0.575,35.6528384676066)) ;
#45689 = CARTESIAN_POINT('',(-52.,0.575,34.7577722283114)) ;
#45690 = CARTESIAN_POINT('',(-45.,0.575,35.6528384676066)) ;
#45691 = CARTESIAN_POINT('Origin',(-45.,0.,34.)) ;
#45692 = CARTESIAN_POINT('',(-52.,-0.575,35.6528384676066)) ;
#45693 = CARTESIAN_POINT('Origin',(-52.,0.,34.)) ;
#45694 = CARTESIAN_POINT('',(-45.,-0.575,35.6528384676066)) ;
#45695 = CARTESIAN_POINT('Origin',(-45.,0.,34.)) ;
#45696 = CARTESIAN_POINT('Origin',(-52.,0.,34.)) ;
#45697 = CARTESIAN_POINT('Origin',(-45.,0.,34.)) ;
#45698 = CARTESIAN_POINT('',(-52.,1.72409396495667,33.7)) ;
#45699 = CARTESIAN_POINT('Origin',(-52.,0.,34.)) ;
#45700 = CARTESIAN_POINT('',(-45.,1.72409396495667,33.7)) ;
#45701 = CARTESIAN_POINT('Origin',(-45.,0.,34.)) ;
#45702 = CARTESIAN_POINT('',(-52.,-1.175,32.7031287650657)) ;
#45703 = CARTESIAN_POINT('Origin',(-52.,0.,34.)) ;
#45704 = CARTESIAN_POINT('',(-45.,-1.175,32.7031287650657)) ;
#45705 = CARTESIAN_POINT('Origin',(-45.,0.,34.)) ;
#45706 = CARTESIAN_POINT('Origin',(-52.,0.,34.)) ;
#45707 = CARTESIAN_POINT('Origin',(-45.,0.,34.)) ;
#45708 = CARTESIAN_POINT('',(-52.,-0.575000000000001,32.3471615323934)) ;
#45709 = CARTESIAN_POINT('',(-45.,-0.575000000000001,32.3471615323934)) ;
#45710 = CARTESIAN_POINT('Origin',(-52.,0.,34.)) ;
#45711 = CARTESIAN_POINT('Origin',(-44.,0.875,32.4844555433772)) ;
#45712 = CARTESIAN_POINT('Origin',(-44.,0.,34.)) ;
#45713 = CARTESIAN_POINT('Origin',(-52.,0.,34.)) ;
#45714 = CARTESIAN_POINT('',(-52.,-0.575000000000001,32.7844555433772)) ;
#45715 = CARTESIAN_POINT('',(-52.,-0.575000000000001,33.2422277716886)) ;
#45716 = CARTESIAN_POINT('',(-52.,-1.175,32.7844555433772)) ;
#45717 = CARTESIAN_POINT('',(-52.,-0.4375,32.7844555433772)) ;
#45718 = CARTESIAN_POINT('',(-52.,-1.175,33.2422277716886)) ;
#45719 = CARTESIAN_POINT('',(-52.,-1.45,34.)) ;
#45720 = CARTESIAN_POINT('',(-52.,-0.575,35.2155444566228)) ;
#45721 = CARTESIAN_POINT('',(-52.,-0.4375,35.2155444566228)) ;
#45722 = CARTESIAN_POINT('',(-52.,-0.575,34.7577722283114)) ;
#45723 = CARTESIAN_POINT('',(-52.,0.4375,35.2155444566228)) ;
#45724 = CARTESIAN_POINT('',(-52.,1.45,33.7)) ;
#45725 = CARTESIAN_POINT('',(-52.,1.45,34.)) ;
#45726 = CARTESIAN_POINT('',(-52.,0.875,33.7)) ;
#45727 = CARTESIAN_POINT('Origin',(-48.,-0.575000000000001,32.4844555433772)) ;
#45728 = CARTESIAN_POINT('',(-44.,-0.575000000000001,32.3471615323934)) ;
#45729 = CARTESIAN_POINT('',(-45.,-0.575000000000001,32.3471615323934)) ;
#45730 = CARTESIAN_POINT('',(-44.,-0.575000000000001,32.7844555433772)) ;
#45731 = CARTESIAN_POINT('',(-44.,-0.575000000000001,32.4844555433772)) ;
#45732 = CARTESIAN_POINT('',(-48.,-0.575000000000001,32.7844555433772)) ;
#45733 = CARTESIAN_POINT('Origin',(-48.,-1.175,32.4844555433772)) ;
#45734 = CARTESIAN_POINT('',(-48.,-1.175,32.7844555433772)) ;
#45735 = CARTESIAN_POINT('Origin',(-48.,-0.875000000000001,32.7844555433772)) ;
#45736 = CARTESIAN_POINT('',(-44.,-0.875000000000001,32.7844555433772)) ;
#45737 = CARTESIAN_POINT('Origin',(-44.,-0.875000000000001,32.4844555433772)) ;
#45738 = CARTESIAN_POINT('Origin',(-44.,0.,34.)) ;
#45739 = CARTESIAN_POINT('Origin',(-44.,-1.75,34.)) ;
#45740 = CARTESIAN_POINT('Origin',(-44.,0.,34.)) ;
#45741 = CARTESIAN_POINT('',(-44.,-1.45,34.)) ;
#45742 = CARTESIAN_POINT('Origin',(-48.,-1.45,34.)) ;
#45743 = CARTESIAN_POINT('Origin',(-45.,0.,34.)) ;
#45744 = CARTESIAN_POINT('',(-38.,-2.14313189850787E-16,35.75)) ;
#45745 = CARTESIAN_POINT('Origin',(-38.,0.,34.)) ;
#45746 = CARTESIAN_POINT('',(-45.,-2.14313189850787E-16,35.75)) ;
#45747 = CARTESIAN_POINT('',(-44.,-0.575,35.6528384676066)) ;
#45748 = CARTESIAN_POINT('',(-45.,-0.575,35.6528384676066)) ;
#45749 = CARTESIAN_POINT('',(-44.,-1.175,35.2968712349343)) ;
#45750 = CARTESIAN_POINT('Origin',(-44.,0.,34.)) ;
#45751 = CARTESIAN_POINT('',(-45.,-1.175,35.2968712349343)) ;
#45752 = CARTESIAN_POINT('',(-44.,1.72409396495667,33.7)) ;
#45753 = CARTESIAN_POINT('',(-45.,1.72409396495667,33.7)) ;
#45754 = CARTESIAN_POINT('Origin',(-44.,0.,34.)) ;
#45755 = CARTESIAN_POINT('Origin',(-44.,0.,34.)) ;
#45756 = CARTESIAN_POINT('Origin',(-48.,-1.175,35.5155444566228)) ;
#45757 = CARTESIAN_POINT('',(-44.,-1.175,35.2155444566228)) ;
#45758 = CARTESIAN_POINT('',(-44.,-1.175,35.5155444566228)) ;
#45759 = CARTESIAN_POINT('',(-48.,-1.175,35.2155444566228)) ;
#45760 = CARTESIAN_POINT('Origin',(-48.,-0.575,35.5155444566228)) ;
#45761 = CARTESIAN_POINT('',(-44.,-0.575,35.2155444566228)) ;
#45762 = CARTESIAN_POINT('',(-48.,-0.575,35.2155444566228)) ;
#45763 = CARTESIAN_POINT('',(-44.,-0.575,35.5155444566228)) ;
#45764 = CARTESIAN_POINT('Origin',(-48.,-0.875,35.2155444566228)) ;
#45765 = CARTESIAN_POINT('',(-44.,-0.875,35.2155444566228)) ;
#45766 = CARTESIAN_POINT('Origin',(-44.,-0.875,35.5155444566228)) ;
#45767 = CARTESIAN_POINT('Origin',(-48.,0.875,35.2155444566228)) ;
#45768 = CARTESIAN_POINT('',(-44.,0.875,35.2155444566228)) ;
#45769 = CARTESIAN_POINT('Origin',(-44.,0.875,35.5155444566228)) ;
#45770 = CARTESIAN_POINT('Origin',(-48.,1.75,33.7)) ;
#45771 = CARTESIAN_POINT('',(-44.,1.45,33.7)) ;
#45772 = CARTESIAN_POINT('',(-48.,1.45,33.7)) ;
#45773 = CARTESIAN_POINT('',(-44.,1.75,33.7)) ;
#45774 = CARTESIAN_POINT('Origin',(-48.,1.45,34.)) ;
#45775 = CARTESIAN_POINT('',(-44.,1.45,34.)) ;
#45776 = CARTESIAN_POINT('Origin',(-44.,1.75,34.)) ;
#45777 = CARTESIAN_POINT('Origin',(-33.5,0.,34.)) ;
#45778 = CARTESIAN_POINT('',(-30.,-2.14313189850787E-16,35.75)) ;
#45779 = CARTESIAN_POINT('Origin',(-30.,0.,34.)) ;
#45780 = CARTESIAN_POINT('',(-37.,-2.14313189850787E-16,35.75)) ;
#45781 = CARTESIAN_POINT('',(-33.5,-2.14313189850787E-16,35.75)) ;
#45782 = CARTESIAN_POINT('Origin',(-37.,0.,34.)) ;
#45783 = CARTESIAN_POINT('Origin',(-30.,0.,34.)) ;
#45784 = CARTESIAN_POINT('Origin',(-38.,0.,34.)) ;
#45785 = CARTESIAN_POINT('',(-38.,-2.69422295812418E-16,36.2)) ;
#45786 = CARTESIAN_POINT('Origin',(-38.,0.,34.)) ;
#45787 = CARTESIAN_POINT('Origin',(-37.5,0.,34.)) ;
#45788 = CARTESIAN_POINT('',(-37.,-2.69422295812418E-16,36.2)) ;
#45789 = CARTESIAN_POINT('Origin',(-37.,0.,34.)) ;
#45790 = CARTESIAN_POINT('',(-37.5,-2.69422295812418E-16,36.2)) ;
#45791 = CARTESIAN_POINT('Origin',(-37.,0.,34.)) ;
#45792 = CARTESIAN_POINT('',(0.,0.,0.)) ;
#45793 = CARTESIAN_POINT('Origin',(-14.35,0.,34.)) ;
#45794 = CARTESIAN_POINT('',(-14.6,-2.14313189850787E-16,35.75)) ;
#45795 = CARTESIAN_POINT('Origin',(-14.6,0.,34.)) ;
#45796 = CARTESIAN_POINT('',(-14.1,2.14313189850787E-16,35.75)) ;
#45797 = CARTESIAN_POINT('',(-14.35,-2.14313189850787E-16,35.75)) ;
#45798 = CARTESIAN_POINT('Origin',(-14.1,0.,34.)) ;
#45799 = CARTESIAN_POINT('Origin',(-14.35,0.,34.)) ;
#45800 = CARTESIAN_POINT('',(-14.1,-3.06161699786838E-16,36.5)) ;
#45801 = CARTESIAN_POINT('Origin',(-14.1,0.,34.)) ;
#45802 = CARTESIAN_POINT('',(-14.6,-3.06161699786838E-16,36.5)) ;
#45803 = CARTESIAN_POINT('',(-14.35,-3.06161699786838E-16,36.5)) ;
#45804 = CARTESIAN_POINT('Origin',(-14.6,0.,34.)) ;
#45805 = CARTESIAN_POINT('Origin',(-14.6,0.,34.)) ;
#45806 = CARTESIAN_POINT('Origin',(-14.1,0.,34.)) ;
#45807 = CARTESIAN_POINT('',(0.,0.,0.)) ;
#45808 = CARTESIAN_POINT('Origin',(-16.1,0.,36.3)) ;
#45809 = CARTESIAN_POINT('',(-16.1,-4.2,35.8761663039294)) ;
#45810 = CARTESIAN_POINT('',(-16.1,4.2,35.8761663039294)) ;
#45811 = CARTESIAN_POINT('Origin',(-16.1,0.,34.)) ;
#45812 = CARTESIAN_POINT('',(-16.1,-4.2,34.)) ;
#45813 = CARTESIAN_POINT('',(-16.1,-4.2,36.3)) ;
#45814 = CARTESIAN_POINT('',(-16.1,4.2,34.)) ;
#45815 = CARTESIAN_POINT('Origin',(-16.1,0.,34.)) ;
#45816 = CARTESIAN_POINT('',(-16.1,4.2,36.3)) ;
#45817 = CARTESIAN_POINT('Origin',(-15.5,4.2,36.3)) ;
#45818 = CARTESIAN_POINT('',(-16.,4.2,35.8761663039294)) ;
#45819 = CARTESIAN_POINT('',(-33.5,4.2,35.8761663039294)) ;
#45820 = CARTESIAN_POINT('',(-15.,4.2,34.)) ;
#45821 = CARTESIAN_POINT('',(-33.5,4.2,34.)) ;
#45822 = CARTESIAN_POINT('',(-15.,4.2,38.6)) ;
#45823 = CARTESIAN_POINT('',(-15.,4.2,35.15)) ;
#45824 = CARTESIAN_POINT('',(-16.,4.2,38.6)) ;
#45825 = CARTESIAN_POINT('',(-15.5,4.2,38.6)) ;
#45826 = CARTESIAN_POINT('',(-16.,4.2,36.65)) ;
#45827 = CARTESIAN_POINT('Origin',(-15.5,0.,38.6)) ;
#45828 = CARTESIAN_POINT('',(-16.,-4.2,38.6)) ;
#45829 = CARTESIAN_POINT('',(-16.,0.,38.6)) ;
#45830 = CARTESIAN_POINT('',(-15.,-4.2,38.6)) ;
#45831 = CARTESIAN_POINT('',(-15.,0.,38.6)) ;
#45832 = CARTESIAN_POINT('',(-15.5,-4.2,38.6)) ;
#45833 = CARTESIAN_POINT('Origin',(-15.5,-4.2,36.3)) ;
#45834 = CARTESIAN_POINT('',(-16.,-4.2,35.8761663039294)) ;
#45835 = CARTESIAN_POINT('',(-33.5,-4.2,35.8761663039294)) ;
#45836 = CARTESIAN_POINT('',(-16.,-4.2,36.65)) ;
#45837 = CARTESIAN_POINT('',(-15.,-4.2,34.)) ;
#45838 = CARTESIAN_POINT('',(-15.,-4.2,35.15)) ;
#45839 = CARTESIAN_POINT('',(-33.5,-4.2,34.)) ;
#45840 = CARTESIAN_POINT('Origin',(-33.5,0.,34.)) ;
#45841 = CARTESIAN_POINT('',(-16.,4.6,34.)) ;
#45842 = CARTESIAN_POINT('Origin',(-16.,0.,34.)) ;
#45843 = CARTESIAN_POINT('',(-52.,4.6,34.)) ;
#45844 = CARTESIAN_POINT('',(-33.5,4.6,34.)) ;
#45845 = CARTESIAN_POINT('',(-52.,-4.6,34.)) ;
#45846 = CARTESIAN_POINT('Origin',(-52.,0.,34.)) ;
#45847 = CARTESIAN_POINT('',(-16.,-4.6,34.)) ;
#45848 = CARTESIAN_POINT('',(-33.5,-4.6,34.)) ;
#45849 = CARTESIAN_POINT('Origin',(-16.,0.,34.)) ;
#45850 = CARTESIAN_POINT('Origin',(-33.5,0.,34.)) ;
#45851 = CARTESIAN_POINT('',(-52.,-4.2,34.)) ;
#45852 = CARTESIAN_POINT('',(-33.5,-4.2,34.)) ;
#45853 = CARTESIAN_POINT('',(-52.,4.2,34.)) ;
#45854 = CARTESIAN_POINT('Origin',(-52.,0.,34.)) ;
#45855 = CARTESIAN_POINT('',(-33.5,4.2,34.)) ;
#45856 = CARTESIAN_POINT('Origin',(-33.5,0.,34.)) ;
#45857 = CARTESIAN_POINT('',(-15.,-4.6,34.)) ;
#45858 = CARTESIAN_POINT('',(-15.,0.,34.)) ;
#45859 = CARTESIAN_POINT('',(-33.5,-4.6,34.)) ;
#45860 = CARTESIAN_POINT('',(-52.,0.,34.)) ;
#45861 = CARTESIAN_POINT('Origin',(-15.,0.,34.)) ;
#45862 = CARTESIAN_POINT('',(-15.,4.6,34.)) ;
#45863 = CARTESIAN_POINT('',(-15.,0.,34.)) ;
#45864 = CARTESIAN_POINT('',(-15.,4.6,40.)) ;
#45865 = CARTESIAN_POINT('',(-15.,4.6,37.)) ;
#45866 = CARTESIAN_POINT('',(-15.,-4.6,40.)) ;
#45867 = CARTESIAN_POINT('',(-15.,0.,40.)) ;
#45868 = CARTESIAN_POINT('',(-15.,-4.6,37.)) ;
#45869 = CARTESIAN_POINT('Origin',(-16.,0.,37.)) ;
#45870 = CARTESIAN_POINT('',(-16.,-4.6,40.)) ;
#45871 = CARTESIAN_POINT('',(-16.,-4.6,37.)) ;
#45872 = CARTESIAN_POINT('',(-16.,4.6,40.)) ;
#45873 = CARTESIAN_POINT('',(-16.,0.,40.)) ;
#45874 = CARTESIAN_POINT('',(-16.,4.6,37.)) ;
#45875 = CARTESIAN_POINT('Origin',(-15.5,0.,40.)) ;
#45876 = CARTESIAN_POINT('',(-15.5,4.6,40.)) ;
#45877 = CARTESIAN_POINT('',(-15.5,-4.6,40.)) ;
#45878 = CARTESIAN_POINT('Origin',(-15.5,-4.6,37.)) ;
#45879 = CARTESIAN_POINT('Origin',(-15.5,4.6,37.)) ;
#45880 = CARTESIAN_POINT('',(-33.5,4.6,34.)) ;
#45881 = CARTESIAN_POINT('Origin',(-33.5,0.,34.)) ;
#45882 = CARTESIAN_POINT('',(-52.,0.,34.)) ;
#45883 = CARTESIAN_POINT('Origin',(-52.,0.,34.)) ;
#45884 = CARTESIAN_POINT('',(0.,0.,0.)) ;
#45885 = CARTESIAN_POINT('Origin',(0.,-12.,37.)) ;
#45886 = CARTESIAN_POINT('',(-1.5,-10.,37.)) ;
#45887 = CARTESIAN_POINT('Origin',(0.,-10.,37.)) ;
#45888 = CARTESIAN_POINT('',(-1.5,-14.,37.)) ;
#45889 = CARTESIAN_POINT('',(-1.5,-12.,37.)) ;
#45890 = CARTESIAN_POINT('Origin',(0.,-14.,37.)) ;
#45891 = CARTESIAN_POINT('Origin',(0.,-14.,37.)) ;
#45892 = CARTESIAN_POINT('Origin',(0.,-10.,37.)) ;
#45893 = CARTESIAN_POINT('',(0.,0.,0.)) ;
#45894 = CARTESIAN_POINT('Origin',(3.,-15.4,37.)) ;
#45895 = CARTESIAN_POINT('',(2.2,-14.,37.)) ;
#45896 = CARTESIAN_POINT('Origin',(3.,-14.,37.)) ;
#45897 = CARTESIAN_POINT('',(2.2,-16.8,37.)) ;
#45898 = CARTESIAN_POINT('',(2.2,-15.4,37.)) ;
#45899 = CARTESIAN_POINT('Origin',(3.,-16.8,37.)) ;
#45900 = CARTESIAN_POINT('Origin',(3.,-16.8,37.)) ;
#45901 = CARTESIAN_POINT('Origin',(0.,-13.5,37.)) ;
#45902 = CARTESIAN_POINT('',(-1.5,-14.,37.)) ;
#45903 = CARTESIAN_POINT('Origin',(0.,-14.,37.)) ;
#45904 = CARTESIAN_POINT('',(-1.5,-13.,37.)) ;
#45905 = CARTESIAN_POINT('',(-1.5,-13.5,37.)) ;
#45906 = CARTESIAN_POINT('Origin',(0.,-13.,37.)) ;
#45907 = CARTESIAN_POINT('Origin',(0.,-13.5,37.)) ;
#45908 = CARTESIAN_POINT('',(-4.5,-13.,37.)) ;
#45909 = CARTESIAN_POINT('Origin',(0.,-13.,37.)) ;
#45910 = CARTESIAN_POINT('',(-4.5,-14.,37.)) ;
#45911 = CARTESIAN_POINT('',(-4.5,-13.5,37.)) ;
#45912 = CARTESIAN_POINT('Origin',(0.,-14.,37.)) ;
#45913 = CARTESIAN_POINT('Origin',(0.,-14.,37.)) ;
#45914 = CARTESIAN_POINT('Origin',(0.,-13.,37.)) ;
#45915 = CARTESIAN_POINT('',(0.,0.,0.)) ;
#45916 = CARTESIAN_POINT('Origin',(0.,-15.7,24.)) ;
#45917 = CARTESIAN_POINT('',(-0.61,-16.2,24.)) ;
#45918 = CARTESIAN_POINT('Origin',(0.,-16.2,24.)) ;
#45919 = CARTESIAN_POINT('',(-0.61,-15.2,24.)) ;
#45920 = CARTESIAN_POINT('',(-0.61,-15.7,24.)) ;
#45921 = CARTESIAN_POINT('Origin',(0.,-15.2,24.)) ;
#45922 = CARTESIAN_POINT('Origin',(0.,-15.7,24.)) ;
#45923 = CARTESIAN_POINT('',(-1.1,-15.2,24.)) ;
#45924 = CARTESIAN_POINT('Origin',(0.,-15.2,24.)) ;
#45925 = CARTESIAN_POINT('',(-1.1,-16.2,24.)) ;
#45926 = CARTESIAN_POINT('',(-1.1,-15.7,24.)) ;
#45927 = CARTESIAN_POINT('Origin',(0.,-16.2,24.)) ;
#45928 = CARTESIAN_POINT('Origin',(0.,-16.2,24.)) ;
#45929 = CARTESIAN_POINT('Origin',(0.,-15.2,24.)) ;
#45930 = CARTESIAN_POINT('Origin',(3.,-15.7,37.)) ;
#45931 = CARTESIAN_POINT('',(2.19,-16.2,37.)) ;
#45932 = CARTESIAN_POINT('Origin',(3.,-16.2,37.)) ;
#45933 = CARTESIAN_POINT('',(2.19,-15.2,37.)) ;
#45934 = CARTESIAN_POINT('',(2.19,-15.7,37.)) ;
#45935 = CARTESIAN_POINT('Origin',(3.,-15.2,37.)) ;
#45936 = CARTESIAN_POINT('Origin',(3.,-15.7,37.)) ;
#45937 = CARTESIAN_POINT('',(1.6,-15.2,37.)) ;
#45938 = CARTESIAN_POINT('Origin',(3.,-15.2,37.)) ;
#45939 = CARTESIAN_POINT('',(1.6,-16.2,37.)) ;
#45940 = CARTESIAN_POINT('',(1.6,-15.7,37.)) ;
#45941 = CARTESIAN_POINT('Origin',(3.,-16.2,37.)) ;
#45942 = CARTESIAN_POINT('Origin',(3.,-16.2,37.)) ;
#45943 = CARTESIAN_POINT('Origin',(3.,-15.2,37.)) ;
#45944 = CARTESIAN_POINT('Origin',(1.46616541353383,-15.7,30.3533834586466)) ;
#45945 = CARTESIAN_POINT('',(-0.336514416664893,-15.7,25.2101036739441)) ;
#45946 = CARTESIAN_POINT('Origin',(0.24812030075188,-15.7,25.0751879699248)) ;
#45947 = CARTESIAN_POINT('',(2.09957580889902,-15.7,35.7664946513877)) ;
#45948 = CARTESIAN_POINT('',(0.881530696117062,-15.7,30.4882991626659)) ;
#45949 = CARTESIAN_POINT('Origin',(2.68421052631579,-15.7,35.6315789473684)) ;
#45950 = CARTESIAN_POINT('Origin',(2.68421052631579,-15.7,35.6315789473684)) ;
#45951 = CARTESIAN_POINT('Origin',(0.24812030075188,-15.7,25.0751879699248)) ;
#45952 = CARTESIAN_POINT('',(0.,0.,0.)) ;
#45953 = CARTESIAN_POINT('Origin',(0.,-8.5,44.6)) ;
#45954 = CARTESIAN_POINT('',(-1.6,-8.5,44.6)) ;
#45955 = CARTESIAN_POINT('Origin',(0.,-8.5,44.6)) ;
#45956 = CARTESIAN_POINT('',(-1.,-8.5,44.6)) ;
#45957 = CARTESIAN_POINT('Origin',(0.,-8.5,44.6)) ;
#45958 = CARTESIAN_POINT('Origin',(0.,-8.5,45.2)) ;
#45959 = CARTESIAN_POINT('',(-1.6,-8.5,45.2)) ;
#45960 = CARTESIAN_POINT('Origin',(0.,-8.5,45.2)) ;
#45961 = CARTESIAN_POINT('',(-1.,-8.5,45.2)) ;
#45962 = CARTESIAN_POINT('Origin',(0.,-8.5,45.2)) ;
#45963 = CARTESIAN_POINT('Origin',(0.,-8.5,44.9)) ;
#45964 = CARTESIAN_POINT('',(-1.6,-8.5,44.9)) ;
#45965 = CARTESIAN_POINT('Origin',(0.,-8.5,55.)) ;
#45966 = CARTESIAN_POINT('',(-1.,-8.5,70.)) ;
#45967 = CARTESIAN_POINT('Origin',(0.,-8.5,70.)) ;
#45968 = CARTESIAN_POINT('',(-1.,-8.5,60.5)) ;
#45969 = CARTESIAN_POINT('',(-1.,-8.5,55.)) ;
#45970 = CARTESIAN_POINT('',(-0.866025403784439,-9.,60.5)) ;
#45971 = CARTESIAN_POINT('Origin',(0.,-8.5,60.5)) ;
#45972 = CARTESIAN_POINT('',(-0.866025403784439,-9.,59.5)) ;
#45973 = CARTESIAN_POINT('',(-0.866025403784439,-9.,55.)) ;
#45974 = CARTESIAN_POINT('',(-1.,-8.5,59.5)) ;
#45975 = CARTESIAN_POINT('Origin',(0.,-8.5,59.5)) ;
#45976 = CARTESIAN_POINT('',(-1.,-8.5,52.5)) ;
#45977 = CARTESIAN_POINT('',(-1.,-8.5,55.)) ;
#45978 = CARTESIAN_POINT('',(-0.866025403784439,-9.,52.5)) ;
#45979 = CARTESIAN_POINT('Origin',(0.,-8.5,52.5)) ;
#45980 = CARTESIAN_POINT('',(-0.866025403784439,-9.,51.5)) ;
#45981 = CARTESIAN_POINT('',(-0.866025403784439,-9.,55.)) ;
#45982 = CARTESIAN_POINT('',(-1.,-8.5,51.5)) ;
#45983 = CARTESIAN_POINT('Origin',(0.,-8.5,51.5)) ;
#45984 = CARTESIAN_POINT('',(-1.,-8.5,55.)) ;
#45985 = CARTESIAN_POINT('',(-0.866025403784439,-8.,51.5)) ;
#45986 = CARTESIAN_POINT('Origin',(0.,-8.5,51.5)) ;
#45987 = CARTESIAN_POINT('',(-0.866025403784439,-8.,52.5)) ;
#45988 = CARTESIAN_POINT('',(-0.866025403784439,-8.,55.)) ;
#45989 = CARTESIAN_POINT('Origin',(0.,-8.5,52.5)) ;
#45990 = CARTESIAN_POINT('',(-0.866025403784439,-8.,59.5)) ;
#45991 = CARTESIAN_POINT('Origin',(0.,-8.5,59.5)) ;
#45992 = CARTESIAN_POINT('',(-0.866025403784439,-8.,60.5)) ;
#45993 = CARTESIAN_POINT('',(-0.866025403784439,-8.,55.)) ;
#45994 = CARTESIAN_POINT('Origin',(0.,-8.5,60.5)) ;
#45995 = CARTESIAN_POINT('',(0.866025403784439,-8.,52.5)) ;
#45996 = CARTESIAN_POINT('',(0.866025403784439,-8.,51.5)) ;
#45997 = CARTESIAN_POINT('',(0.866025403784439,-8.,55.)) ;
#45998 = CARTESIAN_POINT('',(0.866025403784439,-9.,51.5)) ;
#45999 = CARTESIAN_POINT('Origin',(0.,-8.5,51.5)) ;
#46000 = CARTESIAN_POINT('',(0.866025403784439,-9.,52.5)) ;
#46001 = CARTESIAN_POINT('',(0.866025403784439,-9.,55.)) ;
#46002 = CARTESIAN_POINT('Origin',(0.,-8.5,52.5)) ;
#46003 = CARTESIAN_POINT('',(-0.5,-9.36602540378444,51.5)) ;
#46004 = CARTESIAN_POINT('',(-0.5,-9.36602540378444,52.5)) ;
#46005 = CARTESIAN_POINT('',(-0.5,-9.36602540378444,55.)) ;
#46006 = CARTESIAN_POINT('',(0.5,-9.36602540378444,52.5)) ;
#46007 = CARTESIAN_POINT('Origin',(0.,-8.5,52.5)) ;
#46008 = CARTESIAN_POINT('',(0.5,-9.36602540378444,51.5)) ;
#46009 = CARTESIAN_POINT('',(0.5,-9.36602540378444,55.)) ;
#46010 = CARTESIAN_POINT('Origin',(0.,-8.5,51.5)) ;
#46011 = CARTESIAN_POINT('',(-0.5,-7.63397459621556,52.5)) ;
#46012 = CARTESIAN_POINT('',(-0.5,-7.63397459621556,51.5)) ;
#46013 = CARTESIAN_POINT('',(-0.5,-7.63397459621556,55.)) ;
#46014 = CARTESIAN_POINT('',(0.5,-7.63397459621556,51.5)) ;
#46015 = CARTESIAN_POINT('Origin',(0.,-8.5,51.5)) ;
#46016 = CARTESIAN_POINT('',(0.5,-7.63397459621556,52.5)) ;
#46017 = CARTESIAN_POINT('',(0.5,-7.63397459621556,55.)) ;
#46018 = CARTESIAN_POINT('Origin',(0.,-8.5,52.5)) ;
#46019 = CARTESIAN_POINT('',(0.866025403784439,-8.,60.5)) ;
#46020 = CARTESIAN_POINT('',(0.866025403784439,-8.,59.5)) ;
#46021 = CARTESIAN_POINT('',(0.866025403784439,-8.,55.)) ;
#46022 = CARTESIAN_POINT('',(0.866025403784439,-9.,59.5)) ;
#46023 = CARTESIAN_POINT('Origin',(0.,-8.5,59.5)) ;
#46024 = CARTESIAN_POINT('',(0.866025403784439,-9.,60.5)) ;
#46025 = CARTESIAN_POINT('',(0.866025403784439,-9.,55.)) ;
#46026 = CARTESIAN_POINT('Origin',(0.,-8.5,60.5)) ;
#46027 = CARTESIAN_POINT('',(-0.5,-9.36602540378444,59.5)) ;
#46028 = CARTESIAN_POINT('',(-0.5,-9.36602540378444,60.5)) ;
#46029 = CARTESIAN_POINT('',(-0.5,-9.36602540378444,55.)) ;
#46030 = CARTESIAN_POINT('',(0.5,-9.36602540378444,60.5)) ;
#46031 = CARTESIAN_POINT('Origin',(0.,-8.5,60.5)) ;
#46032 = CARTESIAN_POINT('',(0.5,-9.36602540378444,59.5)) ;
#46033 = CARTESIAN_POINT('',(0.5,-9.36602540378444,55.)) ;
#46034 = CARTESIAN_POINT('Origin',(0.,-8.5,59.5)) ;
#46035 = CARTESIAN_POINT('',(-0.5,-7.63397459621556,60.5)) ;
#46036 = CARTESIAN_POINT('',(-0.5,-7.63397459621556,59.5)) ;
#46037 = CARTESIAN_POINT('',(-0.5,-7.63397459621556,55.)) ;
#46038 = CARTESIAN_POINT('',(0.5,-7.63397459621556,59.5)) ;
#46039 = CARTESIAN_POINT('Origin',(0.,-8.5,59.5)) ;
#46040 = CARTESIAN_POINT('',(0.5,-7.63397459621556,60.5)) ;
#46041 = CARTESIAN_POINT('',(0.5,-7.63397459621556,55.)) ;
#46042 = CARTESIAN_POINT('Origin',(0.,-8.5,60.5)) ;
#46043 = CARTESIAN_POINT('Origin',(0.5,-8.5,60.)) ;
#46044 = CARTESIAN_POINT('',(0.5,-15.5,60.5)) ;
#46045 = CARTESIAN_POINT('',(0.5,-8.5,60.5)) ;
#46046 = CARTESIAN_POINT('',(0.5,-15.5,59.5)) ;
#46047 = CARTESIAN_POINT('',(0.5,-15.5,60.)) ;
#46048 = CARTESIAN_POINT('',(0.5,-8.5,59.5)) ;
#46049 = CARTESIAN_POINT('Origin',(0.,-8.5,60.5)) ;
#46050 = CARTESIAN_POINT('',(-0.5,-15.5,60.5)) ;
#46051 = CARTESIAN_POINT('',(-0.5,-8.5,60.5)) ;
#46052 = CARTESIAN_POINT('',(-4.28626379701574E-16,-15.5,60.5)) ;
#46053 = CARTESIAN_POINT('Origin',(0.,-8.5,59.5)) ;
#46054 = CARTESIAN_POINT('',(-0.5,-15.5,59.5)) ;
#46055 = CARTESIAN_POINT('',(-4.28626379701574E-16,-15.5,59.5)) ;
#46056 = CARTESIAN_POINT('',(-0.5,-8.5,59.5)) ;
#46057 = CARTESIAN_POINT('Origin',(0.,-8.5,59.5)) ;
#46058 = CARTESIAN_POINT('',(-0.5,-1.5,59.5)) ;
#46059 = CARTESIAN_POINT('',(-0.5,-8.5,59.5)) ;
#46060 = CARTESIAN_POINT('',(0.5,-1.5,59.5)) ;
#46061 = CARTESIAN_POINT('',(4.28626379701574E-16,-1.5,59.5)) ;
#46062 = CARTESIAN_POINT('',(0.5,-8.5,59.5)) ;
#46063 = CARTESIAN_POINT('Origin',(-0.5,-8.5,60.)) ;
#46064 = CARTESIAN_POINT('',(-0.5,-15.5,60.)) ;
#46065 = CARTESIAN_POINT('Origin',(-0.5,-8.5,60.)) ;
#46066 = CARTESIAN_POINT('',(-0.5,-1.5,60.5)) ;
#46067 = CARTESIAN_POINT('',(-0.5,-8.5,60.5)) ;
#46068 = CARTESIAN_POINT('',(-0.5,-1.5,60.)) ;
#46069 = CARTESIAN_POINT('Origin',(0.5,-8.5,60.)) ;
#46070 = CARTESIAN_POINT('',(0.5,-1.5,60.5)) ;
#46071 = CARTESIAN_POINT('',(0.5,-1.5,60.)) ;
#46072 = CARTESIAN_POINT('',(0.5,-8.5,60.5)) ;
#46073 = CARTESIAN_POINT('Origin',(-4.28626379701574E-16,-15.5,60.)) ;
#46074 = CARTESIAN_POINT('Origin',(0.,-8.5,60.5)) ;
#46075 = CARTESIAN_POINT('',(4.28626379701574E-16,-1.5,60.5)) ;
#46076 = CARTESIAN_POINT('Origin',(4.28626379701574E-16,-1.5,60.)) ;
#46077 = CARTESIAN_POINT('Origin',(0.,-9.,60.)) ;
#46078 = CARTESIAN_POINT('',(7.,-9.,59.5)) ;
#46079 = CARTESIAN_POINT('',(0.,-9.,59.5)) ;
#46080 = CARTESIAN_POINT('',(7.,-9.,60.5)) ;
#46081 = CARTESIAN_POINT('',(7.,-9.,60.)) ;
#46082 = CARTESIAN_POINT('',(0.,-9.,60.5)) ;
#46083 = CARTESIAN_POINT('Origin',(0.,-8.5,59.5)) ;
#46084 = CARTESIAN_POINT('',(7.,-8.,59.5)) ;
#46085 = CARTESIAN_POINT('',(0.,-8.,59.5)) ;
#46086 = CARTESIAN_POINT('',(7.,-8.5,59.5)) ;
#46087 = CARTESIAN_POINT('Origin',(0.,-8.5,60.5)) ;
#46088 = CARTESIAN_POINT('',(7.,-8.,60.5)) ;
#46089 = CARTESIAN_POINT('',(7.,-8.5,60.5)) ;
#46090 = CARTESIAN_POINT('',(0.,-8.,60.5)) ;
#46091 = CARTESIAN_POINT('Origin',(0.,-8.5,60.5)) ;
#46092 = CARTESIAN_POINT('',(-7.,-8.,60.5)) ;
#46093 = CARTESIAN_POINT('',(0.,-8.,60.5)) ;
#46094 = CARTESIAN_POINT('',(-7.,-9.,60.5)) ;
#46095 = CARTESIAN_POINT('',(-7.,-8.5,60.5)) ;
#46096 = CARTESIAN_POINT('',(0.,-9.,60.5)) ;
#46097 = CARTESIAN_POINT('Origin',(0.,-8.,60.)) ;
#46098 = CARTESIAN_POINT('',(7.,-8.,60.)) ;
#46099 = CARTESIAN_POINT('Origin',(0.,-8.,60.)) ;
#46100 = CARTESIAN_POINT('',(-7.,-8.,59.5)) ;
#46101 = CARTESIAN_POINT('',(0.,-8.,59.5)) ;
#46102 = CARTESIAN_POINT('',(-7.,-8.,60.)) ;
#46103 = CARTESIAN_POINT('Origin',(0.,-9.,60.)) ;
#46104 = CARTESIAN_POINT('',(-7.,-9.,59.5)) ;
#46105 = CARTESIAN_POINT('',(-7.,-9.,60.)) ;
#46106 = CARTESIAN_POINT('',(0.,-9.,59.5)) ;
#46107 = CARTESIAN_POINT('Origin',(0.,-8.5,59.5)) ;
#46108 = CARTESIAN_POINT('',(-7.,-8.5,59.5)) ;
#46109 = CARTESIAN_POINT('Origin',(-7.,-8.5,60.)) ;
#46110 = CARTESIAN_POINT('Origin',(7.,-8.5,60.)) ;
#46111 = CARTESIAN_POINT('Origin',(0.5,-8.5,52.)) ;
#46112 = CARTESIAN_POINT('',(0.5,-12.5,52.5)) ;
#46113 = CARTESIAN_POINT('',(0.5,-8.5,52.5)) ;
#46114 = CARTESIAN_POINT('',(0.5,-12.5,51.5)) ;
#46115 = CARTESIAN_POINT('',(0.5,-12.5,52.)) ;
#46116 = CARTESIAN_POINT('',(0.5,-8.5,51.5)) ;
#46117 = CARTESIAN_POINT('Origin',(0.,-8.5,52.5)) ;
#46118 = CARTESIAN_POINT('',(-0.5,-12.5,52.5)) ;
#46119 = CARTESIAN_POINT('',(-0.5,-8.5,52.5)) ;
#46120 = CARTESIAN_POINT('',(-2.44929359829471E-16,-12.5,52.5)) ;
#46121 = CARTESIAN_POINT('Origin',(0.,-8.5,51.5)) ;
#46122 = CARTESIAN_POINT('',(-0.5,-12.5,51.5)) ;
#46123 = CARTESIAN_POINT('',(-2.44929359829471E-16,-12.5,51.5)) ;
#46124 = CARTESIAN_POINT('',(-0.5,-8.5,51.5)) ;
#46125 = CARTESIAN_POINT('Origin',(0.,-8.5,51.5)) ;
#46126 = CARTESIAN_POINT('',(-0.5,-4.5,51.5)) ;
#46127 = CARTESIAN_POINT('',(-0.5,-8.5,51.5)) ;
#46128 = CARTESIAN_POINT('',(0.5,-4.5,51.5)) ;
#46129 = CARTESIAN_POINT('',(2.44929359829471E-16,-4.5,51.5)) ;
#46130 = CARTESIAN_POINT('',(0.5,-8.5,51.5)) ;
#46131 = CARTESIAN_POINT('Origin',(-0.5,-8.5,52.)) ;
#46132 = CARTESIAN_POINT('',(-0.5,-12.5,52.)) ;
#46133 = CARTESIAN_POINT('Origin',(-0.5,-8.5,52.)) ;
#46134 = CARTESIAN_POINT('',(-0.5,-4.5,52.5)) ;
#46135 = CARTESIAN_POINT('',(-0.5,-8.5,52.5)) ;
#46136 = CARTESIAN_POINT('',(-0.5,-4.5,52.)) ;
#46137 = CARTESIAN_POINT('Origin',(0.5,-8.5,52.)) ;
#46138 = CARTESIAN_POINT('',(0.5,-4.5,52.5)) ;
#46139 = CARTESIAN_POINT('',(0.5,-4.5,52.)) ;
#46140 = CARTESIAN_POINT('',(0.5,-8.5,52.5)) ;
#46141 = CARTESIAN_POINT('Origin',(-2.44929359829471E-16,-12.5,52.)) ;
#46142 = CARTESIAN_POINT('Origin',(0.,-8.5,52.5)) ;
#46143 = CARTESIAN_POINT('',(2.44929359829471E-16,-4.5,52.5)) ;
#46144 = CARTESIAN_POINT('Origin',(2.44929359829471E-16,-4.5,52.)) ;
#46145 = CARTESIAN_POINT('Origin',(0.,-9.,52.)) ;
#46146 = CARTESIAN_POINT('',(4.,-9.,51.5)) ;
#46147 = CARTESIAN_POINT('',(0.,-9.,51.5)) ;
#46148 = CARTESIAN_POINT('',(4.,-9.,52.5)) ;
#46149 = CARTESIAN_POINT('',(4.,-9.,52.)) ;
#46150 = CARTESIAN_POINT('',(0.,-9.,52.5)) ;
#46151 = CARTESIAN_POINT('Origin',(0.,-8.5,51.5)) ;
#46152 = CARTESIAN_POINT('',(4.,-8.,51.5)) ;
#46153 = CARTESIAN_POINT('',(0.,-8.,51.5)) ;
#46154 = CARTESIAN_POINT('',(4.,-8.5,51.5)) ;
#46155 = CARTESIAN_POINT('Origin',(0.,-8.5,52.5)) ;
#46156 = CARTESIAN_POINT('',(4.,-8.,52.5)) ;
#46157 = CARTESIAN_POINT('',(4.,-8.5,52.5)) ;
#46158 = CARTESIAN_POINT('',(0.,-8.,52.5)) ;
#46159 = CARTESIAN_POINT('Origin',(0.,-8.5,52.5)) ;
#46160 = CARTESIAN_POINT('',(-4.,-8.,52.5)) ;
#46161 = CARTESIAN_POINT('',(0.,-8.,52.5)) ;
#46162 = CARTESIAN_POINT('',(-4.,-9.,52.5)) ;
#46163 = CARTESIAN_POINT('',(-4.,-8.5,52.5)) ;
#46164 = CARTESIAN_POINT('',(0.,-9.,52.5)) ;
#46165 = CARTESIAN_POINT('Origin',(0.,-8.,52.)) ;
#46166 = CARTESIAN_POINT('',(4.,-8.,52.)) ;
#46167 = CARTESIAN_POINT('Origin',(0.,-8.,52.)) ;
#46168 = CARTESIAN_POINT('',(-4.,-8.,51.5)) ;
#46169 = CARTESIAN_POINT('',(0.,-8.,51.5)) ;
#46170 = CARTESIAN_POINT('',(-4.,-8.,52.)) ;
#46171 = CARTESIAN_POINT('Origin',(0.,-9.,52.)) ;
#46172 = CARTESIAN_POINT('',(-4.,-9.,51.5)) ;
#46173 = CARTESIAN_POINT('',(-4.,-9.,52.)) ;
#46174 = CARTESIAN_POINT('',(0.,-9.,51.5)) ;
#46175 = CARTESIAN_POINT('Origin',(0.,-8.5,51.5)) ;
#46176 = CARTESIAN_POINT('',(-4.,-8.5,51.5)) ;
#46177 = CARTESIAN_POINT('Origin',(-4.,-8.5,52.)) ;
#46178 = CARTESIAN_POINT('Origin',(4.,-8.5,52.)) ;
#46179 = CARTESIAN_POINT('Origin',(0.,-8.5,55.)) ;
#46180 = CARTESIAN_POINT('',(-1.,-8.5,40.)) ;
#46181 = CARTESIAN_POINT('',(-1.,-8.5,55.)) ;
#46182 = CARTESIAN_POINT('Origin',(0.,-8.5,40.)) ;
#46183 = CARTESIAN_POINT('Origin',(0.,-8.5,40.)) ;
#46184 = CARTESIAN_POINT('Origin',(0.,-8.5,70.)) ;
#46185 = CARTESIAN_POINT('',(0.,0.,0.)) ;
#46186 = CARTESIAN_POINT('Origin',(0.,-8.5,44.3)) ;
#46187 = CARTESIAN_POINT('',(-1.,-8.5,44.)) ;
#46188 = CARTESIAN_POINT('Origin',(0.,-8.5,44.)) ;
#46189 = CARTESIAN_POINT('',(-1.,-8.5,44.6)) ;
#46190 = CARTESIAN_POINT('',(-1.,-8.5,44.3)) ;
#46191 = CARTESIAN_POINT('Origin',(0.,-8.5,44.6)) ;
#46192 = CARTESIAN_POINT('Origin',(0.,-8.5,44.3)) ;
#46193 = CARTESIAN_POINT('',(-1.6,-8.5,44.6)) ;
#46194 = CARTESIAN_POINT('Origin',(0.,-8.5,44.6)) ;
#46195 = CARTESIAN_POINT('',(-1.6,-8.5,44.)) ;
#46196 = CARTESIAN_POINT('',(-1.6,-8.5,44.3)) ;
#46197 = CARTESIAN_POINT('Origin',(0.,-8.5,44.)) ;
#46198 = CARTESIAN_POINT('Origin',(0.,-8.5,44.)) ;
#46199 = CARTESIAN_POINT('Origin',(0.,-8.5,44.6)) ;
#46200 = CARTESIAN_POINT('',(0.,0.,0.)) ;
#46201 = CARTESIAN_POINT('',(0.,0.,0.)) ;
#46202 = CARTESIAN_POINT('',(0.,0.,0.)) ;
#46203 = CARTESIAN_POINT('',(0.,0.,0.)) ;
#46204 = CARTESIAN_POINT('',(0.,0.,0.)) ;
#46205 = CARTESIAN_POINT('',(0.,0.,0.)) ;
#46206 = CARTESIAN_POINT('',(0.,0.,0.)) ;
#46207 = CARTESIAN_POINT('',(0.,0.,0.)) ;
#46208 = CARTESIAN_POINT('',(0.,0.,0.)) ;
#46209 = CARTESIAN_POINT('',(0.,0.,0.)) ;
#46210 = CARTESIAN_POINT('',(0.,0.,0.)) ;
#46211 = CARTESIAN_POINT('',(0.,0.,0.)) ;
#46212 = CARTESIAN_POINT('Origin',(31.9,0.,44.)) ;
#46213 = CARTESIAN_POINT('',(31.64,-3.18408167778312E-17,43.8)) ;
#46214 = CARTESIAN_POINT('Origin',(31.9,0.,43.8)) ;
#46215 = CARTESIAN_POINT('',(31.64,3.18408167778312E-17,44.2)) ;
#46216 = CARTESIAN_POINT('',(31.64,-3.18408167778312E-17,44.)) ;
#46217 = CARTESIAN_POINT('Origin',(31.9,0.,44.2)) ;
#46218 = CARTESIAN_POINT('Origin',(32.1,0.,43.8)) ;
#46219 = CARTESIAN_POINT('',(32.6,-1.,43.8)) ;
#46220 = CARTESIAN_POINT('',(32.6,1.,43.8)) ;
#46221 = CARTESIAN_POINT('',(32.6,0.,43.8)) ;
#46222 = CARTESIAN_POINT('',(31.,-1.,43.8)) ;
#46223 = CARTESIAN_POINT('',(32.1,-1.,43.8)) ;
#46224 = CARTESIAN_POINT('',(31.,1.,43.8)) ;
#46225 = CARTESIAN_POINT('',(31.,0.,43.8)) ;
#46226 = CARTESIAN_POINT('',(32.1,1.,43.8)) ;
#46227 = CARTESIAN_POINT('Origin',(31.,0.,44.)) ;
#46228 = CARTESIAN_POINT('',(31.,1.,44.2)) ;
#46229 = CARTESIAN_POINT('',(31.,1.,44.)) ;
#46230 = CARTESIAN_POINT('',(31.,-1.,44.2)) ;
#46231 = CARTESIAN_POINT('',(31.,-1.,44.)) ;
#46232 = CARTESIAN_POINT('',(31.,0.,44.2)) ;
#46233 = CARTESIAN_POINT('Origin',(32.9,1.,43.3)) ;
#46234 = CARTESIAN_POINT('',(33.2,1.,44.2)) ;
#46235 = CARTESIAN_POINT('',(33.2,1.,42.4)) ;
#46236 = CARTESIAN_POINT('',(33.2,1.,43.3)) ;
#46237 = CARTESIAN_POINT('',(32.6,1.,42.4)) ;
#46238 = CARTESIAN_POINT('',(19.95,1.,42.4)) ;
#46239 = CARTESIAN_POINT('',(32.6,1.,43.3)) ;
#46240 = CARTESIAN_POINT('',(32.9,1.,44.2)) ;
#46241 = CARTESIAN_POINT('Origin',(33.2,0.,43.3)) ;
#46242 = CARTESIAN_POINT('',(33.2,-1.,44.2)) ;
#46243 = CARTESIAN_POINT('',(33.2,-1.,42.4)) ;
#46244 = CARTESIAN_POINT('',(33.2,-1.,43.3)) ;
#46245 = CARTESIAN_POINT('',(33.2,0.,42.4)) ;
#46246 = CARTESIAN_POINT('',(33.2,0.,44.2)) ;
#46247 = CARTESIAN_POINT('Origin',(32.9,0.,44.2)) ;
#46248 = CARTESIAN_POINT('',(32.9,-1.,44.2)) ;
#46249 = CARTESIAN_POINT('Origin',(32.9,-1.,43.3)) ;
#46250 = CARTESIAN_POINT('',(32.6,-1.,42.4)) ;
#46251 = CARTESIAN_POINT('',(32.6,-1.,43.3)) ;
#46252 = CARTESIAN_POINT('',(19.95,-1.,42.4)) ;
#46253 = CARTESIAN_POINT('Origin',(32.6,0.,43.3)) ;
#46254 = CARTESIAN_POINT('',(32.6,0.,42.4)) ;
#46255 = CARTESIAN_POINT('Origin',(-17.5,0.,43.6)) ;
#46256 = CARTESIAN_POINT('',(-18.,-5.02105187650415E-17,44.01)) ;
#46257 = CARTESIAN_POINT('Origin',(-18.,0.,43.6)) ;
#46258 = CARTESIAN_POINT('',(-17.,5.02105187650415E-17,44.01)) ;
#46259 = CARTESIAN_POINT('',(-17.5,-5.02105187650415E-17,44.01)) ;
#46260 = CARTESIAN_POINT('Origin',(-17.,0.,43.6)) ;
#46261 = CARTESIAN_POINT('Origin',(-17.5,0.,44.6)) ;
#46262 = CARTESIAN_POINT('',(-17.,-1.,44.6)) ;
#46263 = CARTESIAN_POINT('',(-17.,1.,44.6)) ;
#46264 = CARTESIAN_POINT('',(-17.,0.,44.6)) ;
#46265 = CARTESIAN_POINT('',(-18.,1.,44.6)) ;
#46266 = CARTESIAN_POINT('',(-17.5,1.,44.6)) ;
#46267 = CARTESIAN_POINT('',(-18.,-1.,44.6)) ;
#46268 = CARTESIAN_POINT('',(-18.,0.,44.6)) ;
#46269 = CARTESIAN_POINT('',(-17.5,-1.,44.6)) ;
#46270 = CARTESIAN_POINT('Origin',(-17.5,-1.,43.5)) ;
#46271 = CARTESIAN_POINT('',(-18.,-1.,42.4)) ;
#46272 = CARTESIAN_POINT('',(-18.,-1.,43.5)) ;
#46273 = CARTESIAN_POINT('',(-17.,-1.,42.4)) ;
#46274 = CARTESIAN_POINT('',(-5.25,-1.,42.4)) ;
#46275 = CARTESIAN_POINT('',(-17.,-1.,43.5)) ;
#46276 = CARTESIAN_POINT('Origin',(-18.,0.,43.5)) ;
#46277 = CARTESIAN_POINT('',(-18.,1.,42.4)) ;
#46278 = CARTESIAN_POINT('',(-18.,1.,43.5)) ;
#46279 = CARTESIAN_POINT('',(-18.,0.,42.4)) ;
#46280 = CARTESIAN_POINT('Origin',(-17.5,1.,43.5)) ;
#46281 = CARTESIAN_POINT('',(-17.,1.,42.4)) ;
#46282 = CARTESIAN_POINT('',(-17.,1.,43.5)) ;
#46283 = CARTESIAN_POINT('',(-5.25,1.,42.4)) ;
#46284 = CARTESIAN_POINT('Origin',(-17.,0.,43.5)) ;
#46285 = CARTESIAN_POINT('',(-17.,0.,42.4)) ;
#46286 = CARTESIAN_POINT('Origin',(-11.,-10.,42.4)) ;
#46287 = CARTESIAN_POINT('',(-11.425,-10.,42.)) ;
#46288 = CARTESIAN_POINT('Origin',(-11.,-10.,42.)) ;
#46289 = CARTESIAN_POINT('',(-11.425,-10.,42.8)) ;
#46290 = CARTESIAN_POINT('',(-11.425,-10.,42.4)) ;
#46291 = CARTESIAN_POINT('Origin',(-11.,-10.,42.8)) ;
#46292 = CARTESIAN_POINT('Origin',(-11.,10.,42.4)) ;
#46293 = CARTESIAN_POINT('',(-11.425,10.,42.)) ;
#46294 = CARTESIAN_POINT('Origin',(-11.,10.,42.)) ;
#46295 = CARTESIAN_POINT('',(-11.425,10.,42.8)) ;
#46296 = CARTESIAN_POINT('',(-11.425,10.,42.4)) ;
#46297 = CARTESIAN_POINT('Origin',(-11.,10.,42.8)) ;
#46298 = CARTESIAN_POINT('Origin',(11.,-10.,42.4)) ;
#46299 = CARTESIAN_POINT('',(10.575,-10.,42.)) ;
#46300 = CARTESIAN_POINT('Origin',(11.,-10.,42.)) ;
#46301 = CARTESIAN_POINT('',(10.575,-10.,42.8)) ;
#46302 = CARTESIAN_POINT('',(10.575,-10.,42.4)) ;
#46303 = CARTESIAN_POINT('Origin',(11.,-10.,42.8)) ;
#46304 = CARTESIAN_POINT('Origin',(11.,10.,42.4)) ;
#46305 = CARTESIAN_POINT('',(10.575,10.,42.)) ;
#46306 = CARTESIAN_POINT('Origin',(11.,10.,42.)) ;
#46307 = CARTESIAN_POINT('',(10.575,10.,42.8)) ;
#46308 = CARTESIAN_POINT('',(10.575,10.,42.4)) ;
#46309 = CARTESIAN_POINT('Origin',(11.,10.,42.8)) ;
#46310 = CARTESIAN_POINT('Origin',(7.,7.,42.4)) ;
#46311 = CARTESIAN_POINT('',(5.95,7.,42.)) ;
#46312 = CARTESIAN_POINT('Origin',(7.,7.,42.)) ;
#46313 = CARTESIAN_POINT('',(5.95,7.,42.4)) ;
#46314 = CARTESIAN_POINT('',(5.95,7.,42.4)) ;
#46315 = CARTESIAN_POINT('',(8.03077640640442,7.2,42.4)) ;
#46316 = CARTESIAN_POINT('Origin',(7.,7.,42.4)) ;
#46317 = CARTESIAN_POINT('',(8.03077640640442,7.2,42.8)) ;
#46318 = CARTESIAN_POINT('',(8.03077640640442,7.2,42.4)) ;
#46319 = CARTESIAN_POINT('',(5.96922359359558,7.2,42.8)) ;
#46320 = CARTESIAN_POINT('Origin',(7.,7.,42.8)) ;
#46321 = CARTESIAN_POINT('',(5.96922359359558,7.2,42.4)) ;
#46322 = CARTESIAN_POINT('',(5.96922359359558,7.2,42.4)) ;
#46323 = CARTESIAN_POINT('Origin',(7.,7.,42.4)) ;
#46324 = CARTESIAN_POINT('Origin',(7.,0.,42.4)) ;
#46325 = CARTESIAN_POINT('',(-16.,7.2,42.4)) ;
#46326 = CARTESIAN_POINT('',(3.5,7.2,42.4)) ;
#46327 = CARTESIAN_POINT('',(-16.,12.,42.4)) ;
#46328 = CARTESIAN_POINT('',(-16.,4.8,42.4)) ;
#46329 = CARTESIAN_POINT('',(-20.,12.,42.4)) ;
#46330 = CARTESIAN_POINT('',(7.,12.,42.4)) ;
#46331 = CARTESIAN_POINT('',(-20.,-12.,42.4)) ;
#46332 = CARTESIAN_POINT('',(-20.,0.,42.4)) ;
#46333 = CARTESIAN_POINT('',(-16.,-12.,42.4)) ;
#46334 = CARTESIAN_POINT('',(7.,-12.,42.4)) ;
#46335 = CARTESIAN_POINT('',(-16.,-7.2,42.4)) ;
#46336 = CARTESIAN_POINT('',(-16.,-4.8,42.4)) ;
#46337 = CARTESIAN_POINT('',(-2.19374109684803,-7.2,42.4)) ;
#46338 = CARTESIAN_POINT('',(3.5,-7.2,42.4)) ;
#46339 = CARTESIAN_POINT('',(-1.37550241686044,-6.35279411764706,42.4)) ;
#46340 = CARTESIAN_POINT('Origin',(0.,-8.5,42.4)) ;
#46341 = CARTESIAN_POINT('',(1.37550241686044,-6.35279411764706,42.4)) ;
#46342 = CARTESIAN_POINT('Origin',(0.,0.,42.4)) ;
#46343 = CARTESIAN_POINT('',(2.19374109684803,-7.2,42.4)) ;
#46344 = CARTESIAN_POINT('Origin',(0.,-8.5,42.4)) ;
#46345 = CARTESIAN_POINT('',(16.,-7.2,42.4)) ;
#46346 = CARTESIAN_POINT('',(3.5,-7.2,42.4)) ;
#46347 = CARTESIAN_POINT('',(16.,-12.,42.4)) ;
#46348 = CARTESIAN_POINT('',(16.,-4.8,42.4)) ;
#46349 = CARTESIAN_POINT('',(34.,-12.,42.4)) ;
#46350 = CARTESIAN_POINT('',(7.,-12.,42.4)) ;
#46351 = CARTESIAN_POINT('',(34.,12.,42.4)) ;
#46352 = CARTESIAN_POINT('',(34.,0.,42.4)) ;
#46353 = CARTESIAN_POINT('',(16.,12.,42.4)) ;
#46354 = CARTESIAN_POINT('',(7.,12.,42.4)) ;
#46355 = CARTESIAN_POINT('',(16.,7.2,42.4)) ;
#46356 = CARTESIAN_POINT('',(16.,4.8,42.4)) ;
#46357 = CARTESIAN_POINT('',(3.5,7.2,42.4)) ;
#46358 = CARTESIAN_POINT('Origin',(0.,7.2,42.6)) ;
#46359 = CARTESIAN_POINT('',(-16.,7.2,42.8)) ;
#46360 = CARTESIAN_POINT('',(0.,7.2,42.8)) ;
#46361 = CARTESIAN_POINT('',(-16.,7.2,42.6)) ;
#46362 = CARTESIAN_POINT('Origin',(0.,-9.6,42.8)) ;
#46363 = CARTESIAN_POINT('',(2.19374109684803,-7.2,42.8)) ;
#46364 = CARTESIAN_POINT('',(-2.19374109684803,-7.2,42.8)) ;
#46365 = CARTESIAN_POINT('Origin',(0.,-8.5,42.8)) ;
#46366 = CARTESIAN_POINT('',(-16.,-7.2,42.8)) ;
#46367 = CARTESIAN_POINT('',(0.,-7.2,42.8)) ;
#46368 = CARTESIAN_POINT('',(-16.,-12.,42.8)) ;
#46369 = CARTESIAN_POINT('',(-16.,-9.6,42.8)) ;
#46370 = CARTESIAN_POINT('',(16.,-12.,42.8)) ;
#46371 = CARTESIAN_POINT('',(0.,-12.,42.8)) ;
#46372 = CARTESIAN_POINT('',(16.,-7.2,42.8)) ;
#46373 = CARTESIAN_POINT('',(16.,-9.6,42.8)) ;
#46374 = CARTESIAN_POINT('',(0.,-7.2,42.8)) ;
#46375 = CARTESIAN_POINT('Origin',(0.,-7.2,42.6)) ;
#46376 = CARTESIAN_POINT('',(-2.19374109684803,-7.2,42.4)) ;
#46377 = CARTESIAN_POINT('',(-16.,-7.2,42.6)) ;
#46378 = CARTESIAN_POINT('Origin',(-16.,-9.6,42.6)) ;
#46379 = CARTESIAN_POINT('',(-16.,-12.,42.6)) ;
#46380 = CARTESIAN_POINT('Origin',(0.,-7.2,42.6)) ;
#46381 = CARTESIAN_POINT('',(2.19374109684803,-7.2,42.4)) ;
#46382 = CARTESIAN_POINT('',(16.,-7.2,42.6)) ;
#46383 = CARTESIAN_POINT('Origin',(16.,-9.6,42.6)) ;
#46384 = CARTESIAN_POINT('',(16.,-12.,42.6)) ;
#46385 = CARTESIAN_POINT('Origin',(0.,9.6,42.8)) ;
#46386 = CARTESIAN_POINT('',(16.,7.2,42.8)) ;
#46387 = CARTESIAN_POINT('',(0.,7.2,42.8)) ;
#46388 = CARTESIAN_POINT('',(16.,12.,42.8)) ;
#46389 = CARTESIAN_POINT('',(16.,9.6,42.8)) ;
#46390 = CARTESIAN_POINT('',(-16.,12.,42.8)) ;
#46391 = CARTESIAN_POINT('',(0.,12.,42.8)) ;
#46392 = CARTESIAN_POINT('',(-16.,9.6,42.8)) ;
#46393 = CARTESIAN_POINT('Origin',(0.,7.2,42.6)) ;
#46394 = CARTESIAN_POINT('',(16.,7.2,42.6)) ;
#46395 = CARTESIAN_POINT('Origin',(-16.,9.6,42.6)) ;
#46396 = CARTESIAN_POINT('',(-16.,12.,42.6)) ;
#46397 = CARTESIAN_POINT('Origin',(16.,9.6,42.6)) ;
#46398 = CARTESIAN_POINT('',(16.,12.,42.6)) ;
#46399 = CARTESIAN_POINT('Origin',(0.,-8.5,42.2)) ;
#46400 = CARTESIAN_POINT('',(1.37550241686044,-6.35279411764706,42.)) ;
#46401 = CARTESIAN_POINT('',(1.37550241686045,-6.35279411764706,42.2)) ;
#46402 = CARTESIAN_POINT('',(-1.37550241686044,-6.35279411764706,42.)) ;
#46403 = CARTESIAN_POINT('Origin',(0.,-8.5,42.)) ;
#46404 = CARTESIAN_POINT('',(-1.37550241686045,-6.35279411764706,42.2)) ;
#46405 = CARTESIAN_POINT('Origin',(7.,0.,42.)) ;
#46406 = CARTESIAN_POINT('',(34.,12.,42.)) ;
#46407 = CARTESIAN_POINT('',(34.,-12.,42.)) ;
#46408 = CARTESIAN_POINT('',(34.,0.,42.)) ;
#46409 = CARTESIAN_POINT('',(-20.,-12.,42.)) ;
#46410 = CARTESIAN_POINT('',(7.,-12.,42.)) ;
#46411 = CARTESIAN_POINT('',(-20.,12.,42.)) ;
#46412 = CARTESIAN_POINT('',(-20.,0.,42.)) ;
#46413 = CARTESIAN_POINT('',(7.,12.,42.)) ;
#46414 = CARTESIAN_POINT('Origin',(0.,0.,42.)) ;
#46415 = CARTESIAN_POINT('Origin',(0.,0.,42.2)) ;
#46416 = CARTESIAN_POINT('Origin',(7.,-12.,42.2)) ;
#46417 = CARTESIAN_POINT('',(-20.,-12.,42.2)) ;
#46418 = CARTESIAN_POINT('',(34.,-12.,42.2)) ;
#46419 = CARTESIAN_POINT('Origin',(-20.,0.,42.2)) ;
#46420 = CARTESIAN_POINT('',(-20.,12.,42.2)) ;
#46421 = CARTESIAN_POINT('Origin',(7.,12.,42.2)) ;
#46422 = CARTESIAN_POINT('',(34.,12.,42.2)) ;
#46423 = CARTESIAN_POINT('Origin',(34.,0.,42.2)) ;
#46424 = CARTESIAN_POINT('',(0.,0.,0.)) ;
#46425 = CARTESIAN_POINT('Origin',(21.75,6.,42.9)) ;
#46426 = CARTESIAN_POINT('',(20.,6.,42.8)) ;
#46427 = CARTESIAN_POINT('',(20.,6.,43.)) ;
#46428 = CARTESIAN_POINT('',(20.,6.,42.9)) ;
#46429 = CARTESIAN_POINT('',(24.5,6.,42.8)) ;
#46430 = CARTESIAN_POINT('',(21.75,6.,42.8)) ;
#46431 = CARTESIAN_POINT('',(24.5,6.,43.)) ;
#46432 = CARTESIAN_POINT('',(24.5,6.,42.9)) ;
#46433 = CARTESIAN_POINT('',(21.75,6.,43.)) ;
#46434 = CARTESIAN_POINT('Origin',(24.5,6.6,42.9)) ;
#46435 = CARTESIAN_POINT('',(24.5,7.2,42.8)) ;
#46436 = CARTESIAN_POINT('',(24.5,6.6,42.8)) ;
#46437 = CARTESIAN_POINT('',(24.5,7.2,43.)) ;
#46438 = CARTESIAN_POINT('',(24.5,7.2,42.9)) ;
#46439 = CARTESIAN_POINT('',(24.5,6.6,43.)) ;
#46440 = CARTESIAN_POINT('Origin',(19.5,5.6,43.)) ;
#46441 = CARTESIAN_POINT('',(19.,7.2,43.)) ;
#46442 = CARTESIAN_POINT('',(19.,4.,43.)) ;
#46443 = CARTESIAN_POINT('',(19.,5.6,43.)) ;
#46444 = CARTESIAN_POINT('',(20.,4.,43.)) ;
#46445 = CARTESIAN_POINT('',(19.5,4.,43.)) ;
#46446 = CARTESIAN_POINT('',(20.,5.6,43.)) ;
#46447 = CARTESIAN_POINT('',(19.5,7.2,43.)) ;
#46448 = CARTESIAN_POINT('Origin',(19.,5.6,42.9)) ;
#46449 = CARTESIAN_POINT('',(19.,4.,42.8)) ;
#46450 = CARTESIAN_POINT('',(19.,5.5,42.8)) ;
#46451 = CARTESIAN_POINT('',(19.,2.8,42.8)) ;
#46452 = CARTESIAN_POINT('',(19.,4.,42.9)) ;
#46453 = CARTESIAN_POINT('',(19.,7.2,42.8)) ;
#46454 = CARTESIAN_POINT('',(19.,7.2,42.9)) ;
#46455 = CARTESIAN_POINT('',(19.,5.6,42.8)) ;
#46456 = CARTESIAN_POINT('Origin',(19.5,5.6,42.8)) ;
#46457 = CARTESIAN_POINT('',(20.,5.5,42.8)) ;
#46458 = CARTESIAN_POINT('',(5.,5.5,42.8)) ;
#46459 = CARTESIAN_POINT('',(21.75,7.2,42.8)) ;
#46460 = CARTESIAN_POINT('',(20.,5.6,42.8)) ;
#46461 = CARTESIAN_POINT('Origin',(19.5,4.,42.9)) ;
#46462 = CARTESIAN_POINT('',(20.,4.,42.8)) ;
#46463 = CARTESIAN_POINT('',(12.25,4.,42.8)) ;
#46464 = CARTESIAN_POINT('',(20.,4.,42.9)) ;
#46465 = CARTESIAN_POINT('Origin',(19.5,7.2,42.9)) ;
#46466 = CARTESIAN_POINT('Origin',(21.5,0.,42.6)) ;
#46467 = CARTESIAN_POINT('',(21.25,-3.06161699786838E-17,42.4)) ;
#46468 = CARTESIAN_POINT('Origin',(21.5,0.,42.4)) ;
#46469 = CARTESIAN_POINT('',(21.25,3.06161699786838E-17,42.8)) ;
#46470 = CARTESIAN_POINT('',(21.25,-3.06161699786838E-17,42.6)) ;
#46471 = CARTESIAN_POINT('Origin',(21.5,0.,42.8)) ;
#46472 = CARTESIAN_POINT('Origin',(21.25,-1.5,42.6)) ;
#46473 = CARTESIAN_POINT('',(20.,-1.5,42.4)) ;
#46474 = CARTESIAN_POINT('',(20.,-1.5,42.8)) ;
#46475 = CARTESIAN_POINT('',(20.,-1.5,42.6)) ;
#46476 = CARTESIAN_POINT('',(22.5,-1.5,42.4)) ;
#46477 = CARTESIAN_POINT('',(21.25,-1.5,42.4)) ;
#46478 = CARTESIAN_POINT('',(22.5,-1.5,42.8)) ;
#46479 = CARTESIAN_POINT('',(22.5,-1.5,42.6)) ;
#46480 = CARTESIAN_POINT('',(21.25,-1.5,42.8)) ;
#46481 = CARTESIAN_POINT('Origin',(21.25,1.5,42.6)) ;
#46482 = CARTESIAN_POINT('',(22.5,1.5,42.8)) ;
#46483 = CARTESIAN_POINT('',(22.5,1.5,42.4)) ;
#46484 = CARTESIAN_POINT('',(22.5,1.5,42.6)) ;
#46485 = CARTESIAN_POINT('',(20.,1.5,42.4)) ;
#46486 = CARTESIAN_POINT('',(21.25,1.5,42.4)) ;
#46487 = CARTESIAN_POINT('',(20.,1.5,42.8)) ;
#46488 = CARTESIAN_POINT('',(20.,1.5,42.6)) ;
#46489 = CARTESIAN_POINT('',(21.25,1.5,42.8)) ;
#46490 = CARTESIAN_POINT('Origin',(22.5,0.,42.6)) ;
#46491 = CARTESIAN_POINT('',(22.5,0.,42.4)) ;
#46492 = CARTESIAN_POINT('',(22.5,0.,42.8)) ;
#46493 = CARTESIAN_POINT('Origin',(20.,0.,42.6)) ;
#46494 = CARTESIAN_POINT('',(20.,-5.5,42.8)) ;
#46495 = CARTESIAN_POINT('',(20.,0.,42.8)) ;
#46496 = CARTESIAN_POINT('',(20.,-5.5,42.4)) ;
#46497 = CARTESIAN_POINT('',(20.,-5.5,42.6)) ;
#46498 = CARTESIAN_POINT('',(20.,0.,42.4)) ;
#46499 = CARTESIAN_POINT('Origin',(20.,0.,42.6)) ;
#46500 = CARTESIAN_POINT('',(20.,5.5,42.4)) ;
#46501 = CARTESIAN_POINT('',(20.,0.,42.4)) ;
#46502 = CARTESIAN_POINT('',(20.,5.5,42.6)) ;
#46503 = CARTESIAN_POINT('',(20.,0.,42.8)) ;
#46504 = CARTESIAN_POINT('Origin',(-13.,0.,42.6)) ;
#46505 = CARTESIAN_POINT('',(-13.3,-3.67394039744206E-17,42.4)) ;
#46506 = CARTESIAN_POINT('Origin',(-13.,0.,42.4)) ;
#46507 = CARTESIAN_POINT('',(-13.3,3.67394039744206E-17,42.8)) ;
#46508 = CARTESIAN_POINT('',(-13.3,-3.67394039744206E-17,42.6)) ;
#46509 = CARTESIAN_POINT('Origin',(-13.,0.,42.8)) ;
#46510 = CARTESIAN_POINT('Origin',(-12.,-1.5,42.6)) ;
#46511 = CARTESIAN_POINT('',(-14.,-1.5,42.8)) ;
#46512 = CARTESIAN_POINT('',(-14.,-1.5,42.4)) ;
#46513 = CARTESIAN_POINT('',(-14.,-1.5,42.6)) ;
#46514 = CARTESIAN_POINT('',(-10.,-1.5,42.4)) ;
#46515 = CARTESIAN_POINT('',(-12.,-1.5,42.4)) ;
#46516 = CARTESIAN_POINT('',(-10.,-1.5,42.8)) ;
#46517 = CARTESIAN_POINT('',(-10.,-1.5,42.6)) ;
#46518 = CARTESIAN_POINT('',(-12.,-1.5,42.8)) ;
#46519 = CARTESIAN_POINT('Origin',(-14.,0.,42.6)) ;
#46520 = CARTESIAN_POINT('',(-14.,1.5,42.8)) ;
#46521 = CARTESIAN_POINT('',(-14.,1.5,42.4)) ;
#46522 = CARTESIAN_POINT('',(-14.,1.5,42.6)) ;
#46523 = CARTESIAN_POINT('',(-14.,0.,42.4)) ;
#46524 = CARTESIAN_POINT('',(-14.,0.,42.8)) ;
#46525 = CARTESIAN_POINT('Origin',(-12.,1.5,42.6)) ;
#46526 = CARTESIAN_POINT('',(-10.,1.5,42.4)) ;
#46527 = CARTESIAN_POINT('',(-10.,1.5,42.8)) ;
#46528 = CARTESIAN_POINT('',(-10.,1.5,42.6)) ;
#46529 = CARTESIAN_POINT('',(-12.,1.5,42.4)) ;
#46530 = CARTESIAN_POINT('',(-12.,1.5,42.8)) ;
#46531 = CARTESIAN_POINT('Origin',(-10.,0.,42.6)) ;
#46532 = CARTESIAN_POINT('',(-10.,5.5,42.8)) ;
#46533 = CARTESIAN_POINT('',(-10.,0.,42.8)) ;
#46534 = CARTESIAN_POINT('',(-10.,5.5,42.4)) ;
#46535 = CARTESIAN_POINT('',(-10.,5.5,42.6)) ;
#46536 = CARTESIAN_POINT('',(-10.,0.,42.4)) ;
#46537 = CARTESIAN_POINT('Origin',(-10.,0.,42.6)) ;
#46538 = CARTESIAN_POINT('',(-10.,-5.5,42.4)) ;
#46539 = CARTESIAN_POINT('',(-10.,0.,42.4)) ;
#46540 = CARTESIAN_POINT('',(-10.,-5.5,42.8)) ;
#46541 = CARTESIAN_POINT('',(-10.,-5.5,42.6)) ;
#46542 = CARTESIAN_POINT('',(-10.,0.,42.8)) ;
#46543 = CARTESIAN_POINT('Origin',(15.,0.,42.6)) ;
#46544 = CARTESIAN_POINT('',(10.5,-5.51091059616309E-16,42.4)) ;
#46545 = CARTESIAN_POINT('Origin',(15.,0.,42.4)) ;
#46546 = CARTESIAN_POINT('',(10.5,5.51091059616309E-16,42.8)) ;
#46547 = CARTESIAN_POINT('',(10.5,-5.51091059616309E-16,42.6)) ;
#46548 = CARTESIAN_POINT('Origin',(15.,0.,42.8)) ;
#46549 = CARTESIAN_POINT('Origin',(5.,0.,42.8)) ;
#46550 = CARTESIAN_POINT('',(5.,5.5,42.8)) ;
#46551 = CARTESIAN_POINT('',(5.,-5.5,42.8)) ;
#46552 = CARTESIAN_POINT('Origin',(5.,0.,42.4)) ;
#46553 = CARTESIAN_POINT('',(5.,-5.5,42.4)) ;
#46554 = CARTESIAN_POINT('',(5.,5.5,42.4)) ;
#46555 = CARTESIAN_POINT('Origin',(5.,-5.5,42.6)) ;
#46556 = CARTESIAN_POINT('Origin',(5.,5.5,42.6)) ;
#46557 = CARTESIAN_POINT('',(0.,0.,0.)) ;
#46558 = CARTESIAN_POINT('Origin',(24.2,6.35,42.5)) ;
#46559 = CARTESIAN_POINT('',(24.3,6.,42.5)) ;
#46560 = CARTESIAN_POINT('',(24.1,6.,42.5)) ;
#46561 = CARTESIAN_POINT('',(22.35,6.,42.5)) ;
#46562 = CARTESIAN_POINT('',(24.3,6.8,42.5)) ;
#46563 = CARTESIAN_POINT('',(24.3,6.35,42.5)) ;
#46564 = CARTESIAN_POINT('',(24.1,6.8,42.5)) ;
#46565 = CARTESIAN_POINT('',(24.2,6.8,42.5)) ;
#46566 = CARTESIAN_POINT('',(24.1,6.35,42.5)) ;
#46567 = CARTESIAN_POINT('Origin',(24.1,6.35,42.6)) ;
#46568 = CARTESIAN_POINT('',(24.1,6.,42.6)) ;
#46569 = CARTESIAN_POINT('',(24.1,6.,42.55)) ;
#46570 = CARTESIAN_POINT('',(24.1,6.8,42.6)) ;
#46571 = CARTESIAN_POINT('',(24.1,6.8,42.6)) ;
#46572 = CARTESIAN_POINT('',(24.1,6.475,42.6)) ;
#46573 = CARTESIAN_POINT('Origin',(24.2,6.8,42.6)) ;
#46574 = CARTESIAN_POINT('',(24.3,6.8,42.6)) ;
#46575 = CARTESIAN_POINT('',(22.35,6.8,42.6)) ;
#46576 = CARTESIAN_POINT('',(24.3,6.8,42.6)) ;
#46577 = CARTESIAN_POINT('Origin',(24.3,6.35,42.6)) ;
#46578 = CARTESIAN_POINT('',(24.3,6.,42.6)) ;
#46579 = CARTESIAN_POINT('',(24.3,6.,42.55)) ;
#46580 = CARTESIAN_POINT('',(24.3,6.475,42.6)) ;
#46581 = CARTESIAN_POINT('Origin',(20.5,6.,42.5)) ;
#46582 = CARTESIAN_POINT('',(23.4,6.,42.6)) ;
#46583 = CARTESIAN_POINT('',(20.5,6.,42.6)) ;
#46584 = CARTESIAN_POINT('',(23.4,6.,42.5)) ;
#46585 = CARTESIAN_POINT('',(23.4,6.,42.55)) ;
#46586 = CARTESIAN_POINT('',(23.2,6.,42.5)) ;
#46587 = CARTESIAN_POINT('',(21.9,6.,42.5)) ;
#46588 = CARTESIAN_POINT('',(23.2,6.,42.6)) ;
#46589 = CARTESIAN_POINT('',(23.2,6.,42.55)) ;
#46590 = CARTESIAN_POINT('',(22.5,6.,42.6)) ;
#46591 = CARTESIAN_POINT('',(20.5,6.,42.6)) ;
#46592 = CARTESIAN_POINT('',(22.5,6.,42.5)) ;
#46593 = CARTESIAN_POINT('',(22.5,6.,42.55)) ;
#46594 = CARTESIAN_POINT('',(22.3,6.,42.5)) ;
#46595 = CARTESIAN_POINT('',(21.45,6.,42.5)) ;
#46596 = CARTESIAN_POINT('',(22.3,6.,42.6)) ;
#46597 = CARTESIAN_POINT('',(22.3,6.,42.55)) ;
#46598 = CARTESIAN_POINT('',(21.6,6.,42.6)) ;
#46599 = CARTESIAN_POINT('',(20.5,6.,42.6)) ;
#46600 = CARTESIAN_POINT('',(21.6,6.,42.5)) ;
#46601 = CARTESIAN_POINT('',(21.6,6.,42.55)) ;
#46602 = CARTESIAN_POINT('',(21.4,6.,42.5)) ;
#46603 = CARTESIAN_POINT('',(21.,6.,42.5)) ;
#46604 = CARTESIAN_POINT('',(21.4,6.,42.6)) ;
#46605 = CARTESIAN_POINT('',(21.4,6.,42.55)) ;
#46606 = CARTESIAN_POINT('',(20.7,6.,42.6)) ;
#46607 = CARTESIAN_POINT('',(20.5,6.,42.6)) ;
#46608 = CARTESIAN_POINT('',(20.7,6.,42.5)) ;
#46609 = CARTESIAN_POINT('',(20.7,6.,42.55)) ;
#46610 = CARTESIAN_POINT('',(20.5,6.,42.5)) ;
#46611 = CARTESIAN_POINT('',(20.55,6.,42.5)) ;
#46612 = CARTESIAN_POINT('',(20.5,6.,42.6)) ;
#46613 = CARTESIAN_POINT('',(20.5,6.,42.55)) ;
#46614 = CARTESIAN_POINT('',(19.8,6.,42.6)) ;
#46615 = CARTESIAN_POINT('',(20.5,6.,42.6)) ;
#46616 = CARTESIAN_POINT('',(19.8,6.,42.5)) ;
#46617 = CARTESIAN_POINT('',(19.8,6.,42.55)) ;
#46618 = CARTESIAN_POINT('',(19.6,6.,42.5)) ;
#46619 = CARTESIAN_POINT('',(20.1,6.,42.5)) ;
#46620 = CARTESIAN_POINT('',(19.6,6.,42.6)) ;
#46621 = CARTESIAN_POINT('',(19.6,6.,42.55)) ;
#46622 = CARTESIAN_POINT('',(18.9,6.,42.6)) ;
#46623 = CARTESIAN_POINT('',(20.5,6.,42.6)) ;
#46624 = CARTESIAN_POINT('',(18.9,6.,42.5)) ;
#46625 = CARTESIAN_POINT('',(18.9,6.,42.55)) ;
#46626 = CARTESIAN_POINT('',(18.7,6.,42.5)) ;
#46627 = CARTESIAN_POINT('',(19.65,6.,42.5)) ;
#46628 = CARTESIAN_POINT('',(18.7,6.,42.6)) ;
#46629 = CARTESIAN_POINT('',(18.7,6.,42.55)) ;
#46630 = CARTESIAN_POINT('',(18.,6.,42.6)) ;
#46631 = CARTESIAN_POINT('',(20.5,6.,42.6)) ;
#46632 = CARTESIAN_POINT('',(18.,6.,42.5)) ;
#46633 = CARTESIAN_POINT('',(18.,6.,42.55)) ;
#46634 = CARTESIAN_POINT('',(17.8,6.,42.5)) ;
#46635 = CARTESIAN_POINT('',(19.2,6.,42.5)) ;
#46636 = CARTESIAN_POINT('',(17.8,6.,42.6)) ;
#46637 = CARTESIAN_POINT('',(17.8,6.,42.55)) ;
#46638 = CARTESIAN_POINT('',(17.1,6.,42.6)) ;
#46639 = CARTESIAN_POINT('',(20.5,6.,42.6)) ;
#46640 = CARTESIAN_POINT('',(17.1,6.,42.5)) ;
#46641 = CARTESIAN_POINT('',(17.1,6.,42.55)) ;
#46642 = CARTESIAN_POINT('',(16.9,6.,42.5)) ;
#46643 = CARTESIAN_POINT('',(18.75,6.,42.5)) ;
#46644 = CARTESIAN_POINT('',(16.9,6.,42.6)) ;
#46645 = CARTESIAN_POINT('',(16.9,6.,42.55)) ;
#46646 = CARTESIAN_POINT('',(16.5,6.,42.6)) ;
#46647 = CARTESIAN_POINT('',(20.5,6.,42.6)) ;
#46648 = CARTESIAN_POINT('',(16.5,6.,42.4)) ;
#46649 = CARTESIAN_POINT('',(16.5,6.,42.5)) ;
#46650 = CARTESIAN_POINT('',(24.5,6.,42.4)) ;
#46651 = CARTESIAN_POINT('',(20.5,6.,42.4)) ;
#46652 = CARTESIAN_POINT('',(24.5,6.,42.6)) ;
#46653 = CARTESIAN_POINT('',(24.5,6.,42.5)) ;
#46654 = CARTESIAN_POINT('',(20.5,6.,42.6)) ;
#46655 = CARTESIAN_POINT('Origin',(23.3,6.8,42.6)) ;
#46656 = CARTESIAN_POINT('',(23.2,6.8,42.6)) ;
#46657 = CARTESIAN_POINT('',(23.4,6.8,42.6)) ;
#46658 = CARTESIAN_POINT('',(21.9,6.8,42.6)) ;
#46659 = CARTESIAN_POINT('',(23.2,6.8,42.5)) ;
#46660 = CARTESIAN_POINT('',(23.2,6.8,42.6)) ;
#46661 = CARTESIAN_POINT('',(23.4,6.8,42.5)) ;
#46662 = CARTESIAN_POINT('',(23.3,6.8,42.5)) ;
#46663 = CARTESIAN_POINT('',(23.4,6.8,42.6)) ;
#46664 = CARTESIAN_POINT('Origin',(23.4,6.35,42.6)) ;
#46665 = CARTESIAN_POINT('',(23.4,6.475,42.6)) ;
#46666 = CARTESIAN_POINT('',(23.4,6.35,42.5)) ;
#46667 = CARTESIAN_POINT('Origin',(23.3,6.35,42.5)) ;
#46668 = CARTESIAN_POINT('',(23.2,6.35,42.5)) ;
#46669 = CARTESIAN_POINT('Origin',(23.2,6.35,42.6)) ;
#46670 = CARTESIAN_POINT('',(23.2,6.475,42.6)) ;
#46671 = CARTESIAN_POINT('Origin',(20.5,6.6,42.6)) ;
#46672 = CARTESIAN_POINT('',(24.5,7.2,42.6)) ;
#46673 = CARTESIAN_POINT('',(24.5,6.6,42.6)) ;
#46674 = CARTESIAN_POINT('',(16.5,7.2,42.6)) ;
#46675 = CARTESIAN_POINT('',(20.5,7.2,42.6)) ;
#46676 = CARTESIAN_POINT('',(16.5,6.6,42.6)) ;
#46677 = CARTESIAN_POINT('',(16.9,6.8,42.6)) ;
#46678 = CARTESIAN_POINT('',(16.9,6.475,42.6)) ;
#46679 = CARTESIAN_POINT('',(17.1,6.8,42.6)) ;
#46680 = CARTESIAN_POINT('',(18.75,6.8,42.6)) ;
#46681 = CARTESIAN_POINT('',(17.1,6.475,42.6)) ;
#46682 = CARTESIAN_POINT('',(17.8,6.8,42.6)) ;
#46683 = CARTESIAN_POINT('',(17.8,6.475,42.6)) ;
#46684 = CARTESIAN_POINT('',(18.,6.8,42.6)) ;
#46685 = CARTESIAN_POINT('',(19.2,6.8,42.6)) ;
#46686 = CARTESIAN_POINT('',(18.,6.475,42.6)) ;
#46687 = CARTESIAN_POINT('',(18.7,6.8,42.6)) ;
#46688 = CARTESIAN_POINT('',(18.7,6.475,42.6)) ;
#46689 = CARTESIAN_POINT('',(18.9,6.8,42.6)) ;
#46690 = CARTESIAN_POINT('',(19.65,6.8,42.6)) ;
#46691 = CARTESIAN_POINT('',(18.9,6.475,42.6)) ;
#46692 = CARTESIAN_POINT('',(19.6,6.8,42.6)) ;
#46693 = CARTESIAN_POINT('',(19.6,6.475,42.6)) ;
#46694 = CARTESIAN_POINT('',(19.8,6.8,42.6)) ;
#46695 = CARTESIAN_POINT('',(20.1,6.8,42.6)) ;
#46696 = CARTESIAN_POINT('',(19.8,6.475,42.6)) ;
#46697 = CARTESIAN_POINT('',(20.5,6.8,42.6)) ;
#46698 = CARTESIAN_POINT('',(20.5,6.475,42.6)) ;
#46699 = CARTESIAN_POINT('',(20.7,6.8,42.6)) ;
#46700 = CARTESIAN_POINT('',(20.55,6.8,42.6)) ;
#46701 = CARTESIAN_POINT('',(20.7,6.475,42.6)) ;
#46702 = CARTESIAN_POINT('',(21.4,6.8,42.6)) ;
#46703 = CARTESIAN_POINT('',(21.4,6.475,42.6)) ;
#46704 = CARTESIAN_POINT('',(21.6,6.8,42.6)) ;
#46705 = CARTESIAN_POINT('',(21.,6.8,42.6)) ;
#46706 = CARTESIAN_POINT('',(21.6,6.475,42.6)) ;
#46707 = CARTESIAN_POINT('',(22.3,6.8,42.6)) ;
#46708 = CARTESIAN_POINT('',(22.3,6.475,42.6)) ;
#46709 = CARTESIAN_POINT('',(22.5,6.8,42.6)) ;
#46710 = CARTESIAN_POINT('',(21.45,6.8,42.6)) ;
#46711 = CARTESIAN_POINT('',(22.5,6.475,42.6)) ;
#46712 = CARTESIAN_POINT('Origin',(22.4,6.35,42.5)) ;
#46713 = CARTESIAN_POINT('',(22.5,6.8,42.5)) ;
#46714 = CARTESIAN_POINT('',(22.5,6.35,42.5)) ;
#46715 = CARTESIAN_POINT('',(22.3,6.8,42.5)) ;
#46716 = CARTESIAN_POINT('',(22.4,6.8,42.5)) ;
#46717 = CARTESIAN_POINT('',(22.3,6.35,42.5)) ;
#46718 = CARTESIAN_POINT('Origin',(22.3,6.35,42.6)) ;
#46719 = CARTESIAN_POINT('',(22.3,6.8,42.6)) ;
#46720 = CARTESIAN_POINT('Origin',(22.4,6.8,42.6)) ;
#46721 = CARTESIAN_POINT('',(22.5,6.8,42.6)) ;
#46722 = CARTESIAN_POINT('Origin',(22.5,6.35,42.6)) ;
#46723 = CARTESIAN_POINT('Origin',(21.5,6.8,42.6)) ;
#46724 = CARTESIAN_POINT('',(21.4,6.8,42.5)) ;
#46725 = CARTESIAN_POINT('',(21.4,6.8,42.6)) ;
#46726 = CARTESIAN_POINT('',(21.6,6.8,42.5)) ;
#46727 = CARTESIAN_POINT('',(21.5,6.8,42.5)) ;
#46728 = CARTESIAN_POINT('',(21.6,6.8,42.6)) ;
#46729 = CARTESIAN_POINT('Origin',(21.6,6.35,42.6)) ;
#46730 = CARTESIAN_POINT('',(21.6,6.35,42.5)) ;
#46731 = CARTESIAN_POINT('Origin',(21.5,6.35,42.5)) ;
#46732 = CARTESIAN_POINT('',(21.4,6.35,42.5)) ;
#46733 = CARTESIAN_POINT('Origin',(21.4,6.35,42.6)) ;
#46734 = CARTESIAN_POINT('Origin',(20.6,6.35,42.5)) ;
#46735 = CARTESIAN_POINT('',(20.7,6.8,42.5)) ;
#46736 = CARTESIAN_POINT('',(20.7,6.35,42.5)) ;
#46737 = CARTESIAN_POINT('',(20.5,6.8,42.5)) ;
#46738 = CARTESIAN_POINT('',(20.6,6.8,42.5)) ;
#46739 = CARTESIAN_POINT('',(20.5,6.35,42.5)) ;
#46740 = CARTESIAN_POINT('Origin',(20.5,6.35,42.6)) ;
#46741 = CARTESIAN_POINT('',(20.5,6.8,42.6)) ;
#46742 = CARTESIAN_POINT('Origin',(20.6,6.8,42.6)) ;
#46743 = CARTESIAN_POINT('',(20.7,6.8,42.6)) ;
#46744 = CARTESIAN_POINT('Origin',(20.7,6.35,42.6)) ;
#46745 = CARTESIAN_POINT('Origin',(19.7,6.8,42.6)) ;
#46746 = CARTESIAN_POINT('',(19.6,6.8,42.5)) ;
#46747 = CARTESIAN_POINT('',(19.6,6.8,42.6)) ;
#46748 = CARTESIAN_POINT('',(19.8,6.8,42.5)) ;
#46749 = CARTESIAN_POINT('',(19.7,6.8,42.5)) ;
#46750 = CARTESIAN_POINT('',(19.8,6.8,42.6)) ;
#46751 = CARTESIAN_POINT('Origin',(19.8,6.35,42.6)) ;
#46752 = CARTESIAN_POINT('',(19.8,6.35,42.5)) ;
#46753 = CARTESIAN_POINT('Origin',(19.7,6.35,42.5)) ;
#46754 = CARTESIAN_POINT('',(19.6,6.35,42.5)) ;
#46755 = CARTESIAN_POINT('Origin',(19.6,6.35,42.6)) ;
#46756 = CARTESIAN_POINT('Origin',(18.8,6.35,42.5)) ;
#46757 = CARTESIAN_POINT('',(18.9,6.8,42.5)) ;
#46758 = CARTESIAN_POINT('',(18.9,6.35,42.5)) ;
#46759 = CARTESIAN_POINT('',(18.7,6.8,42.5)) ;
#46760 = CARTESIAN_POINT('',(18.8,6.8,42.5)) ;
#46761 = CARTESIAN_POINT('',(18.7,6.35,42.5)) ;
#46762 = CARTESIAN_POINT('Origin',(18.7,6.35,42.6)) ;
#46763 = CARTESIAN_POINT('',(18.7,6.8,42.6)) ;
#46764 = CARTESIAN_POINT('Origin',(18.8,6.8,42.6)) ;
#46765 = CARTESIAN_POINT('',(18.9,6.8,42.6)) ;
#46766 = CARTESIAN_POINT('Origin',(18.9,6.35,42.6)) ;
#46767 = CARTESIAN_POINT('Origin',(17.9,6.8,42.6)) ;
#46768 = CARTESIAN_POINT('',(17.8,6.8,42.5)) ;
#46769 = CARTESIAN_POINT('',(17.8,6.8,42.6)) ;
#46770 = CARTESIAN_POINT('',(18.,6.8,42.5)) ;
#46771 = CARTESIAN_POINT('',(17.9,6.8,42.5)) ;
#46772 = CARTESIAN_POINT('',(18.,6.8,42.6)) ;
#46773 = CARTESIAN_POINT('Origin',(18.,6.35,42.6)) ;
#46774 = CARTESIAN_POINT('',(18.,6.35,42.5)) ;
#46775 = CARTESIAN_POINT('Origin',(17.9,6.35,42.5)) ;
#46776 = CARTESIAN_POINT('',(17.8,6.35,42.5)) ;
#46777 = CARTESIAN_POINT('Origin',(17.8,6.35,42.6)) ;
#46778 = CARTESIAN_POINT('Origin',(17.,6.35,42.5)) ;
#46779 = CARTESIAN_POINT('',(17.1,6.8,42.5)) ;
#46780 = CARTESIAN_POINT('',(17.1,6.35,42.5)) ;
#46781 = CARTESIAN_POINT('',(16.9,6.8,42.5)) ;
#46782 = CARTESIAN_POINT('',(17.,6.8,42.5)) ;
#46783 = CARTESIAN_POINT('',(16.9,6.35,42.5)) ;
#46784 = CARTESIAN_POINT('Origin',(16.9,6.35,42.6)) ;
#46785 = CARTESIAN_POINT('',(16.9,6.8,42.6)) ;
#46786 = CARTESIAN_POINT('Origin',(17.,6.8,42.6)) ;
#46787 = CARTESIAN_POINT('',(17.1,6.8,42.6)) ;
#46788 = CARTESIAN_POINT('Origin',(17.1,6.35,42.6)) ;
#46789 = CARTESIAN_POINT('Origin',(20.5,6.6,42.4)) ;
#46790 = CARTESIAN_POINT('',(24.5,7.2,42.4)) ;
#46791 = CARTESIAN_POINT('',(24.5,6.6,42.4)) ;
#46792 = CARTESIAN_POINT('',(16.5,7.2,42.4)) ;
#46793 = CARTESIAN_POINT('',(16.5,6.6,42.4)) ;
#46794 = CARTESIAN_POINT('',(20.5,7.2,42.4)) ;
#46795 = CARTESIAN_POINT('Origin',(16.5,6.6,42.5)) ;
#46796 = CARTESIAN_POINT('',(16.5,7.2,42.5)) ;
#46797 = CARTESIAN_POINT('Origin',(20.5,7.2,42.5)) ;
#46798 = CARTESIAN_POINT('',(24.5,7.2,42.5)) ;
#46799 = CARTESIAN_POINT('Origin',(24.5,6.6,42.5)) ;
#46800 = CARTESIAN_POINT('',(0.,0.,0.)) ;
#46801 = CARTESIAN_POINT('Origin',(-11.,-10.,43.)) ;
#46802 = CARTESIAN_POINT('',(-11.425,-10.,42.8)) ;
#46803 = CARTESIAN_POINT('Origin',(-11.,-10.,42.8)) ;
#46804 = CARTESIAN_POINT('',(-11.425,-10.,43.2)) ;
#46805 = CARTESIAN_POINT('',(-11.425,-10.,43.)) ;
#46806 = CARTESIAN_POINT('Origin',(-11.,-10.,43.2)) ;
#46807 = CARTESIAN_POINT('Origin',(-11.,10.,43.)) ;
#46808 = CARTESIAN_POINT('',(-11.425,10.,42.8)) ;
#46809 = CARTESIAN_POINT('Origin',(-11.,10.,42.8)) ;
#46810 = CARTESIAN_POINT('',(-11.425,10.,43.2)) ;
#46811 = CARTESIAN_POINT('',(-11.425,10.,43.)) ;
#46812 = CARTESIAN_POINT('Origin',(-11.,10.,43.2)) ;
#46813 = CARTESIAN_POINT('Origin',(11.,-10.,43.)) ;
#46814 = CARTESIAN_POINT('',(10.575,-10.,42.8)) ;
#46815 = CARTESIAN_POINT('Origin',(11.,-10.,42.8)) ;
#46816 = CARTESIAN_POINT('',(10.575,-10.,43.2)) ;
#46817 = CARTESIAN_POINT('',(10.575,-10.,43.)) ;
#46818 = CARTESIAN_POINT('Origin',(11.,-10.,43.2)) ;
#46819 = CARTESIAN_POINT('Origin',(11.,10.,43.)) ;
#46820 = CARTESIAN_POINT('',(10.575,10.,42.8)) ;
#46821 = CARTESIAN_POINT('Origin',(11.,10.,42.8)) ;
#46822 = CARTESIAN_POINT('',(10.575,10.,43.2)) ;
#46823 = CARTESIAN_POINT('',(10.575,10.,43.)) ;
#46824 = CARTESIAN_POINT('Origin',(11.,10.,43.2)) ;
#46825 = CARTESIAN_POINT('Origin',(0.,-8.5,45.4)) ;
#46826 = CARTESIAN_POINT('',(0.937723156831554,-6.12867647058824,42.8)) ;
#46827 = CARTESIAN_POINT('',(0.937723156831558,-6.12867647058824,43.2)) ;
#46828 = CARTESIAN_POINT('',(0.937723156831553,-6.12867647058824,45.4)) ;
#46829 = CARTESIAN_POINT('',(-0.937723156831554,-6.12867647058824,42.8)) ;
#46830 = CARTESIAN_POINT('Origin',(0.,-8.5,42.8)) ;
#46831 = CARTESIAN_POINT('',(-0.937723156831558,-6.12867647058824,43.2)) ;
#46832 = CARTESIAN_POINT('',(-0.937723156831553,-6.12867647058824,45.4)) ;
#46833 = CARTESIAN_POINT('Ctrl Pts',(0.937723156831556,-6.12867647058824,
43.2)) ;
#46834 = CARTESIAN_POINT('Ctrl Pts',(1.09784051872832,-6.19199375150714,43.283333711661)) ;
#46835 = CARTESIAN_POINT('Ctrl Pts',(1.24365353256702,-6.26883036968412,43.3825149112026)) ;
#46836 = CARTESIAN_POINT('Ctrl Pts',(1.63123265264399,-6.51561417883593,43.692558910546)) ;
#46837 = CARTESIAN_POINT('Ctrl Pts',(1.86026484716295,-6.73020299859327,43.9504989662474)) ;
#46838 = CARTESIAN_POINT('Ctrl Pts',(2.22065273073428,-7.21102082090391,44.4906901557995)) ;
#46839 = CARTESIAN_POINT('Ctrl Pts',(2.35156592596324,-7.47750307164224,44.7730109630824)) ;
#46840 = CARTESIAN_POINT('Ctrl Pts',(2.48678319602362,-7.9074665870395,45.2057062272756)) ;
#46841 = CARTESIAN_POINT('Ctrl Pts',(2.52462680466552,-8.09269952236317,45.3861655557954)) ;
#46842 = CARTESIAN_POINT('Ctrl Pts',(2.55716495223486,-8.476728138187,45.7477877464213)) ;
#46843 = CARTESIAN_POINT('Ctrl Pts',(2.5518683936729,-8.67551622138784,45.9289578753981)) ;
#46844 = CARTESIAN_POINT('Ctrl Pts',(2.4929255543873,-9.07285134981918,46.2803948513796)) ;
#46845 = CARTESIAN_POINT('Ctrl Pts',(2.43925028674063,-9.27156833359866,46.4508409483682)) ;
#46846 = CARTESIAN_POINT('Ctrl Pts',(2.28306121904059,-9.65450903825491,46.7712289756871)) ;
#46847 = CARTESIAN_POINT('Ctrl Pts',(2.1805386953413,-9.83871335384025,46.9211898465972)) ;
#46848 = CARTESIAN_POINT('Ctrl Pts',(1.94718064660289,-10.1567267690656,47.1751631349221)) ;
#46849 = CARTESIAN_POINT('Ctrl Pts',(1.80829195391443,-10.3103948601966,47.2955507638619)) ;
#46850 = CARTESIAN_POINT('Ctrl Pts',(1.48448994480638,-10.5841638269278,47.5067752387865)) ;
#46851 = CARTESIAN_POINT('Ctrl Pts',(1.29928018215051,-10.7039696130829,47.5975398933414)) ;
#46852 = CARTESIAN_POINT('Ctrl Pts',(0.954201226528961,-10.8712714438875,
47.7233432510296)) ;
#46853 = CARTESIAN_POINT('Ctrl Pts',(0.770006896249385,-10.9389661797779,
47.7737387327547)) ;
#46854 = CARTESIAN_POINT('Ctrl Pts',(0.38547380902765,-11.0284138479361,47.8400994317072)) ;
#46855 = CARTESIAN_POINT('Ctrl Pts',(0.1850851223722,-11.05,47.856)) ;
#46856 = CARTESIAN_POINT('Ctrl Pts',(-0.1850851223722,-11.05,47.856)) ;
#46857 = CARTESIAN_POINT('Ctrl Pts',(-0.38547380902765,-11.0284138479361,
47.8400994317072)) ;
#46858 = CARTESIAN_POINT('Ctrl Pts',(-0.770006896249385,-10.9389661797779,
47.7737387327547)) ;
#46859 = CARTESIAN_POINT('Ctrl Pts',(-0.954201226528961,-10.8712714438875,
47.7233432510296)) ;
#46860 = CARTESIAN_POINT('Ctrl Pts',(-1.29928018215051,-10.7039696130829,
47.5975398933414)) ;
#46861 = CARTESIAN_POINT('Ctrl Pts',(-1.48448994480638,-10.5841638269278,
47.5067752387865)) ;
#46862 = CARTESIAN_POINT('Ctrl Pts',(-1.80829195391443,-10.3103948601966,
47.2955507638619)) ;
#46863 = CARTESIAN_POINT('Ctrl Pts',(-1.94718064660289,-10.1567267690656,
47.1751631349221)) ;
#46864 = CARTESIAN_POINT('Ctrl Pts',(-2.1805386953413,-9.83871335384025,46.9211898465972)) ;
#46865 = CARTESIAN_POINT('Ctrl Pts',(-2.28306121904059,-9.65450903825491,
46.7712289756871)) ;
#46866 = CARTESIAN_POINT('Ctrl Pts',(-2.43925028674063,-9.27156833359864,
46.4508409483682)) ;
#46867 = CARTESIAN_POINT('Ctrl Pts',(-2.4929255543873,-9.07285134981916,46.2803948513796)) ;
#46868 = CARTESIAN_POINT('Ctrl Pts',(-2.5518683936729,-8.67551622138783,45.9289578753981)) ;
#46869 = CARTESIAN_POINT('Ctrl Pts',(-2.55716495223486,-8.47672813818699,
45.7477877464213)) ;
#46870 = CARTESIAN_POINT('Ctrl Pts',(-2.52462680466552,-8.09269952236317,
45.3861655557954)) ;
#46871 = CARTESIAN_POINT('Ctrl Pts',(-2.48678319602362,-7.9074665870395,45.2057062272756)) ;
#46872 = CARTESIAN_POINT('Ctrl Pts',(-2.43254496361321,-7.735,45.0321438835623)) ;
#46873 = CARTESIAN_POINT('Ctrl Pts',(-2.35156592596324,-7.47750307164224,
44.7730109630824)) ;
#46874 = CARTESIAN_POINT('Ctrl Pts',(-2.22065273073428,-7.21102082090391,
44.4906901557995)) ;
#46875 = CARTESIAN_POINT('Ctrl Pts',(-1.86026484716295,-6.73020299859328,
43.9504989662474)) ;
#46876 = CARTESIAN_POINT('Ctrl Pts',(-1.63123265264399,-6.51561417883593,
43.692558910546)) ;
#46877 = CARTESIAN_POINT('Ctrl Pts',(-1.24365353116831,-6.26883036879351,
43.3825149100837)) ;
#46878 = CARTESIAN_POINT('Ctrl Pts',(-1.0978405215343,-6.19199375261675,43.2833337131214)) ;
#46879 = CARTESIAN_POINT('Ctrl Pts',(-0.937723156831557,-6.12867647058824,
43.2)) ;
#46880 = CARTESIAN_POINT('',(1.37550241686044,-6.35279411764706,43.2)) ;
#46881 = CARTESIAN_POINT('',(-1.37550241686044,-6.35279411764706,43.2)) ;
#46882 = CARTESIAN_POINT('Origin',(0.,-8.5,43.2)) ;
#46883 = CARTESIAN_POINT('Ctrl Pts',(-1.37550241686045,-6.35279411764706,
43.2)) ;
#46884 = CARTESIAN_POINT('Ctrl Pts',(-1.63469354395804,-6.51883223475618,
43.4084416977862)) ;
#46885 = CARTESIAN_POINT('Ctrl Pts',(-1.86162214059867,-6.73201385546098,
43.6645334351878)) ;
#46886 = CARTESIAN_POINT('Ctrl Pts',(-2.22065273073428,-7.21102082090391,
44.2026901557995)) ;
#46887 = CARTESIAN_POINT('Ctrl Pts',(-2.35156592596324,-7.47750307164224,
44.4850109630824)) ;
#46888 = CARTESIAN_POINT('Ctrl Pts',(-2.43254496361321,-7.735,44.7441438835623)) ;
#46889 = CARTESIAN_POINT('Ctrl Pts',(-2.48678319602362,-7.9074665870395,44.9177062272756)) ;
#46890 = CARTESIAN_POINT('Ctrl Pts',(-2.52462680466552,-8.09269952236319,
45.0981655557954)) ;
#46891 = CARTESIAN_POINT('Ctrl Pts',(-2.55716495223486,-8.47672813818701,
45.4597877464213)) ;
#46892 = CARTESIAN_POINT('Ctrl Pts',(-2.5518683936729,-8.67551622138784,45.6409578753981)) ;
#46893 = CARTESIAN_POINT('Ctrl Pts',(-2.4929255543873,-9.07285134981917,45.9923948513796)) ;
#46894 = CARTESIAN_POINT('Ctrl Pts',(-2.43925028674063,-9.27156833359865,
46.1628409483682)) ;
#46895 = CARTESIAN_POINT('Ctrl Pts',(-2.28306121904059,-9.65450903825491,
46.4832289756871)) ;
#46896 = CARTESIAN_POINT('Ctrl Pts',(-2.1805386953413,-9.83871335384025,46.6331898465971)) ;
#46897 = CARTESIAN_POINT('Ctrl Pts',(-1.94718064660289,-10.1567267690656,
46.8871631349221)) ;
#46898 = CARTESIAN_POINT('Ctrl Pts',(-1.80829195391443,-10.3103948601966,
47.0075507638619)) ;
#46899 = CARTESIAN_POINT('Ctrl Pts',(-1.48448994480638,-10.5841638269278,
47.2187752387865)) ;
#46900 = CARTESIAN_POINT('Ctrl Pts',(-1.29928018215051,-10.7039696130829,
47.3095398933415)) ;
#46901 = CARTESIAN_POINT('Ctrl Pts',(-0.954201226528961,-10.8712714438875,
47.4353432510296)) ;
#46902 = CARTESIAN_POINT('Ctrl Pts',(-0.770006896249383,-10.9389661797779,
47.4857387327547)) ;
#46903 = CARTESIAN_POINT('Ctrl Pts',(-0.385473809027648,-11.0284138479361,
47.5520994317072)) ;
#46904 = CARTESIAN_POINT('Ctrl Pts',(-0.185085122372201,-11.05,47.568)) ;
#46905 = CARTESIAN_POINT('Ctrl Pts',(0.1850851223722,-11.05,47.568)) ;
#46906 = CARTESIAN_POINT('Ctrl Pts',(0.385473809027648,-11.0284138479361,
47.5520994317072)) ;
#46907 = CARTESIAN_POINT('Ctrl Pts',(0.770006896249383,-10.9389661797779,
47.4857387327547)) ;
#46908 = CARTESIAN_POINT('Ctrl Pts',(0.95420122652896,-10.8712714438875,47.4353432510296)) ;
#46909 = CARTESIAN_POINT('Ctrl Pts',(1.29928018215051,-10.7039696130829,47.3095398933415)) ;
#46910 = CARTESIAN_POINT('Ctrl Pts',(1.48448994480638,-10.5841638269278,47.2187752387865)) ;
#46911 = CARTESIAN_POINT('Ctrl Pts',(1.80829195391443,-10.3103948601966,47.0075507638619)) ;
#46912 = CARTESIAN_POINT('Ctrl Pts',(1.94718064660289,-10.1567267690656,46.8871631349221)) ;
#46913 = CARTESIAN_POINT('Ctrl Pts',(2.1805386953413,-9.83871335384025,46.6331898465971)) ;
#46914 = CARTESIAN_POINT('Ctrl Pts',(2.28306121904059,-9.6545090382549,46.4832289756871)) ;
#46915 = CARTESIAN_POINT('Ctrl Pts',(2.43925028674063,-9.27156833359865,46.1628409483682)) ;
#46916 = CARTESIAN_POINT('Ctrl Pts',(2.4929255543873,-9.07285134981917,45.9923948513796)) ;
#46917 = CARTESIAN_POINT('Ctrl Pts',(2.5518683936729,-8.67551622138783,45.6409578753981)) ;
#46918 = CARTESIAN_POINT('Ctrl Pts',(2.55716495223486,-8.47672813818701,45.4597877464213)) ;
#46919 = CARTESIAN_POINT('Ctrl Pts',(2.52462680466552,-8.09269952236319,45.0981655557954)) ;
#46920 = CARTESIAN_POINT('Ctrl Pts',(2.48678319602362,-7.9074665870395,44.9177062272756)) ;
#46921 = CARTESIAN_POINT('Ctrl Pts',(2.35156592596324,-7.47750307164224,44.4850109630824)) ;
#46922 = CARTESIAN_POINT('Ctrl Pts',(2.22065273073428,-7.21102082090391,44.2026901557995)) ;
#46923 = CARTESIAN_POINT('Ctrl Pts',(1.86162214059868,-6.73201385546098,43.6645334351878)) ;
#46924 = CARTESIAN_POINT('Ctrl Pts',(1.63469354395804,-6.51883223475618,43.4084416977862)) ;
#46925 = CARTESIAN_POINT('Ctrl Pts',(1.37550241686045,-6.35279411764706,43.2)) ;
#46926 = CARTESIAN_POINT('Origin',(0.,0.,42.8)) ;
#46927 = CARTESIAN_POINT('',(12.,12.,42.8)) ;
#46928 = CARTESIAN_POINT('',(12.,-12.,42.8)) ;
#46929 = CARTESIAN_POINT('',(12.,0.,42.8)) ;
#46930 = CARTESIAN_POINT('',(-12.,-12.,42.8)) ;
#46931 = CARTESIAN_POINT('',(0.,-12.,42.8)) ;
#46932 = CARTESIAN_POINT('',(-12.,12.,42.8)) ;
#46933 = CARTESIAN_POINT('',(-12.,0.,42.8)) ;
#46934 = CARTESIAN_POINT('',(0.,12.,42.8)) ;
#46935 = CARTESIAN_POINT('Origin',(0.,0.,42.8)) ;
#46936 = CARTESIAN_POINT('Origin',(0.,0.,43.)) ;
#46937 = CARTESIAN_POINT('',(-6.2,-7.59281015471359E-16,43.2)) ;
#46938 = CARTESIAN_POINT('Origin',(0.,0.,43.2)) ;
#46939 = CARTESIAN_POINT('Origin',(0.,0.,43.2)) ;
#46940 = CARTESIAN_POINT('Origin',(0.,0.,45.6)) ;
#46941 = CARTESIAN_POINT('',(-11.5,-1.40834381901946E-15,48.)) ;
#46942 = CARTESIAN_POINT('Origin',(0.,0.,48.)) ;
#46943 = CARTESIAN_POINT('',(-6.5,-7.9602041944578E-16,43.2)) ;
#46944 = CARTESIAN_POINT('',(-9.,-1.10218211923262E-15,45.6)) ;
#46945 = CARTESIAN_POINT('Origin',(0.,0.,43.2)) ;
#46946 = CARTESIAN_POINT('Origin',(0.,0.,43.2)) ;
#46947 = CARTESIAN_POINT('Origin',(0.,0.,43.2)) ;
#46948 = CARTESIAN_POINT('',(12.,-12.,43.2)) ;
#46949 = CARTESIAN_POINT('',(12.,12.,43.2)) ;
#46950 = CARTESIAN_POINT('',(12.,0.,43.2)) ;
#46951 = CARTESIAN_POINT('',(-12.,12.,43.2)) ;
#46952 = CARTESIAN_POINT('',(0.,12.,43.2)) ;
#46953 = CARTESIAN_POINT('',(-12.,-12.,43.2)) ;
#46954 = CARTESIAN_POINT('',(-12.,0.,43.2)) ;
#46955 = CARTESIAN_POINT('',(0.,-12.,43.2)) ;
#46956 = CARTESIAN_POINT('Origin',(0.,-12.,43.)) ;
#46957 = CARTESIAN_POINT('',(-12.,-12.,43.)) ;
#46958 = CARTESIAN_POINT('',(12.,-12.,43.)) ;
#46959 = CARTESIAN_POINT('Origin',(-12.,0.,43.)) ;
#46960 = CARTESIAN_POINT('',(-12.,12.,43.)) ;
#46961 = CARTESIAN_POINT('Origin',(0.,12.,43.)) ;
#46962 = CARTESIAN_POINT('',(12.,12.,43.)) ;
#46963 = CARTESIAN_POINT('Origin',(12.,0.,43.)) ;
#46964 = CARTESIAN_POINT('Origin',(0.,0.,45.6)) ;
#46965 = CARTESIAN_POINT('',(-11.2,1.37160441504504E-15,48.)) ;
#46966 = CARTESIAN_POINT('',(-8.7,-1.0654427152582E-15,45.6)) ;
#46967 = CARTESIAN_POINT('Origin',(0.,0.,48.)) ;
#46968 = CARTESIAN_POINT('Origin',(0.,0.,48.)) ;
#46969 = CARTESIAN_POINT('',(0.,0.,0.)) ;
#46970 = CARTESIAN_POINT('Origin',(0.,0.,41.8)) ;
#46971 = CARTESIAN_POINT('',(-6.3,-7.71527483462833E-16,41.6)) ;
#46972 = CARTESIAN_POINT('Origin',(0.,0.,41.6)) ;
#46973 = CARTESIAN_POINT('',(-6.3,-7.71527483462833E-16,41.8)) ;
#46974 = CARTESIAN_POINT('',(-6.3,-7.71527483462833E-16,41.8)) ;
#46975 = CARTESIAN_POINT('Origin',(0.,0.,41.8)) ;
#46976 = CARTESIAN_POINT('Origin',(0.,0.,41.8)) ;
#46977 = CARTESIAN_POINT('',(-6.3,7.71527483462833E-16,42.)) ;
#46978 = CARTESIAN_POINT('',(-6.3,-7.71527483462833E-16,41.8)) ;
#46979 = CARTESIAN_POINT('Origin',(0.,0.,42.)) ;
#46980 = CARTESIAN_POINT('Origin',(0.,0.,41.8)) ;
#46981 = CARTESIAN_POINT('',(-6.8,-8.327598234202E-16,42.)) ;
#46982 = CARTESIAN_POINT('Origin',(0.,0.,42.)) ;
#46983 = CARTESIAN_POINT('',(-6.8,-8.327598234202E-16,41.6)) ;
#46984 = CARTESIAN_POINT('',(-6.8,-8.327598234202E-16,41.8)) ;
#46985 = CARTESIAN_POINT('Origin',(0.,0.,41.6)) ;
#46986 = CARTESIAN_POINT('Origin',(0.,0.,41.6)) ;
#46987 = CARTESIAN_POINT('Origin',(0.,0.,42.)) ;
#46988 = CARTESIAN_POINT('Origin',(0.,0.,25.)) ;
#46989 = CARTESIAN_POINT('',(-3.,3.67394039744206E-16,25.)) ;
#46990 = CARTESIAN_POINT('Origin',(0.,0.,25.)) ;
#46991 = CARTESIAN_POINT('',(-2.8,-3.42901103761259E-16,25.)) ;
#46992 = CARTESIAN_POINT('Origin',(0.,0.,25.)) ;
#46993 = CARTESIAN_POINT('Origin',(0.,0.,41.8)) ;
#46994 = CARTESIAN_POINT('',(-6.3,-7.71527483462833E-16,41.8)) ;
#46995 = CARTESIAN_POINT('Origin',(0.,0.,41.8)) ;
#46996 = CARTESIAN_POINT('',(-6.1,7.47034547479886E-16,41.8)) ;
#46997 = CARTESIAN_POINT('Origin',(0.,0.,41.8)) ;
#46998 = CARTESIAN_POINT('Origin',(0.,0.,33.4)) ;
#46999 = CARTESIAN_POINT('',(-4.65,5.69460761603519E-16,33.4)) ;
#47000 = CARTESIAN_POINT('Origin',(0.,0.,33.4)) ;
#47001 = CARTESIAN_POINT('',(-4.45,5.44967825620572E-16,33.4)) ;
#47002 = CARTESIAN_POINT('',(0.,0.,0.)) ;
#47003 = CARTESIAN_POINT('Origin',(-56.5,18.2,98.0621778264911)) ;
#47004 = CARTESIAN_POINT('',(-56.9,18.,98.0621778264911)) ;
#47005 = CARTESIAN_POINT('Origin',(-56.5,18.,98.0621778264911)) ;
#47006 = CARTESIAN_POINT('',(-56.9,18.4,98.0621778264911)) ;
#47007 = CARTESIAN_POINT('',(-56.9,18.2,98.0621778264911)) ;
#47008 = CARTESIAN_POINT('Origin',(-56.5,18.4,98.0621778264911)) ;
#47009 = CARTESIAN_POINT('Origin',(-55.3941410032797,18.2,98.5778483455014)) ;
#47010 = CARTESIAN_POINT('',(-55.7941410032797,18.,98.5778483455014)) ;
#47011 = CARTESIAN_POINT('Origin',(-55.3941410032797,18.,98.5778483455014)) ;
#47012 = CARTESIAN_POINT('',(-55.7941410032797,18.4,98.5778483455014)) ;
#47013 = CARTESIAN_POINT('',(-55.7941410032797,18.2,98.5778483455014)) ;
#47014 = CARTESIAN_POINT('Origin',(-55.3941410032797,18.4,98.5778483455014)) ;
#47015 = CARTESIAN_POINT('Origin',(-54.2155372436685,18.2,98.8936542710855)) ;
#47016 = CARTESIAN_POINT('',(-54.6155372436685,18.,98.8936542710855)) ;
#47017 = CARTESIAN_POINT('Origin',(-54.2155372436685,18.,98.8936542710855)) ;
#47018 = CARTESIAN_POINT('',(-54.6155372436685,18.4,98.8936542710855)) ;
#47019 = CARTESIAN_POINT('',(-54.6155372436685,18.2,98.8936542710855)) ;
#47020 = CARTESIAN_POINT('Origin',(-54.2155372436685,18.4,98.8936542710855)) ;
#47021 = CARTESIAN_POINT('Origin',(-53.,18.2,99.)) ;
#47022 = CARTESIAN_POINT('',(-53.4,18.,99.)) ;
#47023 = CARTESIAN_POINT('Origin',(-53.,18.,99.)) ;
#47024 = CARTESIAN_POINT('',(-53.4,18.4,99.)) ;
#47025 = CARTESIAN_POINT('',(-53.4,18.2,99.)) ;
#47026 = CARTESIAN_POINT('Origin',(-53.,18.4,99.)) ;
#47027 = CARTESIAN_POINT('Origin',(-51.7844627563315,18.2,98.8936542710855)) ;
#47028 = CARTESIAN_POINT('',(-52.1844627563315,18.,98.8936542710855)) ;
#47029 = CARTESIAN_POINT('Origin',(-51.7844627563315,18.,98.8936542710855)) ;
#47030 = CARTESIAN_POINT('',(-52.1844627563315,18.4,98.8936542710855)) ;
#47031 = CARTESIAN_POINT('',(-52.1844627563315,18.2,98.8936542710855)) ;
#47032 = CARTESIAN_POINT('Origin',(-51.7844627563315,18.4,98.8936542710855)) ;
#47033 = CARTESIAN_POINT('Origin',(-50.6058589967203,18.2,98.5778483455014)) ;
#47034 = CARTESIAN_POINT('',(-51.0058589967203,18.,98.5778483455014)) ;
#47035 = CARTESIAN_POINT('Origin',(-50.6058589967203,18.,98.5778483455014)) ;
#47036 = CARTESIAN_POINT('',(-51.0058589967203,18.4,98.5778483455014)) ;
#47037 = CARTESIAN_POINT('',(-51.0058589967203,18.2,98.5778483455014)) ;
#47038 = CARTESIAN_POINT('Origin',(-50.6058589967203,18.4,98.5778483455014)) ;
#47039 = CARTESIAN_POINT('Origin',(-49.5,18.2,98.0621778264911)) ;
#47040 = CARTESIAN_POINT('',(-49.9,18.,98.0621778264911)) ;
#47041 = CARTESIAN_POINT('Origin',(-49.5,18.,98.0621778264911)) ;
#47042 = CARTESIAN_POINT('',(-49.9,18.4,98.0621778264911)) ;
#47043 = CARTESIAN_POINT('',(-49.9,18.2,98.0621778264911)) ;
#47044 = CARTESIAN_POINT('Origin',(-49.5,18.4,98.0621778264911)) ;
#47045 = CARTESIAN_POINT('Origin',(-53.,18.2,92.)) ;
#47046 = CARTESIAN_POINT('',(-53.51,18.,92.)) ;
#47047 = CARTESIAN_POINT('Origin',(-53.,18.,92.)) ;
#47048 = CARTESIAN_POINT('',(-53.51,18.4,92.)) ;
#47049 = CARTESIAN_POINT('',(-53.51,18.2,92.)) ;
#47050 = CARTESIAN_POINT('Origin',(-53.,18.4,92.)) ;
#47051 = CARTESIAN_POINT('Origin',(-53.,18.2,90.)) ;
#47052 = CARTESIAN_POINT('',(-60.7459666924148,18.,90.)) ;
#47053 = CARTESIAN_POINT('',(-45.2540333075852,18.,90.)) ;
#47054 = CARTESIAN_POINT('',(-53.,18.,90.)) ;
#47055 = CARTESIAN_POINT('',(-60.7459666924148,18.4,90.)) ;
#47056 = CARTESIAN_POINT('',(-60.7459666924148,18.2,90.)) ;
#47057 = CARTESIAN_POINT('',(-45.2540333075852,18.4,90.)) ;
#47058 = CARTESIAN_POINT('',(-53.,18.4,90.)) ;
#47059 = CARTESIAN_POINT('',(-45.2540333075852,18.2,90.)) ;
#47060 = CARTESIAN_POINT('Origin',(-53.,18.4,92.)) ;
#47061 = CARTESIAN_POINT('Origin',(-53.,18.4,92.)) ;
#47062 = CARTESIAN_POINT('Origin',(-53.,18.,92.)) ;
#47063 = CARTESIAN_POINT('Origin',(-53.,18.,92.)) ;
#47064 = CARTESIAN_POINT('Origin',(-53.,18.2,92.)) ;
#47065 = CARTESIAN_POINT('',(0.,0.,0.)) ;
#47066 = CARTESIAN_POINT('Origin',(-53.,18.1,99.)) ;
#47067 = CARTESIAN_POINT('',(-52.6,18.6,99.)) ;
#47068 = CARTESIAN_POINT('',(-53.4,18.6,99.)) ;
#47069 = CARTESIAN_POINT('Origin',(-53.,18.6,99.)) ;
#47070 = CARTESIAN_POINT('Origin',(-53.,18.6,99.)) ;
#47071 = CARTESIAN_POINT('',(-53.4,17.6,99.)) ;
#47072 = CARTESIAN_POINT('',(-53.4,18.1,99.)) ;
#47073 = CARTESIAN_POINT('Origin',(-53.,17.6,99.)) ;
#47074 = CARTESIAN_POINT('Origin',(-53.,17.6,99.)) ;
#47075 = CARTESIAN_POINT('Origin',(-53.,18.6,96.)) ;
#47076 = CARTESIAN_POINT('',(-52.6,18.6,104.)) ;
#47077 = CARTESIAN_POINT('',(-52.6,18.6,96.)) ;
#47078 = CARTESIAN_POINT('',(-53.4,18.6,104.)) ;
#47079 = CARTESIAN_POINT('',(-53.,18.6,104.)) ;
#47080 = CARTESIAN_POINT('',(-53.4,18.6,96.)) ;
#47081 = CARTESIAN_POINT('Origin',(-53.,18.6,96.)) ;
#47082 = CARTESIAN_POINT('',(-53.4,18.6,92.8)) ;
#47083 = CARTESIAN_POINT('',(-53.4,18.6,96.)) ;
#47084 = CARTESIAN_POINT('',(-52.6,18.6,92.8)) ;
#47085 = CARTESIAN_POINT('',(-53.,18.6,92.8)) ;
#47086 = CARTESIAN_POINT('',(-52.6,18.6,96.)) ;
#47087 = CARTESIAN_POINT('Origin',(-53.,19.,89.6)) ;
#47088 = CARTESIAN_POINT('',(-53.31,19.,89.3)) ;
#47089 = CARTESIAN_POINT('Origin',(-53.,19.,89.3)) ;
#47090 = CARTESIAN_POINT('',(-53.31,19.,89.9)) ;
#47091 = CARTESIAN_POINT('',(-53.31,19.,89.6)) ;
#47092 = CARTESIAN_POINT('Origin',(-53.,19.,89.9)) ;
#47093 = CARTESIAN_POINT('Origin',(-53.,19.,89.3)) ;
#47094 = CARTESIAN_POINT('',(-53.15,19.,89.3)) ;
#47095 = CARTESIAN_POINT('Origin',(-53.,19.,89.3)) ;
#47096 = CARTESIAN_POINT('Origin',(-53.,19.,89.9)) ;
#47097 = CARTESIAN_POINT('Origin',(-53.,19.,88.7)) ;
#47098 = CARTESIAN_POINT('',(-53.15,19.,88.)) ;
#47099 = CARTESIAN_POINT('Origin',(-53.,19.,88.)) ;
#47100 = CARTESIAN_POINT('',(-53.15,19.,88.7)) ;
#47101 = CARTESIAN_POINT('Origin',(-53.,19.,92.)) ;
#47102 = CARTESIAN_POINT('',(-53.51,18.4,92.)) ;
#47103 = CARTESIAN_POINT('Origin',(-53.,18.4,92.)) ;
#47104 = CARTESIAN_POINT('',(-53.51,19.6,92.)) ;
#47105 = CARTESIAN_POINT('',(-53.51,19.,92.)) ;
#47106 = CARTESIAN_POINT('Origin',(-53.,19.6,92.)) ;
#47107 = CARTESIAN_POINT('Origin',(-53.,19.,91.2)) ;
#47108 = CARTESIAN_POINT('',(-52.,19.6,91.2)) ;
#47109 = CARTESIAN_POINT('',(-52.,18.4,91.2)) ;
#47110 = CARTESIAN_POINT('',(-52.,19.,91.2)) ;
#47111 = CARTESIAN_POINT('',(-54.,18.4,91.2)) ;
#47112 = CARTESIAN_POINT('',(-53.,18.4,91.2)) ;
#47113 = CARTESIAN_POINT('',(-54.,19.6,91.2)) ;
#47114 = CARTESIAN_POINT('',(-54.,19.,91.2)) ;
#47115 = CARTESIAN_POINT('',(-53.,19.6,91.2)) ;
#47116 = CARTESIAN_POINT('',(-53.4,19.4,91.2)) ;
#47117 = CARTESIAN_POINT('',(-52.6,19.4,91.2)) ;
#47118 = CARTESIAN_POINT('',(-53.,19.4,91.2)) ;
#47119 = CARTESIAN_POINT('',(-53.4,18.6,91.2)) ;
#47120 = CARTESIAN_POINT('',(-53.4,19.,91.2)) ;
#47121 = CARTESIAN_POINT('',(-52.6,18.6,91.2)) ;
#47122 = CARTESIAN_POINT('',(-53.,18.6,91.2)) ;
#47123 = CARTESIAN_POINT('',(-52.6,19.,91.2)) ;
#47124 = CARTESIAN_POINT('Origin',(-53.,19.,92.8)) ;
#47125 = CARTESIAN_POINT('',(-52.,18.4,92.8)) ;
#47126 = CARTESIAN_POINT('',(-52.,19.6,92.8)) ;
#47127 = CARTESIAN_POINT('',(-52.,19.,92.8)) ;
#47128 = CARTESIAN_POINT('',(-54.,19.6,92.8)) ;
#47129 = CARTESIAN_POINT('',(-53.,19.6,92.8)) ;
#47130 = CARTESIAN_POINT('',(-54.,18.4,92.8)) ;
#47131 = CARTESIAN_POINT('',(-54.,19.,92.8)) ;
#47132 = CARTESIAN_POINT('',(-53.,18.4,92.8)) ;
#47133 = CARTESIAN_POINT('',(-52.6,19.4,92.8)) ;
#47134 = CARTESIAN_POINT('',(-52.6,19.,92.8)) ;
#47135 = CARTESIAN_POINT('',(-53.4,19.4,92.8)) ;
#47136 = CARTESIAN_POINT('',(-53.4,19.,92.8)) ;
#47137 = CARTESIAN_POINT('',(-53.,19.4,92.8)) ;
#47138 = CARTESIAN_POINT('Origin',(-53.,18.4,92.)) ;
#47139 = CARTESIAN_POINT('',(-54.,18.4,92.)) ;
#47140 = CARTESIAN_POINT('',(-52.,18.4,92.)) ;
#47141 = CARTESIAN_POINT('Origin',(-54.,19.,92.)) ;
#47142 = CARTESIAN_POINT('',(-54.,19.6,92.)) ;
#47143 = CARTESIAN_POINT('Origin',(-53.,19.6,92.)) ;
#47144 = CARTESIAN_POINT('',(-52.,19.6,92.)) ;
#47145 = CARTESIAN_POINT('Origin',(-52.,19.,92.)) ;
#47146 = CARTESIAN_POINT('Origin',(-53.4,19.,96.)) ;
#47147 = CARTESIAN_POINT('',(-53.4,19.4,104.)) ;
#47148 = CARTESIAN_POINT('',(-53.4,19.,104.)) ;
#47149 = CARTESIAN_POINT('',(-53.4,19.4,96.)) ;
#47150 = CARTESIAN_POINT('Origin',(-52.6,19.,96.)) ;
#47151 = CARTESIAN_POINT('',(-52.6,19.4,104.)) ;
#47152 = CARTESIAN_POINT('',(-52.6,19.4,96.)) ;
#47153 = CARTESIAN_POINT('',(-52.6,19.,104.)) ;
#47154 = CARTESIAN_POINT('Origin',(-53.,19.,104.)) ;
#47155 = CARTESIAN_POINT('',(-53.,19.4,104.)) ;
#47156 = CARTESIAN_POINT('Origin',(-53.,19.4,96.)) ;
#47157 = CARTESIAN_POINT('Origin',(-53.,18.6,96.)) ;
#47158 = CARTESIAN_POINT('',(-53.4,18.6,88.)) ;
#47159 = CARTESIAN_POINT('',(-53.4,18.6,96.)) ;
#47160 = CARTESIAN_POINT('',(-52.6,18.6,88.)) ;
#47161 = CARTESIAN_POINT('',(-53.,18.6,88.)) ;
#47162 = CARTESIAN_POINT('',(-52.6,18.6,96.)) ;
#47163 = CARTESIAN_POINT('Origin',(-53.4,19.,96.)) ;
#47164 = CARTESIAN_POINT('',(-53.4,19.4,88.)) ;
#47165 = CARTESIAN_POINT('',(-53.4,19.4,96.)) ;
#47166 = CARTESIAN_POINT('',(-53.4,19.,88.)) ;
#47167 = CARTESIAN_POINT('Origin',(-53.,19.4,96.)) ;
#47168 = CARTESIAN_POINT('',(-52.6,19.4,88.)) ;
#47169 = CARTESIAN_POINT('',(-52.6,19.4,96.)) ;
#47170 = CARTESIAN_POINT('',(-53.,19.4,88.)) ;
#47171 = CARTESIAN_POINT('Origin',(-52.6,19.,96.)) ;
#47172 = CARTESIAN_POINT('',(-52.6,19.,88.)) ;
#47173 = CARTESIAN_POINT('Origin',(-53.,19.,88.)) ;
#47174 = CARTESIAN_POINT('',(0.,0.,0.)) ;
#47175 = CARTESIAN_POINT('Origin',(-53.,19.,104.3)) ;
#47176 = CARTESIAN_POINT('',(-53.7,19.,104.361250543006)) ;
#47177 = CARTESIAN_POINT('Origin',(-53.,19.,104.361250543006)) ;
#47178 = CARTESIAN_POINT('',(-53.7,19.,104.)) ;
#47179 = CARTESIAN_POINT('',(-53.7,19.,104.3)) ;
#47180 = CARTESIAN_POINT('Origin',(-53.,19.,104.)) ;
#47181 = CARTESIAN_POINT('Origin',(-53.,19.,104.)) ;
#47182 = CARTESIAN_POINT('Origin',(-53.,19.,105.8)) ;
#47183 = CARTESIAN_POINT('',(-53.,19.,107.4)) ;
#47184 = CARTESIAN_POINT('Origin',(-53.,19.,105.8)) ;
#47185 = CARTESIAN_POINT('',(0.,0.,0.)) ;
#47186 = CARTESIAN_POINT('Origin',(-53.,17.6,92.)) ;
#47187 = CARTESIAN_POINT('',(-53.8,17.6,92.)) ;
#47188 = CARTESIAN_POINT('Origin',(-53.,17.6,92.)) ;
#47189 = CARTESIAN_POINT('',(-53.5,17.6,92.)) ;
#47190 = CARTESIAN_POINT('Origin',(-53.,17.6,92.)) ;
#47191 = CARTESIAN_POINT('Origin',(-53.,17.4,92.)) ;
#47192 = CARTESIAN_POINT('',(-53.8,17.2,92.)) ;
#47193 = CARTESIAN_POINT('',(-53.8,17.4,92.)) ;
#47194 = CARTESIAN_POINT('Origin',(-53.,17.2,92.)) ;
#47195 = CARTESIAN_POINT('Origin',(-53.,17.2,92.)) ;
#47196 = CARTESIAN_POINT('Origin',(-53.,19.,92.)) ;
#47197 = CARTESIAN_POINT('',(-53.5,20.4,92.)) ;
#47198 = CARTESIAN_POINT('Origin',(-53.,20.4,92.)) ;
#47199 = CARTESIAN_POINT('',(-53.5,19.,92.)) ;
#47200 = CARTESIAN_POINT('Origin',(-53.,20.4,92.)) ;
#47201 = CARTESIAN_POINT('',(0.,0.,0.)) ;
#47202 = CARTESIAN_POINT('Origin',(-57.8,19.,87.2)) ;
#47203 = CARTESIAN_POINT('',(-57.8,19.,87.05)) ;
#47204 = CARTESIAN_POINT('',(-57.8,19.,87.35)) ;
#47205 = CARTESIAN_POINT('Origin',(-57.8,19.,87.2)) ;
#47206 = CARTESIAN_POINT('Origin',(-57.8,0.,45.)) ;
#47207 = CARTESIAN_POINT('',(-57.8,-1.12481983699639E-33,44.85)) ;
#47208 = CARTESIAN_POINT('',(-57.8,-1.12481983699639E-33,45.15)) ;
#47209 = CARTESIAN_POINT('Origin',(-57.8,0.,45.)) ;
#47210 = CARTESIAN_POINT('Origin',(-20.,0.,43.6)) ;
#47211 = CARTESIAN_POINT('',(-20.,-1.12481983699639E-33,43.45)) ;
#47212 = CARTESIAN_POINT('',(-20.,-1.12481983699639E-33,43.75)) ;
#47213 = CARTESIAN_POINT('Origin',(-20.,0.,43.6)) ;
#47214 = CARTESIAN_POINT('Origin',(-20.,0.,43.6)) ;
#47215 = CARTESIAN_POINT('',(-20.3765088376712,1.83697019872102E-17,43.4649404014685)) ;
#47216 = CARTESIAN_POINT('Origin',(-20.3705136319189,0.,43.6148205452768)) ;
#47217 = CARTESIAN_POINT('Origin',(-25.,0.,43.8)) ;
#47218 = CARTESIAN_POINT('',(-29.6354815738335,-1.83697019872102E-17,43.835299310915)) ;
#47219 = CARTESIAN_POINT('Origin',(-29.6294863680811,0.,43.9851794547233)) ;
#47220 = CARTESIAN_POINT('',(-25.0059952057523,1.83697019872103E-17,43.6501198561917)) ;
#47221 = CARTESIAN_POINT('Origin',(-30.,0.,44.)) ;
#47222 = CARTESIAN_POINT('Origin',(-30.,0.,44.)) ;
#47223 = CARTESIAN_POINT('',(-29.9999999999997,-0.4,44.0000000000068)) ;
#47224 = CARTESIAN_POINT('',(-29.9999999999997,0.4,44.0000000000068)) ;
#47225 = CARTESIAN_POINT('Origin',(-30.,0.,44.)) ;
#47226 = CARTESIAN_POINT('Origin',(-30.,0.,44.)) ;
#47227 = CARTESIAN_POINT('Origin',(-57.8,0.,45.)) ;
#47228 = CARTESIAN_POINT('',(-57.8139063298872,0.101735781806649,44.6134040291347)) ;
#47229 = CARTESIAN_POINT('',(-57.8143791893917,4.89858719658941E-17,44.6002585349098)) ;
#47230 = CARTESIAN_POINT('Origin',(-57.8,0.,45.)) ;
#47231 = CARTESIAN_POINT('',(-57.7860936701128,-0.101735781806649,45.3865959708653)) ;
#47232 = CARTESIAN_POINT('Origin',(-57.8,0.,45.)) ;
#47233 = CARTESIAN_POINT('',(-58.2,-1.06581410364015E-14,45.)) ;
#47234 = CARTESIAN_POINT('Origin',(-57.8,0.,45.)) ;
#47235 = CARTESIAN_POINT('Origin',(-57.8,0.,45.)) ;
#47236 = CARTESIAN_POINT('Origin',(-57.8,19.,87.2)) ;
#47237 = CARTESIAN_POINT('',(-57.4291900756452,18.85,87.2)) ;
#47238 = CARTESIAN_POINT('',(-57.4291900756452,19.15,87.2)) ;
#47239 = CARTESIAN_POINT('Origin',(-57.8,19.,87.2)) ;
#47240 = CARTESIAN_POINT('Origin',(-57.4291900756452,19.,87.2)) ;
#47241 = CARTESIAN_POINT('Origin',(-57.8,19.,87.2)) ;
#47242 = CARTESIAN_POINT('',(-57.8,19.4,87.2)) ;
#47243 = CARTESIAN_POINT('',(-58.2,19.,87.2)) ;
#47244 = CARTESIAN_POINT('Origin',(-57.8,19.,87.2)) ;
#47245 = CARTESIAN_POINT('',(-57.8,18.6,87.2)) ;
#47246 = CARTESIAN_POINT('Origin',(-57.8,19.,87.2)) ;
#47247 = CARTESIAN_POINT('Origin',(-57.8,19.,87.2)) ;
#47248 = CARTESIAN_POINT('Origin',(-55.6,19.,87.2)) ;
#47249 = CARTESIAN_POINT('',(-53.4,19.,87.05)) ;
#47250 = CARTESIAN_POINT('Origin',(-53.4,19.,87.2)) ;
#47251 = CARTESIAN_POINT('',(-57.4,19.,87.05)) ;
#47252 = CARTESIAN_POINT('',(-55.6,19.,87.05)) ;
#47253 = CARTESIAN_POINT('Ctrl Pts',(-57.4,19.,87.05)) ;
#47254 = CARTESIAN_POINT('Ctrl Pts',(-57.4,18.9809695677553,87.05)) ;
#47255 = CARTESIAN_POINT('Ctrl Pts',(-57.4014894752437,18.9607940299519,87.0538410060698)) ;
#47256 = CARTESIAN_POINT('Ctrl Pts',(-57.4068656051584,18.9238876225274,87.0692083147017)) ;
#47257 = CARTESIAN_POINT('Ctrl Pts',(-57.4106861522654,18.9071430958613,87.0807248697828)) ;
#47258 = CARTESIAN_POINT('Ctrl Pts',(-57.4179542005944,18.8807147469091,87.1071532187349)) ;
#47259 = CARTESIAN_POINT('Ctrl Pts',(-57.4218995741112,18.8692059165228,87.1238938323863)) ;
#47260 = CARTESIAN_POINT('Ctrl Pts',(-57.4275680116987,18.8538444576424,87.1607852902757)) ;
#47261 = CARTESIAN_POINT('Ctrl Pts',(-57.4291900756452,18.85,87.1809549836829)) ;
#47262 = CARTESIAN_POINT('Ctrl Pts',(-57.4291900756452,18.85,87.2)) ;
#47263 = CARTESIAN_POINT('Ctrl Pts',(-57.4291900756452,19.15,87.2)) ;
#47264 = CARTESIAN_POINT('Ctrl Pts',(-57.4291900756452,19.15,87.1809549836829)) ;
#47265 = CARTESIAN_POINT('Ctrl Pts',(-57.4275680116987,19.1461555423576,87.1607852902757)) ;
#47266 = CARTESIAN_POINT('Ctrl Pts',(-57.4218995741112,19.1307940834772,87.1238938323863)) ;
#47267 = CARTESIAN_POINT('Ctrl Pts',(-57.4179542005944,19.1192852530909,87.1071532187349)) ;
#47268 = CARTESIAN_POINT('Ctrl Pts',(-57.4106861522654,19.0928569041387,87.0807248697828)) ;
#47269 = CARTESIAN_POINT('Ctrl Pts',(-57.4068656051584,19.0761123774726,87.0692083147017)) ;
#47270 = CARTESIAN_POINT('Ctrl Pts',(-57.4014894752437,19.0392059700481,87.0538410060698)) ;
#47271 = CARTESIAN_POINT('Ctrl Pts',(-57.4,19.0190304322447,87.05)) ;
#47272 = CARTESIAN_POINT('Ctrl Pts',(-57.4,19.,87.05)) ;
#47273 = CARTESIAN_POINT('Origin',(-19.05,0.,43.6)) ;
#47274 = CARTESIAN_POINT('',(-19.6291900756452,1.83697019872101E-17,43.75)) ;
#47275 = CARTESIAN_POINT('Origin',(-19.6291900756452,0.,43.6)) ;
#47276 = CARTESIAN_POINT('',(-18.1,1.83697019872103E-17,43.75)) ;
#47277 = CARTESIAN_POINT('',(-19.05,-1.83697019872103E-17,43.75)) ;
#47278 = CARTESIAN_POINT('Origin',(-18.1,0.,43.6)) ;
#47279 = CARTESIAN_POINT('Origin',(-19.05,0.,43.6)) ;
#47280 = CARTESIAN_POINT('',(-18.1,-4.89858719658941E-17,44.)) ;
#47281 = CARTESIAN_POINT('Origin',(-18.1,0.,43.6)) ;
#47282 = CARTESIAN_POINT('',(-19.9920031974416,-4.89858719658943E-17,44.)) ;
#47283 = CARTESIAN_POINT('',(-19.05,-4.89858719658941E-17,44.)) ;
#47284 = CARTESIAN_POINT('',(-20.,-0.4,43.6000000000023)) ;
#47285 = CARTESIAN_POINT('Origin',(-19.9999999999996,0.,43.6)) ;
#47286 = CARTESIAN_POINT('',(-20.,0.4,43.6000000000023)) ;
#47287 = CARTESIAN_POINT('Origin',(-20.,0.,43.6)) ;
#47288 = CARTESIAN_POINT('Origin',(-19.9999999999996,0.,43.6)) ;
#47289 = CARTESIAN_POINT('Origin',(-18.1,0.,43.6)) ;
#47290 = CARTESIAN_POINT('Origin',(-25.,0.,43.8)) ;
#47291 = CARTESIAN_POINT('',(-20.0159872153392,4.89858719658941E-17,43.2003196165113)) ;
#47292 = CARTESIAN_POINT('Origin',(-20.,0.,43.6)) ;
#47293 = CARTESIAN_POINT('',(-30.0151832638221,4.8985871965894E-17,43.6002874584506)) ;
#47294 = CARTESIAN_POINT('',(-25.0159872153395,4.89858719658941E-17,43.4003196165113)) ;
#47295 = CARTESIAN_POINT('Origin',(-30.0000000000128,0.,44.0000000000005)) ;
#47296 = CARTESIAN_POINT('Origin',(-30.0000000000128,0.,44.0000000000005)) ;
#47297 = CARTESIAN_POINT('Origin',(-20.,0.,43.6)) ;
#47298 = CARTESIAN_POINT('Origin',(-43.9,0.,44.5)) ;
#47299 = CARTESIAN_POINT('',(-43.9143791893917,4.89858719658941E-17,44.1002585349098)) ;
#47300 = CARTESIAN_POINT('Origin',(-57.8,0.,45.)) ;
#47301 = CARTESIAN_POINT('Origin',(-57.8,9.5,47.5)) ;
#47302 = CARTESIAN_POINT('',(-58.2,19.,50.)) ;
#47303 = CARTESIAN_POINT('',(-58.2,9.5,47.5)) ;
#47304 = CARTESIAN_POINT('',(-57.4,19.,50.)) ;
#47305 = CARTESIAN_POINT('Origin',(-57.8,19.,50.)) ;
#47306 = CARTESIAN_POINT('Origin',(-57.8,19.,50.)) ;
#47307 = CARTESIAN_POINT('Origin',(-57.8,19.,68.6)) ;
#47308 = CARTESIAN_POINT('Origin',(-57.8,19.,50.)) ;
#47309 = CARTESIAN_POINT('',(-58.2,19.,68.6)) ;
#47310 = CARTESIAN_POINT('',(-57.4,19.,86.8)) ;
#47311 = CARTESIAN_POINT('Origin',(-57.8,19.,87.2)) ;
#47312 = CARTESIAN_POINT('Origin',(-57.8,19.,87.2)) ;
#47313 = CARTESIAN_POINT('Origin',(-57.8,19.,68.6)) ;
#47314 = CARTESIAN_POINT('Origin',(-55.6,19.,87.2)) ;
#47315 = CARTESIAN_POINT('',(-53.4,19.,86.8)) ;
#47316 = CARTESIAN_POINT('',(-55.6,19.,86.8)) ;
#47317 = CARTESIAN_POINT('Origin',(-53.4,19.,87.2)) ;
#47318 = CARTESIAN_POINT('Origin',(-53.4,19.,87.2)) ;
#47319 = CARTESIAN_POINT('Origin',(-57.8,19.,50.)) ;
#47320 = CARTESIAN_POINT('Origin',(-20.,0.,43.6)) ;
#47321 = CARTESIAN_POINT('Origin',(-20.,0.,43.6)) ;
#47322 = CARTESIAN_POINT('Origin',(-30.,0.,44.)) ;
#47323 = CARTESIAN_POINT('',(-30.3759624521008,1.83697019872102E-17,43.8634268159178)) ;
#47324 = CARTESIAN_POINT('Origin',(-30.3705702560789,0.,44.0133298653266)) ;
#47325 = CARTESIAN_POINT('Origin',(-57.8,0.,45.)) ;
#47326 = CARTESIAN_POINT('',(-57.4346122660986,0.041422100489503,44.8425960181399)) ;
#47327 = CARTESIAN_POINT('',(-57.434821939943,1.83697019872103E-17,44.8367670852646)) ;
#47328 = CARTESIAN_POINT('Origin',(-57.4294297439211,0.,44.9866701346734)) ;
#47329 = CARTESIAN_POINT('',(-57.4241851865086,-0.0348602186165462,45.1324688307429)) ;
#47330 = CARTESIAN_POINT('Origin',(-57.8,0.,45.)) ;
#47331 = CARTESIAN_POINT('Origin',(-57.4294297439211,0.,44.9866701346734)) ;
#47332 = CARTESIAN_POINT('Origin',(-43.9,0.,44.5)) ;
#47333 = CARTESIAN_POINT('',(-43.9053921960219,1.83697019872103E-17,44.3500969505912)) ;
#47334 = CARTESIAN_POINT('Ctrl Pts',(-57.4346122660986,0.0414221004895022,
44.8425960181399)) ;
#47335 = CARTESIAN_POINT('Ctrl Pts',(-57.4344333524598,0.0587443254615674,
44.8475698172985)) ;
#47336 = CARTESIAN_POINT('Ctrl Pts',(-57.4326932970465,0.076021419458707,
44.8560347742558)) ;
#47337 = CARTESIAN_POINT('Ctrl Pts',(-57.4266783464393,0.106859093622014,
44.8793548046319)) ;
#47338 = CARTESIAN_POINT('Ctrl Pts',(-57.4223334613447,0.12012956463638,44.8946026069999)) ;
#47339 = CARTESIAN_POINT('Ctrl Pts',(-57.414147220962,0.138975753362532,44.9266249722163)) ;
#47340 = CARTESIAN_POINT('Ctrl Pts',(-57.4097459189252,0.145853589807542,
44.9456087582207)) ;
#47341 = CARTESIAN_POINT('Ctrl Pts',(-57.4030911664522,0.151324256094906,
44.9849967325437)) ;
#47342 = CARTESIAN_POINT('Ctrl Pts',(-57.4009030339391,0.149904658760938,
45.0054136535252)) ;
#47343 = CARTESIAN_POINT('Ctrl Pts',(-57.3995805772631,0.140229844131874,
45.0421779491157)) ;
#47344 = CARTESIAN_POINT('Ctrl Pts',(-57.4003662647291,0.131389448751725,
45.0607490004478)) ;
#47345 = CARTESIAN_POINT('Ctrl Pts',(-57.4044547408517,0.10714444495445,45.0927035086624)) ;
#47346 = CARTESIAN_POINT('Ctrl Pts',(-57.4076912940542,0.0917455512477126,
45.1060997402527)) ;
#47347 = CARTESIAN_POINT('Ctrl Pts',(-57.4140390783082,0.0594496045273251,
45.1251864554143)) ;
#47348 = CARTESIAN_POINT('Ctrl Pts',(-57.4175834666219,0.0403228675895078,
45.1321924635554)) ;
#47349 = CARTESIAN_POINT('Ctrl Pts',(-57.4225620861009,0.00190361306705893,
45.1376824385441)) ;
#47350 = CARTESIAN_POINT('Ctrl Pts',(-57.4240346154731,-0.0173306451253857,
45.1366547055289)) ;
#47351 = CARTESIAN_POINT('Ctrl Pts',(-57.4241851865085,-0.0348602186165459,
45.1324688307429)) ;
#47352 = CARTESIAN_POINT('Origin',(-57.8,9.5,47.5)) ;
#47353 = CARTESIAN_POINT('Origin',(-30.,0.,44.)) ;
#47354 = CARTESIAN_POINT('',(-30.,-1.12481983699639E-33,43.85)) ;
#47355 = CARTESIAN_POINT('',(-30.,-1.12481983699639E-33,44.15)) ;
#47356 = CARTESIAN_POINT('Origin',(-30.,0.,44.)) ;
#47357 = CARTESIAN_POINT('Origin',(-57.8,19.,50.)) ;
#47358 = CARTESIAN_POINT('',(-57.6860796798847,18.6165653110831,50.)) ;
#47359 = CARTESIAN_POINT('',(-57.9139203201154,18.6165653110831,50.)) ;
#47360 = CARTESIAN_POINT('Origin',(-57.8,19.,50.)) ;
#47361 = CARTESIAN_POINT('',(-57.95,18.6413991639922,49.9056313589453)) ;
#47362 = CARTESIAN_POINT('Origin',(-57.8,18.6413991639922,49.9056313589453)) ;
#47363 = CARTESIAN_POINT('Origin',(-57.8,18.6413991639922,49.9056313589453)) ;
#47364 = CARTESIAN_POINT('Origin',(-57.8,19.,68.6)) ;
#47365 = CARTESIAN_POINT('Ctrl Pts',(-57.6860796798847,18.6165653110831,50.)) ;
#47366 = CARTESIAN_POINT('Ctrl Pts',(-57.6886146178473,18.6158121686249,50.0028619413412)) ;
#47367 = CARTESIAN_POINT('Ctrl Pts',(-57.6912408078998,18.6150594333075,50.0055921722713)) ;
#47368 = CARTESIAN_POINT('Ctrl Pts',(-57.7072600366897,18.6106539924209,50.0209974725143)) ;
#47369 = CARTESIAN_POINT('Ctrl Pts',(-57.7241193190454,18.6068199894771,50.0319162690223)) ;
#47370 = CARTESIAN_POINT('Ctrl Pts',(-57.7610636991397,18.6014622194592,50.0463321317631)) ;
#47371 = CARTESIAN_POINT('Ctrl Pts',(-57.7811519935343,18.6,50.0498438108241)) ;
#47372 = CARTESIAN_POINT('Ctrl Pts',(-57.8188480064657,18.6,50.0498438108241)) ;
#47373 = CARTESIAN_POINT('Ctrl Pts',(-57.8389363008603,18.6014622194592,50.0463321317631)) ;
#47374 = CARTESIAN_POINT('Ctrl Pts',(-57.8758806809546,18.6068199894771,50.0319162690223)) ;
#47375 = CARTESIAN_POINT('Ctrl Pts',(-57.8927399633103,18.6106539924209,50.0209974725143)) ;
#47376 = CARTESIAN_POINT('Ctrl Pts',(-57.9087591921002,18.6150594333075,50.0055921722713)) ;
#47377 = CARTESIAN_POINT('Ctrl Pts',(-57.9113853821527,18.6158121686249,50.0028619413412)) ;
#47378 = CARTESIAN_POINT('Ctrl Pts',(-57.9139203201154,18.6165653110831,50.)) ;
#47379 = CARTESIAN_POINT('Origin',(-43.9,0.,44.5)) ;
#47380 = CARTESIAN_POINT('',(-57.8018230872335,0.396772011309262,44.9493181749091)) ;
#47381 = CARTESIAN_POINT('',(-57.7913960076435,0.320489692203214,45.2391909875121)) ;
#47382 = CARTESIAN_POINT('Ctrl Pts',(-57.8018230872335,0.396772011309261,
44.9493181749091)) ;
#47383 = CARTESIAN_POINT('Ctrl Pts',(-57.7838099638155,0.396827731634953,
44.9491064376715)) ;
#47384 = CARTESIAN_POINT('Ctrl Pts',(-57.7648197232592,0.397403006824304,
44.9525521245349)) ;
#47385 = CARTESIAN_POINT('Ctrl Pts',(-57.7285306259727,0.398930598445194,
44.9670570197925)) ;
#47386 = CARTESIAN_POINT('Ctrl Pts',(-57.7113958074383,0.399819549885464,
44.9785768936597)) ;
#47387 = CARTESIAN_POINT('Ctrl Pts',(-57.6840433857854,0.400129413279351,
45.0050225681604)) ;
#47388 = CARTESIAN_POINT('Ctrl Pts',(-57.6719414680996,0.399565898583832,
45.0217756379422)) ;
#47389 = CARTESIAN_POINT('Ctrl Pts',(-57.655291417997,0.395377554048088,45.0582755050382)) ;
#47390 = CARTESIAN_POINT('Ctrl Pts',(-57.650752206554,0.391685614070328,45.078018639465)) ;
#47391 = CARTESIAN_POINT('Ctrl Pts',(-57.6494291476468,0.382006393643826,
45.1147996770857)) ;
#47392 = CARTESIAN_POINT('Ctrl Pts',(-57.6525653247154,0.375434029513804,
45.1340608982685)) ;
#47393 = CARTESIAN_POINT('Ctrl Pts',(-57.6666482059757,0.360841507256248,
45.168928324987)) ;
#47394 = CARTESIAN_POINT('Ctrl Pts',(-57.6775850700919,0.352881735310964,
45.1845637444403)) ;
#47395 = CARTESIAN_POINT('Ctrl Pts',(-57.7030996592059,0.33912667597473,45.2092098145205)) ;
#47396 = CARTESIAN_POINT('Ctrl Pts',(-57.7194346236979,0.332386160750563,
45.2199258830321)) ;
#47397 = CARTESIAN_POINT('Ctrl Pts',(-57.754688260616,0.323283359066371,45.234206786015)) ;
#47398 = CARTESIAN_POINT('Ctrl Pts',(-57.7734112133181,0.320752662206818,
45.2381917014984)) ;
#47399 = CARTESIAN_POINT('Ctrl Pts',(-57.7913960076435,0.320489692203213,
45.2391909875121)) ;
#47400 = CARTESIAN_POINT('Origin',(-57.8,0.,45.)) ;
#47401 = CARTESIAN_POINT('Origin',(-57.8,9.5,47.5)) ;
#47402 = CARTESIAN_POINT('',(-57.95,0.358600836007785,45.0943686410547)) ;
#47403 = CARTESIAN_POINT('',(-57.95,9.5,47.5)) ;
#47404 = CARTESIAN_POINT('Origin',(-57.8,0.358600836007795,45.0943686410547)) ;
#47405 = CARTESIAN_POINT('Origin',(-57.8,0.358600836007795,45.0943686410547)) ;
#47406 = CARTESIAN_POINT('Origin',(-57.8,0.,45.)) ;
#47407 = CARTESIAN_POINT('Origin',(-57.8,19.,50.)) ;
#47408 = CARTESIAN_POINT('',(-57.9139203201153,18.9024184409593,50.3708099243548)) ;
#47409 = CARTESIAN_POINT('',(-57.95,19.,50.3708099243548)) ;
#47410 = CARTESIAN_POINT('Origin',(-57.8,19.,50.3708099243548)) ;
#47411 = CARTESIAN_POINT('',(-57.6860796798847,18.9024184409593,50.3708099243548)) ;
#47412 = CARTESIAN_POINT('Origin',(-57.8,19.,50.)) ;
#47413 = CARTESIAN_POINT('Origin',(-57.8,19.,50.3708099243548)) ;
#47414 = CARTESIAN_POINT('',(-57.8,19.,50.4)) ;
#47415 = CARTESIAN_POINT('Origin',(-57.8,19.,50.)) ;
#47416 = CARTESIAN_POINT('Origin',(-55.6,19.,87.2)) ;
#47417 = CARTESIAN_POINT('',(-57.8,19.15,86.8291900756452)) ;
#47418 = CARTESIAN_POINT('',(-57.8,18.85,86.8291900756452)) ;
#47419 = CARTESIAN_POINT('Ctrl Pts',(-57.8,19.15,86.8291900756452)) ;
#47420 = CARTESIAN_POINT('Ctrl Pts',(-57.7809549836829,19.15,86.8291900756452)) ;
#47421 = CARTESIAN_POINT('Ctrl Pts',(-57.7607852902757,19.1461555423576,86.8275680116987)) ;
#47422 = CARTESIAN_POINT('Ctrl Pts',(-57.7238938323863,19.1307940834772,86.8218995741112)) ;
#47423 = CARTESIAN_POINT('Ctrl Pts',(-57.7071532187349,19.1192852530909,86.8179542005944)) ;
#47424 = CARTESIAN_POINT('Ctrl Pts',(-57.6807248697828,19.0928569041387,86.8106861522654)) ;
#47425 = CARTESIAN_POINT('Ctrl Pts',(-57.6692083147017,19.0761123774726,86.8068656051584)) ;
#47426 = CARTESIAN_POINT('Ctrl Pts',(-57.6538410060698,19.0392059700481,86.8014894752437)) ;
#47427 = CARTESIAN_POINT('Ctrl Pts',(-57.65,19.0190304322447,86.8)) ;
#47428 = CARTESIAN_POINT('Ctrl Pts',(-57.65,18.9809695677553,86.8)) ;
#47429 = CARTESIAN_POINT('Ctrl Pts',(-57.6538410060698,18.9607940299519,86.8014894752437)) ;
#47430 = CARTESIAN_POINT('Ctrl Pts',(-57.6692083147017,18.9238876225274,86.8068656051584)) ;
#47431 = CARTESIAN_POINT('Ctrl Pts',(-57.6807248697828,18.9071430958613,86.8106861522654)) ;
#47432 = CARTESIAN_POINT('Ctrl Pts',(-57.7071532187349,18.8807147469091,86.8179542005944)) ;
#47433 = CARTESIAN_POINT('Ctrl Pts',(-57.7238938323863,18.8692059165228,86.8218995741112)) ;
#47434 = CARTESIAN_POINT('Ctrl Pts',(-57.7607852902757,18.8538444576424,86.8275680116987)) ;
#47435 = CARTESIAN_POINT('Ctrl Pts',(-57.7809549836829,18.85,86.8291900756452)) ;
#47436 = CARTESIAN_POINT('Ctrl Pts',(-57.8,18.85,86.8291900756452)) ;
#47437 = CARTESIAN_POINT('Origin',(-57.8,19.,87.2)) ;
#47438 = CARTESIAN_POINT('Origin',(-57.8,19.,68.6)) ;
#47439 = CARTESIAN_POINT('',(-57.95,19.,86.8291900756452)) ;
#47440 = CARTESIAN_POINT('Origin',(-57.8,19.,86.8291900756452)) ;
#47441 = CARTESIAN_POINT('',(-57.95,19.,68.6)) ;
#47442 = CARTESIAN_POINT('Ctrl Pts',(-57.6860796798847,18.9024184409593,50.3708099243548)) ;
#47443 = CARTESIAN_POINT('Ctrl Pts',(-57.6885032122124,18.8995891197094,50.3708099243548)) ;
#47444 = CARTESIAN_POINT('Ctrl Pts',(-57.6910096124592,18.8968769056013,50.3708402030569)) ;
#47445 = CARTESIAN_POINT('Ctrl Pts',(-57.7069183737083,18.8808606548532,50.3711657794823)) ;
#47446 = CARTESIAN_POINT('Ctrl Pts',(-57.7238219217715,18.869232921536,50.3720978089255)) ;
#47447 = CARTESIAN_POINT('Ctrl Pts',(-57.7608947554465,18.853801818028,50.3736194963427)) ;
#47448 = CARTESIAN_POINT('Ctrl Pts',(-57.7810672966117,18.85,50.3741448990397)) ;
#47449 = CARTESIAN_POINT('Ctrl Pts',(-57.8189327033883,18.85,50.3741448990398)) ;
#47450 = CARTESIAN_POINT('Ctrl Pts',(-57.8391052445535,18.853801818028,50.3736194963427)) ;
#47451 = CARTESIAN_POINT('Ctrl Pts',(-57.8761780782285,18.869232921536,50.3720978089255)) ;
#47452 = CARTESIAN_POINT('Ctrl Pts',(-57.8930816262917,18.8808606548532,50.3711657794824)) ;
#47453 = CARTESIAN_POINT('Ctrl Pts',(-57.9089903875408,18.8968769056013,50.3708402030569)) ;
#47454 = CARTESIAN_POINT('Ctrl Pts',(-57.9114967877876,18.8995891197094,50.3708099243548)) ;
#47455 = CARTESIAN_POINT('Ctrl Pts',(-57.9139203201153,18.9024184409593,50.3708099243548)) ;
#47456 = CARTESIAN_POINT('Origin',(-57.8,19.,86.8291900756452)) ;
#47457 = CARTESIAN_POINT('Origin',(-57.8,9.5,47.5)) ;
#47458 = CARTESIAN_POINT('Origin',(-57.8,19.,87.2)) ;
#47459 = CARTESIAN_POINT('Origin',(-57.8,19.,50.)) ;
#47460 = CARTESIAN_POINT('',(-57.8,19.,49.85)) ;
#47461 = CARTESIAN_POINT('',(-57.8,19.,50.15)) ;
#47462 = CARTESIAN_POINT('Origin',(-57.8,19.,50.)) ;
#47463 = CARTESIAN_POINT('',(0.,0.,0.)) ;
#47464 = CARTESIAN_POINT('Origin',(-13.,0.,43.25)) ;
#47465 = CARTESIAN_POINT('',(-13.,-0.125,43.6)) ;
#47466 = CARTESIAN_POINT('',(-13.1,-0.0749999999999981,43.7)) ;
#47467 = CARTESIAN_POINT('Origin',(-13.,0.,43.6)) ;
#47468 = CARTESIAN_POINT('',(-13.125,-1.53080849893416E-17,43.475)) ;
#47469 = CARTESIAN_POINT('Origin',(-13.,0.,43.6)) ;
#47470 = CARTESIAN_POINT('',(-13.125,-1.53080849893419E-17,42.8)) ;
#47471 = CARTESIAN_POINT('',(-13.125,-1.53080849893419E-17,43.25)) ;
#47472 = CARTESIAN_POINT('Origin',(-13.,0.,42.8)) ;
#47473 = CARTESIAN_POINT('',(-13.,0.125,43.6)) ;
#47474 = CARTESIAN_POINT('Origin',(-13.,0.,43.6)) ;
#47475 = CARTESIAN_POINT('',(-13.1,0.0749999999999981,43.7)) ;
#47476 = CARTESIAN_POINT('Origin',(-13.,0.,43.6)) ;
#47477 = CARTESIAN_POINT('Origin',(-13.,0.,43.7)) ;
#47478 = CARTESIAN_POINT('Origin',(-13.,0.,42.8)) ;
#47479 = CARTESIAN_POINT('Origin',(-13.,0.,43.7)) ;
#47480 = CARTESIAN_POINT('',(-13.,-0.0749999999999981,43.7)) ;
#47481 = CARTESIAN_POINT('',(-15.6,-0.0749999999999981,43.7)) ;
#47482 = CARTESIAN_POINT('',(-13.,0.0749999999999981,43.7)) ;
#47483 = CARTESIAN_POINT('',(-15.6,0.0749999999999981,43.7)) ;
#47484 = CARTESIAN_POINT('',(-13.,0.,43.7)) ;
#47485 = CARTESIAN_POINT('Origin',(-13.,0.,43.6)) ;
#47486 = CARTESIAN_POINT('',(-13.,-1.53080849893419E-17,43.725)) ;
#47487 = CARTESIAN_POINT('Origin',(-13.,0.,43.6)) ;
#47488 = CARTESIAN_POINT('Origin',(-13.,0.,43.6)) ;
#47489 = CARTESIAN_POINT('Origin',(-15.6,0.,43.6)) ;
#47490 = CARTESIAN_POINT('',(-18.2,-1.53080849893419E-17,43.725)) ;
#47491 = CARTESIAN_POINT('',(-15.6,-1.53080849893419E-17,43.725)) ;
#47492 = CARTESIAN_POINT('Origin',(-18.2,0.,43.6)) ;
#47493 = CARTESIAN_POINT('Origin',(-18.2,0.,43.6)) ;
#47494 = CARTESIAN_POINT('Origin',(-53.,19.,88.2)) ;
#47495 = CARTESIAN_POINT('',(-53.125,19.,89.4)) ;
#47496 = CARTESIAN_POINT('Origin',(-53.,19.,89.4)) ;
#47497 = CARTESIAN_POINT('',(-53.125,19.,87.)) ;
#47498 = CARTESIAN_POINT('',(-53.125,19.,88.2)) ;
#47499 = CARTESIAN_POINT('Origin',(-53.,19.,87.)) ;
#47500 = CARTESIAN_POINT('Origin',(-53.,19.,87.)) ;
#47501 = CARTESIAN_POINT('Origin',(-53.,19.,89.4)) ;
#47502 = CARTESIAN_POINT('',(0.,0.,0.)) ;
#47503 = CARTESIAN_POINT('Origin',(-13.,0.,42.6)) ;
#47504 = CARTESIAN_POINT('',(-13.29,-3.55147571752732E-17,42.8)) ;
#47505 = CARTESIAN_POINT('Origin',(-13.,0.,42.8)) ;
#47506 = CARTESIAN_POINT('',(-13.29,-3.55147571752732E-17,42.4)) ;
#47507 = CARTESIAN_POINT('',(-13.29,-3.55147571752732E-17,42.6)) ;
#47508 = CARTESIAN_POINT('Origin',(-13.,0.,42.4)) ;
#47509 = CARTESIAN_POINT('Origin',(-13.,0.,42.4)) ;
#47510 = CARTESIAN_POINT('Origin',(-13.,0.,42.8)) ;
#47511 = CARTESIAN_POINT('',(0.,0.,0.)) ;
#47512 = CARTESIAN_POINT('Origin',(-53.,19.,89.6)) ;
#47513 = CARTESIAN_POINT('',(-53.29,19.,89.8)) ;
#47514 = CARTESIAN_POINT('Origin',(-53.,19.,89.8)) ;
#47515 = CARTESIAN_POINT('',(-53.29,19.,89.4)) ;
#47516 = CARTESIAN_POINT('',(-53.29,19.,89.6)) ;
#47517 = CARTESIAN_POINT('Origin',(-53.,19.,89.4)) ;
#47518 = CARTESIAN_POINT('Origin',(-53.,19.,89.4)) ;
#47519 = CARTESIAN_POINT('Origin',(-53.,19.,89.8)) ;
#47520 = CARTESIAN_POINT('',(0.,0.,0.)) ;
#47521 = CARTESIAN_POINT('Origin',(21.5,0.,43.2)) ;
#47522 = CARTESIAN_POINT('',(20.95,-6.73555739531044E-17,43.6)) ;
#47523 = CARTESIAN_POINT('Origin',(21.5,0.,43.6)) ;
#47524 = CARTESIAN_POINT('',(20.95,-6.73555739531044E-17,42.8)) ;
#47525 = CARTESIAN_POINT('',(20.95,-6.73555739531044E-17,43.2)) ;
#47526 = CARTESIAN_POINT('Origin',(21.5,0.,42.8)) ;
#47527 = CARTESIAN_POINT('',(22.0291502622129,0.149999999999999,43.3279353866634)) ;
#47528 = CARTESIAN_POINT('',(22.05,-5.24397723358717E-16,43.4943625562705)) ;
#47529 = CARTESIAN_POINT('Ctrl Pts',(22.0291502622129,0.149999999999999,43.3279353866634)) ;
#47530 = CARTESIAN_POINT('Ctrl Pts',(22.0291502622129,0.15,43.3482640855675)) ;
#47531 = CARTESIAN_POINT('Ctrl Pts',(22.0302886323727,0.146138210109205,43.3699496533073)) ;
#47532 = CARTESIAN_POINT('Ctrl Pts',(22.0342671466072,0.13084733724015,43.410330079765)) ;
#47533 = CARTESIAN_POINT('Ctrl Pts',(22.0370500041276,0.119426507636106,43.4290336867825)) ;
#47534 = CARTESIAN_POINT('Ctrl Pts',(22.0421962389769,0.0932418857328599,
43.4586176511119)) ;
#47535 = CARTESIAN_POINT('Ctrl Pts',(22.0449278595246,0.0767918256322746,
43.4717830449028)) ;
#47536 = CARTESIAN_POINT('Ctrl Pts',(22.0488606852484,0.0399412858806604,
43.4896777850851)) ;
#47537 = CARTESIAN_POINT('Ctrl Pts',(22.05,0.019512600055463,43.4943625562705)) ;
#47538 = CARTESIAN_POINT('Ctrl Pts',(22.05,1.28369537222284E-16,43.4943625562705)) ;
#47539 = CARTESIAN_POINT('Ctrl Pts',(22.05,-1.07205910815367E-15,43.4943625562705)) ;
#47540 = CARTESIAN_POINT('Ctrl Pts',(22.05,-0.019512600055464,43.4943625562705)) ;
#47541 = CARTESIAN_POINT('Ctrl Pts',(22.0488606852484,-0.0399412858806645,
43.4896777850851)) ;
#47542 = CARTESIAN_POINT('Ctrl Pts',(22.0449278595246,-0.0767918256322786,
43.4717830449028)) ;
#47543 = CARTESIAN_POINT('Ctrl Pts',(22.0421962389769,-0.0932418857328599,
43.4586176511119)) ;
#47544 = CARTESIAN_POINT('Ctrl Pts',(22.0370500041276,-0.119426507636106,
43.4290336867825)) ;
#47545 = CARTESIAN_POINT('Ctrl Pts',(22.0342671466072,-0.13084733724015,43.410330079765)) ;
#47546 = CARTESIAN_POINT('Ctrl Pts',(22.0302886323727,-0.146138210109205,
43.3699496533073)) ;
#47547 = CARTESIAN_POINT('Ctrl Pts',(22.0291502622129,-0.15,43.3482640855675)) ;
#47548 = CARTESIAN_POINT('Ctrl Pts',(22.0291502622129,-0.15,43.308519632144)) ;
#47549 = CARTESIAN_POINT('Ctrl Pts',(22.0302085659904,-0.146426832233699,
43.2877474258495)) ;
#47550 = CARTESIAN_POINT('Ctrl Pts',(22.0341811514524,-0.131196166457133,
43.2497089483429)) ;
#47551 = CARTESIAN_POINT('Ctrl Pts',(22.037037832312,-0.119519687559714,43.2324442857003)) ;
#47552 = CARTESIAN_POINT('Ctrl Pts',(22.0423222675757,-0.0925698332601531,
43.2058565502346)) ;
#47553 = CARTESIAN_POINT('Ctrl Pts',(22.0450738363931,-0.075751613095341,
43.1946402298968)) ;
#47554 = CARTESIAN_POINT('Ctrl Pts',(22.0489379804298,-0.0388701328861759,
43.1798339464663)) ;
#47555 = CARTESIAN_POINT('Ctrl Pts',(22.05,-0.01880894404086,43.1762256790236)) ;
#47556 = CARTESIAN_POINT('Ctrl Pts',(22.05,0.0188089440408599,43.1762256790237)) ;
#47557 = CARTESIAN_POINT('Ctrl Pts',(22.0489379804298,0.038870132886171,43.1798339464663)) ;
#47558 = CARTESIAN_POINT('Ctrl Pts',(22.0450738363931,0.0757516130953385,
43.1946402298968)) ;
#47559 = CARTESIAN_POINT('Ctrl Pts',(22.0423222675757,0.0925698332601531,
43.2058565502346)) ;
#47560 = CARTESIAN_POINT('Ctrl Pts',(22.037037832312,0.119519687559714,43.2324442857003)) ;
#47561 = CARTESIAN_POINT('Ctrl Pts',(22.0341811514524,0.131196166457133,43.2497089483429)) ;
#47562 = CARTESIAN_POINT('Ctrl Pts',(22.0302085659904,0.146426832233699,43.2877474258495)) ;
#47563 = CARTESIAN_POINT('Ctrl Pts',(22.0291502622129,0.15,43.308519632144)) ;
#47564 = CARTESIAN_POINT('Ctrl Pts',(22.0291502622129,0.15,43.3279353866634)) ;
#47565 = CARTESIAN_POINT('Origin',(21.5,0.,43.2)) ;
#47566 = CARTESIAN_POINT('',(21.25,-3.06161699786838E-17,42.8)) ;
#47567 = CARTESIAN_POINT('Origin',(21.5,0.,42.8)) ;
#47568 = CARTESIAN_POINT('',(21.25,3.06161699786838E-17,43.6)) ;
#47569 = CARTESIAN_POINT('',(21.25,-3.06161699786838E-17,43.2)) ;
#47570 = CARTESIAN_POINT('Origin',(21.5,0.,43.6)) ;
#47571 = CARTESIAN_POINT('Origin',(21.5,0.,42.8)) ;
#47572 = CARTESIAN_POINT('Origin',(21.5,0.,43.6)) ;
#47573 = CARTESIAN_POINT('Origin',(22.375,0.,43.45)) ;
#47574 = CARTESIAN_POINT('',(22.7500769823397,-1.83697019872103E-17,43.7414485500374)) ;
#47575 = CARTESIAN_POINT('Origin',(22.8,0.,43.6)) ;
#47576 = CARTESIAN_POINT('',(22.3250769823397,-1.83697019872103E-17,43.5914485500374)) ;
#47577 = CARTESIAN_POINT('Origin',(22.8,0.,43.6)) ;
#47578 = CARTESIAN_POINT('Origin',(22.75,0.,43.6)) ;
#47579 = CARTESIAN_POINT('',(22.6,-9.79717439317883E-17,44.4)) ;
#47580 = CARTESIAN_POINT('Origin',(22.6,0.,43.6)) ;
#47581 = CARTESIAN_POINT('',(22.9,9.79717439317883E-17,44.4)) ;
#47582 = CARTESIAN_POINT('',(22.75,-9.79717439317883E-17,44.4)) ;
#47583 = CARTESIAN_POINT('Origin',(22.9,0.,43.6)) ;
#47584 = CARTESIAN_POINT('Origin',(22.75,0.,43.6)) ;
#47585 = CARTESIAN_POINT('',(22.9,-1.34711147906209E-16,44.7)) ;
#47586 = CARTESIAN_POINT('Origin',(22.9,0.,43.6)) ;
#47587 = CARTESIAN_POINT('',(22.6,-1.34711147906209E-16,44.7)) ;
#47588 = CARTESIAN_POINT('',(22.75,-1.34711147906209E-16,44.7)) ;
#47589 = CARTESIAN_POINT('Origin',(22.6,0.,43.6)) ;
#47590 = CARTESIAN_POINT('Origin',(22.6,0.,43.6)) ;
#47591 = CARTESIAN_POINT('Origin',(22.9,0.,43.6)) ;
#47592 = CARTESIAN_POINT('Origin',(30.55,0.,43.6)) ;
#47593 = CARTESIAN_POINT('',(30.549269378395,0.014786277360407,44.399863342079)) ;
#47594 = CARTESIAN_POINT('',(30.4,-9.79717439317883E-17,44.4)) ;
#47595 = CARTESIAN_POINT('Origin',(33.7324739562774,0.,43.6)) ;
#47596 = CARTESIAN_POINT('',(30.4930138235359,0.576083171705783,44.155092946521)) ;
#47597 = CARTESIAN_POINT('Ctrl Pts',(30.4930138235359,0.576083171705784,44.155092946521)) ;
#47598 = CARTESIAN_POINT('Ctrl Pts',(30.4975561420248,0.544490046590428,44.1878807306833)) ;
#47599 = CARTESIAN_POINT('Ctrl Pts',(30.4989740974443,0.508397435011936,44.2195320006755)) ;
#47600 = CARTESIAN_POINT('Ctrl Pts',(30.5019483280108,0.417669414774168,44.2853318237253)) ;
#47601 = CARTESIAN_POINT('Ctrl Pts',(30.5041008614886,0.360794086722511,44.3164679562894)) ;
#47602 = CARTESIAN_POINT('Ctrl Pts',(30.5149996703933,0.251188800558993,44.3618679523262)) ;
#47603 = CARTESIAN_POINT('Ctrl Pts',(30.5246605716675,0.189242972393476,44.3799145318681)) ;
#47604 = CARTESIAN_POINT('Ctrl Pts',(30.5401014529422,0.0890575887576062,
44.3959153638972)) ;
#47605 = CARTESIAN_POINT('Ctrl Pts',(30.5456292162213,0.0515279069685374,
44.3991841361479)) ;
#47606 = CARTESIAN_POINT('Ctrl Pts',(30.549269378395,0.0147862773604065,44.399863342079)) ;
#47607 = CARTESIAN_POINT('',(30.4367638235359,0.79986230391446,43.5851576694332)) ;
#47608 = CARTESIAN_POINT('Ctrl Pts',(30.4367638235359,0.799862303914459,43.5851576694332)) ;
#47609 = CARTESIAN_POINT('Ctrl Pts',(30.4413061420248,0.800707055427765,43.6306818469624)) ;
#47610 = CARTESIAN_POINT('Ctrl Pts',(30.4427240974443,0.797566552674501,43.6785840050049)) ;
#47611 = CARTESIAN_POINT('Ctrl Pts',(30.4456983280108,0.779939655400098,43.7892659044381)) ;
#47612 = CARTESIAN_POINT('Ctrl Pts',(30.4478508614886,0.761739295728619,43.8514994050616)) ;
#47613 = CARTESIAN_POINT('Ctrl Pts',(30.4587496703933,0.716339299691906,43.9611046912252)) ;
#47614 = CARTESIAN_POINT('Ctrl Pts',(30.4684105716675,0.685297843301198,44.0176678651586)) ;
#47615 = CARTESIAN_POINT('Ctrl Pts',(30.4838485444283,0.625781588850216,44.0998084508506)) ;
#47616 = CARTESIAN_POINT('Ctrl Pts',(30.4893735852195,0.601568925505817,44.1286434771584)) ;
#47617 = CARTESIAN_POINT('Ctrl Pts',(30.4930138235359,0.576083171705781,44.155092946521)) ;
#47618 = CARTESIAN_POINT('',(30.4,0.749934102053461,43.3214343119168)) ;
#47619 = CARTESIAN_POINT('Ctrl Pts',(30.4,0.749934102053461,43.3214343119168)) ;
#47620 = CARTESIAN_POINT('Ctrl Pts',(30.405505133701,0.767659246796581,43.3691526457797)) ;
#47621 = CARTESIAN_POINT('Ctrl Pts',(30.4137552132925,0.781567001849141,43.4211035732546)) ;
#47622 = CARTESIAN_POINT('Ctrl Pts',(30.4275985444283,0.795912349908512,43.5109235398731)) ;
#47623 = CARTESIAN_POINT('Ctrl Pts',(30.4331235852195,0.799180854104993,43.5484339209525)) ;
#47624 = CARTESIAN_POINT('Ctrl Pts',(30.4367638235359,0.79986230391446,43.5851576694333)) ;
#47625 = CARTESIAN_POINT('Origin',(30.4,0.,43.6)) ;
#47626 = CARTESIAN_POINT('',(30.7,9.79717439317883E-17,44.4)) ;
#47627 = CARTESIAN_POINT('',(30.55,-9.79717439317883E-17,44.4)) ;
#47628 = CARTESIAN_POINT('Origin',(30.7,0.,43.6)) ;
#47629 = CARTESIAN_POINT('Origin',(30.55,0.,43.6)) ;
#47630 = CARTESIAN_POINT('',(30.7,-1.34711147906209E-16,44.7)) ;
#47631 = CARTESIAN_POINT('Origin',(30.7,0.,43.6)) ;
#47632 = CARTESIAN_POINT('',(30.4,-1.34711147906209E-16,44.7)) ;
#47633 = CARTESIAN_POINT('',(30.55,-1.34711147906209E-16,44.7)) ;
#47634 = CARTESIAN_POINT('Origin',(30.4,0.,43.6)) ;
#47635 = CARTESIAN_POINT('Origin',(30.4,0.,43.6)) ;
#47636 = CARTESIAN_POINT('',(30.4,0.0574025148547688,44.5385819298767)) ;
#47637 = CARTESIAN_POINT('',(30.4,-0.141421356237311,44.0585786437627)) ;
#47638 = CARTESIAN_POINT('',(30.4,0.887209576122323,43.5526899605521)) ;
#47639 = CARTESIAN_POINT('Origin',(30.4,1.26862915010156,44.7313708498986)) ;
#47640 = CARTESIAN_POINT('',(30.4,0.895119732372327,43.6282132329487)) ;
#47641 = CARTESIAN_POINT('Origin',(30.4,0.8,43.6)) ;
#47642 = CARTESIAN_POINT('',(30.4,0.696043110499698,44.2140880211392)) ;
#47643 = CARTESIAN_POINT('Origin',(30.4,0.331370849898448,44.7313708498985)) ;
#47644 = CARTESIAN_POINT('',(30.4,0.623636424388808,44.2920880323747)) ;
#47645 = CARTESIAN_POINT('Origin',(30.4,0.565685424949239,44.1656854249492)) ;
#47646 = CARTESIAN_POINT('Origin',(30.4,-1.47659662275146E-14,44.4)) ;
#47647 = CARTESIAN_POINT('Origin',(30.7,0.,43.6)) ;
#47648 = CARTESIAN_POINT('Origin',(30.4,3.05311331771918E-15,44.4)) ;
#47649 = CARTESIAN_POINT('Origin',(30.4,3.05311331771918E-15,44.4)) ;
#47650 = CARTESIAN_POINT('Origin',(30.34375,0.565685424949239,44.1656854249492)) ;
#47651 = CARTESIAN_POINT('',(30.1944861227066,0.555190308577042,44.1761805413214)) ;
#47652 = CARTESIAN_POINT('Origin',(30.34375,0.565685424949239,44.1656854249492)) ;
#47653 = CARTESIAN_POINT('Origin',(30.34375,0.565685424949239,44.1656854249492)) ;
#47654 = CARTESIAN_POINT('Origin',(30.2875,0.8,43.6)) ;
#47655 = CARTESIAN_POINT('',(30.1381289970792,0.805251324321435,43.6126778183972)) ;
#47656 = CARTESIAN_POINT('Origin',(30.2875,0.8,43.6)) ;
#47657 = CARTESIAN_POINT('',(30.1382361227066,0.799999999999998,43.6148423359122)) ;
#47658 = CARTESIAN_POINT('Origin',(30.2875,0.8,43.6)) ;
#47659 = CARTESIAN_POINT('Origin',(30.2875,0.8,43.6)) ;
#47660 = CARTESIAN_POINT('Origin',(30.23125,0.565685424949232,43.0343145750508)) ;
#47661 = CARTESIAN_POINT('',(30.0819861227066,0.576180541321441,43.0448096914229)) ;
#47662 = CARTESIAN_POINT('',(30.3805138772934,0.55519030857705,43.0238194586786)) ;
#47663 = CARTESIAN_POINT('Origin',(30.23125,0.565685424949232,43.0343145750508)) ;
#47664 = CARTESIAN_POINT('',(30.0818789970792,0.57836324334647,43.0395658993722)) ;
#47665 = CARTESIAN_POINT('Origin',(30.23125,0.565685424949232,43.0343145750508)) ;
#47666 = CARTESIAN_POINT('Origin',(30.23125,0.565685424949232,43.0343145750508)) ;
#47667 = CARTESIAN_POINT('Origin',(30.175,-5.87929500492584E-15,42.8)) ;
#47668 = CARTESIAN_POINT('',(30.0257361227066,0.0148423359122354,42.8)) ;
#47669 = CARTESIAN_POINT('',(30.3242638772934,-0.014842335912247,42.8)) ;
#47670 = CARTESIAN_POINT('Origin',(30.175,-5.88418203051333E-15,42.8)) ;
#47671 = CARTESIAN_POINT('',(30.0291439534833,-5.89715721897613E-15,42.7649855216442)) ;
#47672 = CARTESIAN_POINT('Origin',(30.175,-5.82867087928207E-15,42.8)) ;
#47673 = CARTESIAN_POINT('',(30.175,-5.87929500492584E-15,42.65)) ;
#47674 = CARTESIAN_POINT('Origin',(30.175,-5.87929500492584E-15,42.8)) ;
#47675 = CARTESIAN_POINT('',(30.0256289970792,0.0126778183972199,42.7947486756786)) ;
#47676 = CARTESIAN_POINT('Origin',(30.175,-5.82867087928207E-15,42.8)) ;
#47677 = CARTESIAN_POINT('Origin',(30.175,-5.82867087928207E-15,42.8)) ;
#47678 = CARTESIAN_POINT('Origin',(30.11875,-0.565685424949241,43.0343145750508)) ;
#47679 = CARTESIAN_POINT('',(29.9694861227066,-0.555190308577047,43.0238194586786)) ;
#47680 = CARTESIAN_POINT('',(30.2680138772934,-0.576180541321434,43.044809691423)) ;
#47681 = CARTESIAN_POINT('Origin',(30.11875,-0.565685424949241,43.0343145750508)) ;
#47682 = CARTESIAN_POINT('',(29.9693789970792,-0.560434100627805,43.0216367566535)) ;
#47683 = CARTESIAN_POINT('Origin',(30.11875,-0.565685424949241,43.0343145750508)) ;
#47684 = CARTESIAN_POINT('Origin',(30.11875,-0.565685424949241,43.0343145750508)) ;
#47685 = CARTESIAN_POINT('Origin',(30.0625,-0.8,43.6)) ;
#47686 = CARTESIAN_POINT('',(29.9132361227066,-0.799999999999999,43.5851576640878)) ;
#47687 = CARTESIAN_POINT('',(30.2117638772934,-0.800000000000001,43.6148423359122)) ;
#47688 = CARTESIAN_POINT('Origin',(30.0625,-0.8,43.6)) ;
#47689 = CARTESIAN_POINT('',(29.9131289970792,-0.805251324321434,43.5873221816028)) ;
#47690 = CARTESIAN_POINT('Origin',(30.0625,-0.8,43.6)) ;
#47691 = CARTESIAN_POINT('Origin',(30.0625,-0.8,43.6)) ;
#47692 = CARTESIAN_POINT('Origin',(30.00625,-0.565685424949238,44.1656854249492)) ;
#47693 = CARTESIAN_POINT('',(29.8569861227066,-0.576180541321436,44.155190308577)) ;
#47694 = CARTESIAN_POINT('',(30.1555138772934,-0.555190308577049,44.1761805413214)) ;
#47695 = CARTESIAN_POINT('Origin',(30.00625,-0.565685424949238,44.1656854249492)) ;
#47696 = CARTESIAN_POINT('',(29.8568789970792,-0.578363243346471,44.1604341006278)) ;
#47697 = CARTESIAN_POINT('Origin',(30.00625,-0.565685424949238,44.1656854249492)) ;
#47698 = CARTESIAN_POINT('Origin',(30.00625,-0.565685424949238,44.1656854249492)) ;
#47699 = CARTESIAN_POINT('Origin',(29.95,8.62349420403445E-15,44.4)) ;
#47700 = CARTESIAN_POINT('',(29.8007361227066,-0.0148423359122325,44.4)) ;
#47701 = CARTESIAN_POINT('',(30.0992638772934,0.0148423359122498,44.4)) ;
#47702 = CARTESIAN_POINT('Origin',(29.95,8.65973959207622E-15,44.4)) ;
#47703 = CARTESIAN_POINT('',(29.8041439534833,8.60563198998416E-15,44.4350144783558)) ;
#47704 = CARTESIAN_POINT('Origin',(29.95,8.65973959207622E-15,44.4)) ;
#47705 = CARTESIAN_POINT('',(29.95,8.62349420403445E-15,44.55)) ;
#47706 = CARTESIAN_POINT('Origin',(29.95,8.62349420403445E-15,44.4)) ;
#47707 = CARTESIAN_POINT('',(29.8006289970792,-0.0126778183972173,44.4052513243214)) ;
#47708 = CARTESIAN_POINT('Origin',(29.95,8.65973959207622E-15,44.4)) ;
#47709 = CARTESIAN_POINT('Origin',(29.95,8.65973959207622E-15,44.4)) ;
#47710 = CARTESIAN_POINT('Origin',(29.89375,0.565685424949243,44.1656854249492)) ;
#47711 = CARTESIAN_POINT('',(29.7444861227066,0.555190308577048,44.1761805413214)) ;
#47712 = CARTESIAN_POINT('',(30.0430138772934,0.576180541321437,44.155190308577)) ;
#47713 = CARTESIAN_POINT('Origin',(29.89375,0.565685424949243,44.1656854249492)) ;
#47714 = CARTESIAN_POINT('',(29.7443789970792,0.560434100627808,44.1783632433465)) ;
#47715 = CARTESIAN_POINT('Origin',(29.89375,0.565685424949242,44.1656854249492)) ;
#47716 = CARTESIAN_POINT('Origin',(29.89375,0.565685424949242,44.1656854249492)) ;
#47717 = CARTESIAN_POINT('Origin',(29.8375,0.8,43.6)) ;
#47718 = CARTESIAN_POINT('',(29.6882361227066,0.8,43.6148423359122)) ;
#47719 = CARTESIAN_POINT('',(29.9867638772934,0.799999999999997,43.5851576640878)) ;
#47720 = CARTESIAN_POINT('Origin',(29.8375,0.8,43.6)) ;
#47721 = CARTESIAN_POINT('',(29.6881289970792,0.805251324321436,43.6126778183972)) ;
#47722 = CARTESIAN_POINT('Origin',(29.8375,0.8,43.6)) ;
#47723 = CARTESIAN_POINT('Origin',(29.8375,0.8,43.6)) ;
#47724 = CARTESIAN_POINT('Origin',(29.78125,0.565685424949237,43.0343145750508)) ;
#47725 = CARTESIAN_POINT('',(29.6319861227066,0.576180541321439,43.0448096914229)) ;
#47726 = CARTESIAN_POINT('',(29.9305138772934,0.555190308577052,43.0238194586786)) ;
#47727 = CARTESIAN_POINT('Origin',(29.78125,0.565685424949237,43.0343145750508)) ;
#47728 = CARTESIAN_POINT('',(29.6318789970792,0.578363243346468,43.0395658993722)) ;
#47729 = CARTESIAN_POINT('Origin',(29.78125,0.565685424949237,43.0343145750508)) ;
#47730 = CARTESIAN_POINT('Origin',(29.78125,0.565685424949237,43.0343145750508)) ;
#47731 = CARTESIAN_POINT('Origin',(29.725,9.90369018541372E-19,42.8)) ;
#47732 = CARTESIAN_POINT('',(29.5757361227066,0.0148423359122408,42.8)) ;
#47733 = CARTESIAN_POINT('',(29.8742638772934,-0.0148423359122408,42.8)) ;
#47734 = CARTESIAN_POINT('Origin',(29.725,-5.55111512312578E-17,42.8)) ;
#47735 = CARTESIAN_POINT('',(29.5791439534833,-1.68718450317509E-17,42.7649855216442)) ;
#47736 = CARTESIAN_POINT('Origin',(29.725,5.55111512312578E-17,42.8)) ;
#47737 = CARTESIAN_POINT('',(29.725,9.90369018541371E-19,42.65)) ;
#47738 = CARTESIAN_POINT('Origin',(29.725,9.90369018541372E-19,42.8)) ;
#47739 = CARTESIAN_POINT('',(29.5756289970792,0.0126778183972255,42.7947486756786)) ;
#47740 = CARTESIAN_POINT('Origin',(29.725,5.55111512312578E-17,42.8)) ;
#47741 = CARTESIAN_POINT('Origin',(29.725,5.55111512312578E-17,42.8)) ;
#47742 = CARTESIAN_POINT('Origin',(29.66875,-0.565685424949237,43.0343145750508)) ;
#47743 = CARTESIAN_POINT('',(29.5194861227066,-0.555190308577044,43.0238194586786)) ;
#47744 = CARTESIAN_POINT('',(29.8180138772934,-0.576180541321431,43.044809691423)) ;
#47745 = CARTESIAN_POINT('Origin',(29.66875,-0.565685424949237,43.0343145750508)) ;
#47746 = CARTESIAN_POINT('',(29.5193789970792,-0.5604341006278,43.0216367566535)) ;
#47747 = CARTESIAN_POINT('Origin',(29.66875,-0.565685424949237,43.0343145750508)) ;
#47748 = CARTESIAN_POINT('Origin',(29.66875,-0.565685424949237,43.0343145750508)) ;
#47749 = CARTESIAN_POINT('Origin',(29.6125,-0.8,43.6)) ;
#47750 = CARTESIAN_POINT('',(29.4632361227066,-0.800000000000003,43.5851576640878)) ;
#47751 = CARTESIAN_POINT('',(29.7617638772934,-0.800000000000005,43.6148423359123)) ;
#47752 = CARTESIAN_POINT('Origin',(29.6125,-0.8,43.6)) ;
#47753 = CARTESIAN_POINT('',(29.4631289970792,-0.805251324321435,43.5873221816028)) ;
#47754 = CARTESIAN_POINT('Origin',(29.6125,-0.8,43.6)) ;
#47755 = CARTESIAN_POINT('Origin',(29.6125,-0.8,43.6)) ;
#47756 = CARTESIAN_POINT('Origin',(29.55625,-0.565685424949235,44.1656854249492)) ;
#47757 = CARTESIAN_POINT('',(29.4069861227066,-0.57618054132143,44.155190308577)) ;
#47758 = CARTESIAN_POINT('',(29.7055138772934,-0.555190308577039,44.1761805413214)) ;
#47759 = CARTESIAN_POINT('Origin',(29.55625,-0.565685424949234,44.1656854249492)) ;
#47760 = CARTESIAN_POINT('',(29.4068789970792,-0.578363243346462,44.1604341006278)) ;
#47761 = CARTESIAN_POINT('Origin',(29.55625,-0.565685424949235,44.1656854249492)) ;
#47762 = CARTESIAN_POINT('Origin',(29.55625,-0.565685424949235,44.1656854249492)) ;
#47763 = CARTESIAN_POINT('Origin',(29.5,2.74320883009007E-15,44.4)) ;
#47764 = CARTESIAN_POINT('',(29.3507361227066,-0.0148423359122402,44.4)) ;
#47765 = CARTESIAN_POINT('',(29.6492638772934,0.0148423359122423,44.4)) ;
#47766 = CARTESIAN_POINT('Origin',(29.5,2.83106871279415E-15,44.4)) ;
#47767 = CARTESIAN_POINT('',(29.3541439534833,2.72534661603978E-15,44.4350144783558)) ;
#47768 = CARTESIAN_POINT('Origin',(29.5,2.72004641033163E-15,44.4)) ;
#47769 = CARTESIAN_POINT('',(29.5,2.74320883009007E-15,44.55)) ;
#47770 = CARTESIAN_POINT('Origin',(29.5,2.74320883009007E-15,44.4)) ;
#47771 = CARTESIAN_POINT('',(29.3506289970792,-0.0126778183972286,44.4052513243214)) ;
#47772 = CARTESIAN_POINT('Origin',(29.5,2.72004641033163E-15,44.4)) ;
#47773 = CARTESIAN_POINT('Origin',(29.5,2.72004641033163E-15,44.4)) ;
#47774 = CARTESIAN_POINT('Origin',(29.44375,0.565685424949238,44.1656854249492)) ;
#47775 = CARTESIAN_POINT('',(29.2944861227066,0.555190308577043,44.1761805413214)) ;
#47776 = CARTESIAN_POINT('',(29.5930138772934,0.576180541321431,44.155190308577)) ;
#47777 = CARTESIAN_POINT('Origin',(29.44375,0.565685424949238,44.1656854249492)) ;
#47778 = CARTESIAN_POINT('',(29.2943789970792,0.560434100627805,44.1783632433465)) ;
#47779 = CARTESIAN_POINT('Origin',(29.44375,0.565685424949238,44.1656854249492)) ;
#47780 = CARTESIAN_POINT('Origin',(29.44375,0.565685424949238,44.1656854249492)) ;
#47781 = CARTESIAN_POINT('Origin',(29.3875,0.8,43.6)) ;
#47782 = CARTESIAN_POINT('',(29.2382361227066,0.799999999999999,43.6148423359122)) ;
#47783 = CARTESIAN_POINT('',(29.5367638772934,0.799999999999997,43.5851576640878)) ;
#47784 = CARTESIAN_POINT('Origin',(29.3875,0.8,43.6)) ;
#47785 = CARTESIAN_POINT('',(29.2381289970792,0.805251324321435,43.6126778183972)) ;
#47786 = CARTESIAN_POINT('Origin',(29.3875,0.8,43.6)) ;
#47787 = CARTESIAN_POINT('Origin',(29.3875,0.8,43.6)) ;
#47788 = CARTESIAN_POINT('Origin',(29.33125,0.565685424949233,43.0343145750508)) ;
#47789 = CARTESIAN_POINT('',(29.1819861227066,0.576180541321431,43.044809691423)) ;
#47790 = CARTESIAN_POINT('',(29.4805138772934,0.555190308577043,43.0238194586786)) ;
#47791 = CARTESIAN_POINT('Origin',(29.33125,0.565685424949233,43.0343145750508)) ;
#47792 = CARTESIAN_POINT('',(29.1818789970792,0.578363243346465,43.0395658993722)) ;
#47793 = CARTESIAN_POINT('Origin',(29.33125,0.565685424949233,43.0343145750508)) ;
#47794 = CARTESIAN_POINT('Origin',(29.33125,0.565685424949233,43.0343145750508)) ;
#47795 = CARTESIAN_POINT('Origin',(29.275,-5.48740802919868E-15,42.8)) ;
#47796 = CARTESIAN_POINT('',(29.1257361227066,0.0148423359122358,42.8)) ;
#47797 = CARTESIAN_POINT('',(29.4242638772934,-0.0148423359122466,42.8)) ;
#47798 = CARTESIAN_POINT('Origin',(29.275,-5.44009282066327E-15,42.8)) ;
#47799 = CARTESIAN_POINT('',(29.1291439534833,-5.50527024324898E-15,42.7649855216442)) ;
#47800 = CARTESIAN_POINT('Origin',(29.275,-5.38458166943201E-15,42.8)) ;
#47801 = CARTESIAN_POINT('',(29.275,-5.48740802919868E-15,42.65)) ;
#47802 = CARTESIAN_POINT('Origin',(29.275,-5.48740802919868E-15,42.8)) ;
#47803 = CARTESIAN_POINT('',(29.1256289970792,0.012677818397221,42.7947486756786)) ;
#47804 = CARTESIAN_POINT('Origin',(29.275,-5.38458166943201E-15,42.8)) ;
#47805 = CARTESIAN_POINT('Origin',(29.275,-5.38458166943201E-15,42.8)) ;
#47806 = CARTESIAN_POINT('Origin',(29.21875,-0.56568542494924,43.0343145750508)) ;
#47807 = CARTESIAN_POINT('',(29.0694861227066,-0.555190308577045,43.0238194586786)) ;
#47808 = CARTESIAN_POINT('',(29.3680138772934,-0.576180541321436,43.044809691423)) ;
#47809 = CARTESIAN_POINT('Origin',(29.21875,-0.56568542494924,43.0343145750508)) ;
#47810 = CARTESIAN_POINT('',(29.0693789970792,-0.560434100627806,43.0216367566535)) ;
#47811 = CARTESIAN_POINT('Origin',(29.21875,-0.56568542494924,43.0343145750508)) ;
#47812 = CARTESIAN_POINT('Origin',(29.21875,-0.56568542494924,43.0343145750508)) ;
#47813 = CARTESIAN_POINT('Origin',(29.1625,-0.8,43.6)) ;
#47814 = CARTESIAN_POINT('',(29.0132361227066,-0.8,43.5851576640878)) ;
#47815 = CARTESIAN_POINT('',(29.3117638772934,-0.8,43.6148423359123)) ;
#47816 = CARTESIAN_POINT('Origin',(29.1625,-0.8,43.6)) ;
#47817 = CARTESIAN_POINT('',(29.0131289970792,-0.805251324321434,43.5873221816028)) ;
#47818 = CARTESIAN_POINT('Origin',(29.1625,-0.8,43.6)) ;
#47819 = CARTESIAN_POINT('Origin',(29.1625,-0.8,43.6)) ;
#47820 = CARTESIAN_POINT('Origin',(29.10625,-0.565685424949239,44.1656854249492)) ;
#47821 = CARTESIAN_POINT('',(28.9569861227066,-0.576180541321438,44.155190308577)) ;
#47822 = CARTESIAN_POINT('',(29.2555138772934,-0.555190308577048,44.1761805413214)) ;
#47823 = CARTESIAN_POINT('Origin',(29.10625,-0.565685424949239,44.1656854249492)) ;
#47824 = CARTESIAN_POINT('',(28.9568789970792,-0.578363243346472,44.1604341006278)) ;
#47825 = CARTESIAN_POINT('Origin',(29.10625,-0.565685424949239,44.1656854249492)) ;
#47826 = CARTESIAN_POINT('Origin',(29.10625,-0.565685424949239,44.1656854249492)) ;
#47827 = CARTESIAN_POINT('Origin',(29.05,-3.13707654385431E-15,44.4)) ;
#47828 = CARTESIAN_POINT('',(28.9007361227066,-0.0148423359122443,44.4)) ;
#47829 = CARTESIAN_POINT('',(29.1992638772934,0.014842335912238,44.4)) ;
#47830 = CARTESIAN_POINT('Origin',(29.05,-3.05311331771918E-15,44.4)) ;
#47831 = CARTESIAN_POINT('',(28.9041439534833,-3.1549387579046E-15,44.4350144783558)) ;
#47832 = CARTESIAN_POINT('Origin',(29.05,-3.1641356201817E-15,44.4)) ;
#47833 = CARTESIAN_POINT('',(29.05,-3.13707654385431E-15,44.55)) ;
#47834 = CARTESIAN_POINT('Origin',(29.05,-3.13707654385431E-15,44.4)) ;
#47835 = CARTESIAN_POINT('',(28.9006289970792,-0.0126778183972283,44.4052513243214)) ;
#47836 = CARTESIAN_POINT('Origin',(29.05,-3.1641356201817E-15,44.4)) ;
#47837 = CARTESIAN_POINT('Origin',(29.05,-3.1641356201817E-15,44.4)) ;
#47838 = CARTESIAN_POINT('Origin',(28.99375,0.565685424949242,44.1656854249492)) ;
#47839 = CARTESIAN_POINT('',(28.8444861227066,0.55519030857705,44.1761805413214)) ;
#47840 = CARTESIAN_POINT('',(29.1430138772934,0.576180541321436,44.155190308577)) ;
#47841 = CARTESIAN_POINT('Origin',(28.99375,0.565685424949242,44.1656854249492)) ;
#47842 = CARTESIAN_POINT('',(28.8443789970792,0.560434100627807,44.1783632433465)) ;
#47843 = CARTESIAN_POINT('Origin',(28.99375,0.565685424949242,44.1656854249492)) ;
#47844 = CARTESIAN_POINT('Origin',(28.99375,0.565685424949242,44.1656854249492)) ;
#47845 = CARTESIAN_POINT('Origin',(28.9375,0.8,43.6)) ;
#47846 = CARTESIAN_POINT('',(28.7882361227066,0.799999999999998,43.6148423359122)) ;
#47847 = CARTESIAN_POINT('',(29.0867638772934,0.799999999999999,43.5851576640878)) ;
#47848 = CARTESIAN_POINT('Origin',(28.9375,0.8,43.6)) ;
#47849 = CARTESIAN_POINT('',(28.7881289970792,0.805251324321436,43.6126778183972)) ;
#47850 = CARTESIAN_POINT('Origin',(28.9375,0.8,43.6)) ;
#47851 = CARTESIAN_POINT('Origin',(28.9375,0.8,43.6)) ;
#47852 = CARTESIAN_POINT('Origin',(28.88125,0.565685424949237,43.0343145750508)) ;
#47853 = CARTESIAN_POINT('',(28.7319861227066,0.576180541321439,43.0448096914229)) ;
#47854 = CARTESIAN_POINT('',(29.0305138772934,0.555190308577051,43.0238194586786)) ;
#47855 = CARTESIAN_POINT('Origin',(28.88125,0.565685424949237,43.0343145750508)) ;
#47856 = CARTESIAN_POINT('',(28.7318789970792,0.578363243346472,43.0395658993722)) ;
#47857 = CARTESIAN_POINT('Origin',(28.88125,0.565685424949237,43.0343145750508)) ;
#47858 = CARTESIAN_POINT('Origin',(28.88125,0.565685424949237,43.0343145750508)) ;
#47859 = CARTESIAN_POINT('Origin',(28.825,3.92877344745694E-16,42.8)) ;
#47860 = CARTESIAN_POINT('',(28.6757361227066,0.0148423359122434,42.8)) ;
#47861 = CARTESIAN_POINT('',(28.9742638772934,-0.0148423359122391,42.8)) ;
#47862 = CARTESIAN_POINT('Origin',(28.825,4.44089209850063E-16,42.8)) ;
#47863 = CARTESIAN_POINT('',(28.6791439534833,3.75015130695402E-16,42.7649855216442)) ;
#47864 = CARTESIAN_POINT('Origin',(28.825,4.44089209850063E-16,42.8)) ;
#47865 = CARTESIAN_POINT('',(28.825,3.92877344745694E-16,42.65)) ;
#47866 = CARTESIAN_POINT('Origin',(28.825,3.92877344745694E-16,42.8)) ;
#47867 = CARTESIAN_POINT('',(28.6756289970792,0.0126778183972335,42.7947486756786)) ;
#47868 = CARTESIAN_POINT('Origin',(28.825,4.44089209850063E-16,42.8)) ;
#47869 = CARTESIAN_POINT('Origin',(28.825,4.44089209850063E-16,42.8)) ;
#47870 = CARTESIAN_POINT('Origin',(28.76875,-0.565685424949236,43.0343145750508)) ;
#47871 = CARTESIAN_POINT('',(28.6194861227066,-0.555190308577039,43.0238194586786)) ;
#47872 = CARTESIAN_POINT('',(28.9180138772934,-0.57618054132143,43.044809691423)) ;
#47873 = CARTESIAN_POINT('Origin',(28.76875,-0.565685424949236,43.0343145750508)) ;
#47874 = CARTESIAN_POINT('',(28.6193789970792,-0.560434100627803,43.0216367566535)) ;
#47875 = CARTESIAN_POINT('Origin',(28.76875,-0.565685424949236,43.0343145750508)) ;
#47876 = CARTESIAN_POINT('Origin',(28.76875,-0.565685424949236,43.0343145750508)) ;
#47877 = CARTESIAN_POINT('Origin',(28.7125,-0.8,43.6)) ;
#47878 = CARTESIAN_POINT('',(28.5632361227066,-0.800000000000002,43.5851576640878)) ;
#47879 = CARTESIAN_POINT('',(28.8617638772934,-0.799999999999998,43.6148423359123)) ;
#47880 = CARTESIAN_POINT('Origin',(28.7125,-0.8,43.6)) ;
#47881 = CARTESIAN_POINT('',(28.5631289970792,-0.805251324321435,43.5873221816028)) ;
#47882 = CARTESIAN_POINT('Origin',(28.7125,-0.8,43.6)) ;
#47883 = CARTESIAN_POINT('Origin',(28.7125,-0.8,43.6)) ;
#47884 = CARTESIAN_POINT('Origin',(28.65625,-0.565685424949235,44.1656854249492)) ;
#47885 = CARTESIAN_POINT('',(28.5069861227066,-0.576180541321428,44.155190308577)) ;
#47886 = CARTESIAN_POINT('',(28.8055138772934,-0.555190308577041,44.1761805413214)) ;
#47887 = CARTESIAN_POINT('Origin',(28.65625,-0.565685424949235,44.1656854249492)) ;
#47888 = CARTESIAN_POINT('',(28.5068789970792,-0.57836324334646,44.1604341006278)) ;
#47889 = CARTESIAN_POINT('Origin',(28.65625,-0.565685424949235,44.1656854249492)) ;
#47890 = CARTESIAN_POINT('Origin',(28.65625,-0.565685424949235,44.1656854249492)) ;
#47891 = CARTESIAN_POINT('Origin',(28.6,2.35132185436292E-15,44.4)) ;
#47892 = CARTESIAN_POINT('',(28.4507361227066,-0.0148423359122402,44.4)) ;
#47893 = CARTESIAN_POINT('',(28.7492638772934,0.0148423359122414,44.4)) ;
#47894 = CARTESIAN_POINT('Origin',(28.6,2.38697950294409E-15,44.4)) ;
#47895 = CARTESIAN_POINT('',(28.4541439534833,2.33345964031263E-15,44.4350144783558)) ;
#47896 = CARTESIAN_POINT('Origin',(28.6,2.27595720048157E-15,44.4)) ;
#47897 = CARTESIAN_POINT('',(28.6,2.35132185436292E-15,44.55)) ;
#47898 = CARTESIAN_POINT('Origin',(28.6,2.35132185436292E-15,44.4)) ;
#47899 = CARTESIAN_POINT('',(28.4506289970792,-0.0126778183972291,44.4052513243214)) ;
#47900 = CARTESIAN_POINT('Origin',(28.6,2.27595720048157E-15,44.4)) ;
#47901 = CARTESIAN_POINT('Origin',(28.6,2.27595720048157E-15,44.4)) ;
#47902 = CARTESIAN_POINT('Origin',(28.54375,0.565685424949238,44.1656854249492)) ;
#47903 = CARTESIAN_POINT('',(28.3944861227066,0.555190308577043,44.1761805413214)) ;
#47904 = CARTESIAN_POINT('',(28.6930138772934,0.57618054132143,44.155190308577)) ;
#47905 = CARTESIAN_POINT('Origin',(28.54375,0.565685424949238,44.1656854249492)) ;
#47906 = CARTESIAN_POINT('',(28.3943789970792,0.560434100627804,44.1783632433465)) ;
#47907 = CARTESIAN_POINT('Origin',(28.54375,0.565685424949238,44.1656854249492)) ;
#47908 = CARTESIAN_POINT('Origin',(28.54375,0.565685424949238,44.1656854249492)) ;
#47909 = CARTESIAN_POINT('Origin',(28.4875,0.8,43.6)) ;
#47910 = CARTESIAN_POINT('',(28.3382361227066,0.799999999999997,43.6148423359122)) ;
#47911 = CARTESIAN_POINT('',(28.6367638772934,0.8,43.5851576640878)) ;
#47912 = CARTESIAN_POINT('Origin',(28.4875,0.8,43.6)) ;
#47913 = CARTESIAN_POINT('',(28.3381289970792,0.805251324321436,43.6126778183972)) ;
#47914 = CARTESIAN_POINT('Origin',(28.4875,0.8,43.6)) ;
#47915 = CARTESIAN_POINT('Origin',(28.4875,0.8,43.6)) ;
#47916 = CARTESIAN_POINT('Origin',(28.43125,0.565685424949233,43.0343145750508)) ;
#47917 = CARTESIAN_POINT('',(28.2819861227066,0.576180541321441,43.0448096914229)) ;
#47918 = CARTESIAN_POINT('',(28.5805138772934,0.555190308577051,43.0238194586786)) ;
#47919 = CARTESIAN_POINT('Origin',(28.43125,0.565685424949233,43.0343145750508)) ;
#47920 = CARTESIAN_POINT('',(28.2818789970792,0.57836324334647,43.0395658993722)) ;
#47921 = CARTESIAN_POINT('Origin',(28.43125,0.565685424949233,43.0343145750508)) ;
#47922 = CARTESIAN_POINT('Origin',(28.43125,0.565685424949233,43.0343145750508)) ;
#47923 = CARTESIAN_POINT('Origin',(28.375,-5.09552105347153E-15,42.8)) ;
#47924 = CARTESIAN_POINT('',(28.2257361227066,0.0148423359122326,42.8)) ;
#47925 = CARTESIAN_POINT('',(28.5242638772934,-0.0148423359122499,42.8)) ;
#47926 = CARTESIAN_POINT('Origin',(28.375,-5.10702591327572E-15,42.8)) ;
#47927 = CARTESIAN_POINT('',(28.2291439534833,-5.11338326752182E-15,42.7649855216442)) ;
#47928 = CARTESIAN_POINT('Origin',(28.375,-5.10702591327572E-15,42.8)) ;
#47929 = CARTESIAN_POINT('',(28.375,-5.09552105347153E-15,42.65)) ;
#47930 = CARTESIAN_POINT('Origin',(28.375,-5.09552105347153E-15,42.8)) ;
#47931 = CARTESIAN_POINT('',(28.2256289970792,0.0126778183972205,42.7947486756786)) ;
#47932 = CARTESIAN_POINT('Origin',(28.375,-5.10702591327572E-15,42.8)) ;
#47933 = CARTESIAN_POINT('Origin',(28.375,-5.10702591327572E-15,42.8)) ;
#47934 = CARTESIAN_POINT('Origin',(28.31875,-0.56568542494924,43.0343145750508)) ;
#47935 = CARTESIAN_POINT('',(28.1694861227066,-0.555190308577046,43.0238194586786)) ;
#47936 = CARTESIAN_POINT('',(28.4680138772934,-0.576180541321434,43.044809691423)) ;
#47937 = CARTESIAN_POINT('Origin',(28.31875,-0.56568542494924,43.0343145750508)) ;
#47938 = CARTESIAN_POINT('',(28.1693789970792,-0.560434100627805,43.0216367566535)) ;
#47939 = CARTESIAN_POINT('Origin',(28.31875,-0.56568542494924,43.0343145750508)) ;
#47940 = CARTESIAN_POINT('Origin',(28.31875,-0.56568542494924,43.0343145750508)) ;
#47941 = CARTESIAN_POINT('Origin',(28.2625,-0.8,43.6)) ;
#47942 = CARTESIAN_POINT('',(28.1132361227066,-0.800000000000001,43.5851576640878)) ;
#47943 = CARTESIAN_POINT('',(28.4117638772934,-0.799999999999999,43.6148423359122)) ;
#47944 = CARTESIAN_POINT('Origin',(28.2625,-0.8,43.6)) ;
#47945 = CARTESIAN_POINT('',(28.1131289970792,-0.805251324321435,43.5873221816028)) ;
#47946 = CARTESIAN_POINT('Origin',(28.2625,-0.8,43.6)) ;
#47947 = CARTESIAN_POINT('Origin',(28.2625,-0.8,43.6)) ;
#47948 = CARTESIAN_POINT('Origin',(28.20625,-0.565685424949239,44.1656854249492)) ;
#47949 = CARTESIAN_POINT('',(28.0569861227066,-0.576180541321436,44.155190308577)) ;
#47950 = CARTESIAN_POINT('',(28.3555138772934,-0.55519030857705,44.1761805413214)) ;
#47951 = CARTESIAN_POINT('Origin',(28.20625,-0.565685424949239,44.1656854249492)) ;
#47952 = CARTESIAN_POINT('',(28.0568789970792,-0.578363243346472,44.1604341006278)) ;
#47953 = CARTESIAN_POINT('Origin',(28.20625,-0.565685424949239,44.1656854249492)) ;
#47954 = CARTESIAN_POINT('Origin',(28.20625,-0.565685424949239,44.1656854249492)) ;
#47955 = CARTESIAN_POINT('Origin',(28.15,7.83972025258014E-15,44.4)) ;
#47956 = CARTESIAN_POINT('',(28.0007361227066,-0.0148423359122333,44.4)) ;
#47957 = CARTESIAN_POINT('',(28.2992638772934,0.014842335912249,44.4)) ;
#47958 = CARTESIAN_POINT('Origin',(28.15,7.93809462606987E-15,44.4)) ;
#47959 = CARTESIAN_POINT('',(28.0041439534833,7.82185803852985E-15,44.4350144783558)) ;
#47960 = CARTESIAN_POINT('Origin',(28.15,7.88258347483861E-15,44.4)) ;
#47961 = CARTESIAN_POINT('',(28.15,7.83972025258014E-15,44.55)) ;
#47962 = CARTESIAN_POINT('Origin',(28.15,7.83972025258014E-15,44.4)) ;
#47963 = CARTESIAN_POINT('',(28.0006289970792,-0.0126778183972181,44.4052513243214)) ;
#47964 = CARTESIAN_POINT('Origin',(28.15,7.88258347483861E-15,44.4)) ;
#47965 = CARTESIAN_POINT('Origin',(28.15,7.88258347483861E-15,44.4)) ;
#47966 = CARTESIAN_POINT('Origin',(28.09375,0.565685424949242,44.1656854249492)) ;
#47967 = CARTESIAN_POINT('',(27.9444861227066,0.555190308577047,44.1761805413214)) ;
#47968 = CARTESIAN_POINT('',(28.2430138772934,0.576180541321437,44.155190308577)) ;
#47969 = CARTESIAN_POINT('Origin',(28.09375,0.565685424949242,44.1656854249492)) ;
#47970 = CARTESIAN_POINT('',(27.9443789970792,0.560434100627808,44.1783632433465)) ;
#47971 = CARTESIAN_POINT('Origin',(28.09375,0.565685424949242,44.1656854249492)) ;
#47972 = CARTESIAN_POINT('Origin',(28.09375,0.565685424949242,44.1656854249492)) ;
#47973 = CARTESIAN_POINT('Origin',(28.0375,0.8,43.6)) ;
#47974 = CARTESIAN_POINT('',(27.8882361227066,0.799999999999999,43.6148423359122)) ;
#47975 = CARTESIAN_POINT('',(28.1867638772934,0.799999999999998,43.5851576640877)) ;
#47976 = CARTESIAN_POINT('Origin',(28.0375,0.8,43.6)) ;
#47977 = CARTESIAN_POINT('',(27.8881289970792,0.805251324321436,43.6126778183972)) ;
#47978 = CARTESIAN_POINT('Origin',(28.0375,0.8,43.6)) ;
#47979 = CARTESIAN_POINT('Origin',(28.0375,0.8,43.6)) ;
#47980 = CARTESIAN_POINT('Origin',(27.98125,0.565685424949237,43.0343145750508)) ;
#47981 = CARTESIAN_POINT('',(27.8319861227066,0.576180541321441,43.0448096914229)) ;
#47982 = CARTESIAN_POINT('',(28.1305138772934,0.555190308577051,43.0238194586786)) ;
#47983 = CARTESIAN_POINT('Origin',(27.98125,0.565685424949237,43.0343145750508)) ;
#47984 = CARTESIAN_POINT('',(27.8318789970792,0.578363243346469,43.0395658993722)) ;
#47985 = CARTESIAN_POINT('Origin',(27.98125,0.565685424949237,43.0343145750508)) ;
#47986 = CARTESIAN_POINT('Origin',(27.98125,0.565685424949237,43.0343145750508)) ;
#47987 = CARTESIAN_POINT('Origin',(27.925,7.84764320472847E-16,42.8)) ;
#47988 = CARTESIAN_POINT('',(27.7757361227066,0.0148423359122439,42.8)) ;
#47989 = CARTESIAN_POINT('',(28.0742638772934,-0.0148423359122386,42.8)) ;
#47990 = CARTESIAN_POINT('Origin',(27.925,7.7715611723761E-16,42.8)) ;
#47991 = CARTESIAN_POINT('',(27.7791439534833,7.66902106422555E-16,42.7649855216442)) ;
#47992 = CARTESIAN_POINT('Origin',(27.925,8.32667268468867E-16,42.8)) ;
#47993 = CARTESIAN_POINT('',(27.925,7.84764320472847E-16,42.65)) ;
#47994 = CARTESIAN_POINT('Origin',(27.925,7.84764320472847E-16,42.8)) ;
#47995 = CARTESIAN_POINT('',(27.7756289970792,0.0126778183972334,42.7947486756786)) ;
#47996 = CARTESIAN_POINT('Origin',(27.925,8.32667268468867E-16,42.8)) ;
#47997 = CARTESIAN_POINT('Origin',(27.925,8.32667268468867E-16,42.8)) ;
#47998 = CARTESIAN_POINT('Origin',(27.86875,-0.565685424949236,43.0343145750508)) ;
#47999 = CARTESIAN_POINT('',(27.7194861227066,-0.555190308577041,43.0238194586786)) ;
#48000 = CARTESIAN_POINT('',(28.0180138772934,-0.576180541321428,43.044809691423)) ;
#48001 = CARTESIAN_POINT('Origin',(27.86875,-0.565685424949236,43.0343145750508)) ;
#48002 = CARTESIAN_POINT('',(27.7193789970792,-0.560434100627802,43.0216367566535)) ;
#48003 = CARTESIAN_POINT('Origin',(27.86875,-0.565685424949236,43.0343145750508)) ;
#48004 = CARTESIAN_POINT('Origin',(27.86875,-0.565685424949236,43.0343145750508)) ;
#48005 = CARTESIAN_POINT('Origin',(27.8125,-0.8,43.6)) ;
#48006 = CARTESIAN_POINT('',(27.6632361227066,-0.8,43.5851576640878)) ;
#48007 = CARTESIAN_POINT('',(27.9617638772934,-0.8,43.6148423359123)) ;
#48008 = CARTESIAN_POINT('Origin',(27.8125,-0.8,43.6)) ;
#48009 = CARTESIAN_POINT('',(27.6631289970792,-0.805251324321434,43.5873221816028)) ;
#48010 = CARTESIAN_POINT('Origin',(27.8125,-0.8,43.6)) ;
#48011 = CARTESIAN_POINT('Origin',(27.8125,-0.8,43.6)) ;
#48012 = CARTESIAN_POINT('Origin',(27.75625,-0.565685424949235,44.1656854249492)) ;
#48013 = CARTESIAN_POINT('',(27.6069861227066,-0.576180541321429,44.1551903085771)) ;
#48014 = CARTESIAN_POINT('',(27.9055138772934,-0.555190308577041,44.1761805413214)) ;
#48015 = CARTESIAN_POINT('Origin',(27.75625,-0.565685424949235,44.1656854249492)) ;
#48016 = CARTESIAN_POINT('',(27.6068789970792,-0.578363243346462,44.1604341006278)) ;
#48017 = CARTESIAN_POINT('Origin',(27.75625,-0.565685424949235,44.1656854249492)) ;
#48018 = CARTESIAN_POINT('Origin',(27.75625,-0.565685424949235,44.1656854249492)) ;
#48019 = CARTESIAN_POINT('Origin',(27.7,1.95943487863577E-15,44.4)) ;
#48020 = CARTESIAN_POINT('',(27.5507361227066,-0.0148423359122409,44.4)) ;
#48021 = CARTESIAN_POINT('',(27.8492638772934,0.0148423359122416,44.4)) ;
#48022 = CARTESIAN_POINT('Origin',(27.7,2.05391259555654E-15,44.4)) ;
#48023 = CARTESIAN_POINT('',(27.5541439534833,1.94157266458547E-15,44.4350144783558)) ;
#48024 = CARTESIAN_POINT('Origin',(27.7,1.94289029309402E-15,44.4)) ;
#48025 = CARTESIAN_POINT('',(27.7,1.95943487863577E-15,44.55)) ;
#48026 = CARTESIAN_POINT('Origin',(27.7,1.95943487863577E-15,44.4)) ;
#48027 = CARTESIAN_POINT('',(27.5506289970792,-0.0126778183972306,44.4052513243214)) ;
#48028 = CARTESIAN_POINT('Origin',(27.7,1.94289029309402E-15,44.4)) ;
#48029 = CARTESIAN_POINT('Origin',(27.7,1.94289029309402E-15,44.4)) ;
#48030 = CARTESIAN_POINT('Origin',(27.64375,0.565685424949238,44.1656854249492)) ;
#48031 = CARTESIAN_POINT('',(27.4944861227066,0.555190308577042,44.1761805413214)) ;
#48032 = CARTESIAN_POINT('',(27.7930138772934,0.576180541321432,44.155190308577)) ;
#48033 = CARTESIAN_POINT('Origin',(27.64375,0.565685424949238,44.1656854249492)) ;
#48034 = CARTESIAN_POINT('',(27.4943789970792,0.560434100627803,44.1783632433465)) ;
#48035 = CARTESIAN_POINT('Origin',(27.64375,0.565685424949238,44.1656854249492)) ;
#48036 = CARTESIAN_POINT('Origin',(27.64375,0.565685424949238,44.1656854249492)) ;
#48037 = CARTESIAN_POINT('Origin',(27.5875,0.8,43.6)) ;
#48038 = CARTESIAN_POINT('',(27.4382361227066,0.8,43.6148423359122)) ;
#48039 = CARTESIAN_POINT('',(27.7367638772934,0.799999999999996,43.5851576640877)) ;
#48040 = CARTESIAN_POINT('Origin',(27.5875,0.8,43.6)) ;
#48041 = CARTESIAN_POINT('',(27.4381289970792,0.805251324321436,43.6126778183972)) ;
#48042 = CARTESIAN_POINT('Origin',(27.5875,0.8,43.6)) ;
#48043 = CARTESIAN_POINT('Origin',(27.5875,0.8,43.6)) ;
#48044 = CARTESIAN_POINT('Origin',(27.53125,0.565685424949237,43.0343145750508)) ;
#48045 = CARTESIAN_POINT('',(27.3819861227066,0.576180541321439,43.0448096914229)) ;
#48046 = CARTESIAN_POINT('',(27.6805138772934,0.555190308577052,43.0238194586786)) ;
#48047 = CARTESIAN_POINT('Origin',(27.53125,0.565685424949237,43.0343145750508)) ;
#48048 = CARTESIAN_POINT('',(27.3818789970792,0.578363243346468,43.0395658993722)) ;
#48049 = CARTESIAN_POINT('Origin',(27.53125,0.565685424949237,43.0343145750508)) ;
#48050 = CARTESIAN_POINT('Origin',(27.53125,0.565685424949237,43.0343145750508)) ;
#48051 = CARTESIAN_POINT('Origin',(27.475,-4.70363407774438E-15,42.8)) ;
#48052 = CARTESIAN_POINT('',(27.3257361227066,0.0148423359122361,42.8)) ;
#48053 = CARTESIAN_POINT('',(27.6242638772934,-0.0148423359122454,42.8)) ;
#48054 = CARTESIAN_POINT('Origin',(27.475,-4.66293670342566E-15,42.8)) ;
#48055 = CARTESIAN_POINT('',(27.3291439534833,-4.72149629179467E-15,42.7649855216442)) ;
#48056 = CARTESIAN_POINT('Origin',(27.475,-4.6074255521944E-15,42.8)) ;
#48057 = CARTESIAN_POINT('',(27.475,-4.70363407774438E-15,42.65)) ;
#48058 = CARTESIAN_POINT('Origin',(27.475,-4.70363407774438E-15,42.8)) ;
#48059 = CARTESIAN_POINT('',(27.3256289970792,0.0126778183972205,42.7947486756786)) ;
#48060 = CARTESIAN_POINT('Origin',(27.475,-4.6074255521944E-15,42.8)) ;
#48061 = CARTESIAN_POINT('Origin',(27.475,-4.6074255521944E-15,42.8)) ;
#48062 = CARTESIAN_POINT('Origin',(27.41875,-0.56568542494924,43.0343145750508)) ;
#48063 = CARTESIAN_POINT('',(27.2694861227066,-0.555190308577046,43.0238194586786)) ;
#48064 = CARTESIAN_POINT('',(27.5680138772934,-0.576180541321434,43.044809691423)) ;
#48065 = CARTESIAN_POINT('Origin',(27.41875,-0.56568542494924,43.0343145750508)) ;
#48066 = CARTESIAN_POINT('',(27.2693789970792,-0.560434100627804,43.0216367566535)) ;
#48067 = CARTESIAN_POINT('Origin',(27.41875,-0.56568542494924,43.0343145750508)) ;
#48068 = CARTESIAN_POINT('Origin',(27.41875,-0.56568542494924,43.0343145750508)) ;
#48069 = CARTESIAN_POINT('Origin',(27.3625,-0.8,43.6)) ;
#48070 = CARTESIAN_POINT('',(27.2132361227066,-0.799999999999997,43.5851576640878)) ;
#48071 = CARTESIAN_POINT('',(27.5117638772934,-0.799999999999999,43.6148423359122)) ;
#48072 = CARTESIAN_POINT('Origin',(27.3625,-0.8,43.6)) ;
#48073 = CARTESIAN_POINT('',(27.2131289970792,-0.805251324321435,43.5873221816028)) ;
#48074 = CARTESIAN_POINT('Origin',(27.3625,-0.8,43.6)) ;
#48075 = CARTESIAN_POINT('Origin',(27.3625,-0.8,43.6)) ;
#48076 = CARTESIAN_POINT('Origin',(27.30625,-0.565685424949235,44.1656854249492)) ;
#48077 = CARTESIAN_POINT('',(27.1569861227066,-0.576180541321439,44.1551903085771)) ;
#48078 = CARTESIAN_POINT('',(27.4555138772934,-0.555190308577049,44.1761805413214)) ;
#48079 = CARTESIAN_POINT('Origin',(27.30625,-0.565685424949235,44.1656854249493)) ;
#48080 = CARTESIAN_POINT('',(27.1568789970792,-0.578363243346466,44.1604341006278)) ;
#48081 = CARTESIAN_POINT('Origin',(27.30625,-0.565685424949235,44.1656854249492)) ;
#48082 = CARTESIAN_POINT('Origin',(27.30625,-0.565685424949235,44.1656854249492)) ;
#48083 = CARTESIAN_POINT('Origin',(27.25,1.76349139077219E-15,44.4)) ;
#48084 = CARTESIAN_POINT('',(27.1007361227066,-0.0148423359122413,44.4)) ;
#48085 = CARTESIAN_POINT('',(27.3992638772934,0.0148423359122413,44.4)) ;
#48086 = CARTESIAN_POINT('Origin',(27.25,1.77635683940025E-15,44.4)) ;
#48087 = CARTESIAN_POINT('',(27.1041439534833,1.7456291767219E-15,44.4350144783558)) ;
#48088 = CARTESIAN_POINT('Origin',(27.25,1.77635683940025E-15,44.4)) ;
#48089 = CARTESIAN_POINT('',(27.25,1.76349139077219E-15,44.55)) ;
#48090 = CARTESIAN_POINT('Origin',(27.25,1.76349139077219E-15,44.4)) ;
#48091 = CARTESIAN_POINT('',(27.1006289970792,-0.0126778183972294,44.4052513243214)) ;
#48092 = CARTESIAN_POINT('Origin',(27.25,1.77635683940025E-15,44.4)) ;
#48093 = CARTESIAN_POINT('Origin',(27.25,1.77635683940025E-15,44.4)) ;
#48094 = CARTESIAN_POINT('Origin',(27.19375,0.565685424949238,44.1656854249492)) ;
#48095 = CARTESIAN_POINT('',(27.0444861227066,0.555190308577043,44.1761805413214)) ;
#48096 = CARTESIAN_POINT('',(27.3430138772934,0.576180541321431,44.155190308577)) ;
#48097 = CARTESIAN_POINT('Origin',(27.19375,0.565685424949238,44.1656854249492)) ;
#48098 = CARTESIAN_POINT('',(27.0443789970792,0.560434100627803,44.1783632433465)) ;
#48099 = CARTESIAN_POINT('Origin',(27.19375,0.565685424949238,44.1656854249492)) ;
#48100 = CARTESIAN_POINT('Origin',(27.19375,0.565685424949238,44.1656854249492)) ;
#48101 = CARTESIAN_POINT('Origin',(27.1375,0.8,43.6)) ;
#48102 = CARTESIAN_POINT('',(26.9882361227066,0.8,43.6148423359122)) ;
#48103 = CARTESIAN_POINT('',(27.2867638772934,0.799999999999996,43.5851576640877)) ;
#48104 = CARTESIAN_POINT('Origin',(27.1375,0.8,43.6)) ;
#48105 = CARTESIAN_POINT('',(26.9881289970792,0.805251324321436,43.6126778183972)) ;
#48106 = CARTESIAN_POINT('Origin',(27.1375,0.8,43.6)) ;
#48107 = CARTESIAN_POINT('Origin',(27.1375,0.8,43.6)) ;
#48108 = CARTESIAN_POINT('Origin',(27.08125,0.565685424949237,43.0343145750508)) ;
#48109 = CARTESIAN_POINT('',(26.9319861227066,0.57618054132144,43.044809691423)) ;
#48110 = CARTESIAN_POINT('',(27.2305138772934,0.555190308577053,43.0238194586786)) ;
#48111 = CARTESIAN_POINT('Origin',(27.08125,0.565685424949237,43.0343145750508)) ;
#48112 = CARTESIAN_POINT('',(26.9318789970792,0.578363243346467,43.0395658993722)) ;
#48113 = CARTESIAN_POINT('Origin',(27.08125,0.565685424949237,43.0343145750508)) ;
#48114 = CARTESIAN_POINT('Origin',(27.08125,0.565685424949237,43.0343145750508)) ;
#48115 = CARTESIAN_POINT('Origin',(27.025,1.1766512962E-15,42.8)) ;
#48116 = CARTESIAN_POINT('',(26.8757361227066,0.0148423359122424,42.8)) ;
#48117 = CARTESIAN_POINT('',(27.1742638772934,-0.01484233591224,42.8)) ;
#48118 = CARTESIAN_POINT('Origin',(27.025,1.16573417585641E-15,42.8)) ;
#48119 = CARTESIAN_POINT('',(26.8791439534833,1.15878908214971E-15,42.7649855216442)) ;
#48120 = CARTESIAN_POINT('Origin',(27.025,1.27675647831893E-15,42.8)) ;
#48121 = CARTESIAN_POINT('',(27.025,1.1766512962E-15,42.65)) ;
#48122 = CARTESIAN_POINT('Origin',(27.025,1.1766512962E-15,42.8)) ;
#48123 = CARTESIAN_POINT('',(26.8756289970792,0.012677818397228,42.7947486756786)) ;
#48124 = CARTESIAN_POINT('Origin',(27.025,1.27675647831893E-15,42.8)) ;
#48125 = CARTESIAN_POINT('Origin',(27.025,1.27675647831893E-15,42.8)) ;
#48126 = CARTESIAN_POINT('Origin',(26.96875,-0.56568542494924,43.0343145750508)) ;
#48127 = CARTESIAN_POINT('',(26.8194861227066,-0.555190308577045,43.0238194586786)) ;
#48128 = CARTESIAN_POINT('',(27.1180138772934,-0.576180541321435,43.044809691423)) ;
#48129 = CARTESIAN_POINT('Origin',(26.96875,-0.56568542494924,43.0343145750508)) ;
#48130 = CARTESIAN_POINT('',(26.8193789970792,-0.560434100627806,43.0216367566535)) ;
#48131 = CARTESIAN_POINT('Origin',(26.96875,-0.56568542494924,43.0343145750508)) ;
#48132 = CARTESIAN_POINT('Origin',(26.96875,-0.56568542494924,43.0343145750508)) ;
#48133 = CARTESIAN_POINT('Origin',(26.9125,-0.8,43.6)) ;
#48134 = CARTESIAN_POINT('',(26.7632361227066,-0.799999999999999,43.5851576640878)) ;
#48135 = CARTESIAN_POINT('',(27.0617638772934,-0.799999999999999,43.6148423359123)) ;
#48136 = CARTESIAN_POINT('Origin',(26.9125,-0.8,43.6)) ;
#48137 = CARTESIAN_POINT('',(26.7631289970792,-0.805251324321435,43.5873221816028)) ;
#48138 = CARTESIAN_POINT('Origin',(26.9125,-0.8,43.6)) ;
#48139 = CARTESIAN_POINT('Origin',(26.9125,-0.8,43.6)) ;
#48140 = CARTESIAN_POINT('Origin',(26.85625,-0.565685424949235,44.1656854249492)) ;
#48141 = CARTESIAN_POINT('',(26.7069861227066,-0.57618054132143,44.1551903085771)) ;
#48142 = CARTESIAN_POINT('',(27.0055138772934,-0.55519030857704,44.1761805413214)) ;
#48143 = CARTESIAN_POINT('Origin',(26.85625,-0.565685424949235,44.1656854249492)) ;
#48144 = CARTESIAN_POINT('',(26.7068789970792,-0.578363243346464,44.1604341006278)) ;
#48145 = CARTESIAN_POINT('Origin',(26.85625,-0.565685424949235,44.1656854249492)) ;
#48146 = CARTESIAN_POINT('Origin',(26.85625,-0.565685424949235,44.1656854249492)) ;
#48147 = CARTESIAN_POINT('Origin',(26.8,1.56754790290861E-15,44.4)) ;
#48148 = CARTESIAN_POINT('',(26.6507361227066,-0.0148423359122415,44.4)) ;
#48149 = CARTESIAN_POINT('',(26.9492638772934,0.014842335912241,44.4)) ;
#48150 = CARTESIAN_POINT('Origin',(26.8,1.55431223447522E-15,44.4)) ;
#48151 = CARTESIAN_POINT('',(26.6541439534833,1.54968568885832E-15,44.4350144783558)) ;
#48152 = CARTESIAN_POINT('Origin',(26.8,1.55431223447522E-15,44.4)) ;
#48153 = CARTESIAN_POINT('',(26.8,1.56754790290861E-15,44.55)) ;
#48154 = CARTESIAN_POINT('Origin',(26.8,1.56754790290861E-15,44.4)) ;
#48155 = CARTESIAN_POINT('',(26.6506289970792,-0.0126778183972318,44.4052513243214)) ;
#48156 = CARTESIAN_POINT('Origin',(26.8,1.55431223447522E-15,44.4)) ;
#48157 = CARTESIAN_POINT('Origin',(26.8,1.55431223447522E-15,44.4)) ;
#48158 = CARTESIAN_POINT('Origin',(26.74375,0.565685424949238,44.1656854249492)) ;
#48159 = CARTESIAN_POINT('',(26.5944861227066,0.555190308577043,44.1761805413214)) ;
#48160 = CARTESIAN_POINT('',(26.8930138772934,0.57618054132143,44.155190308577)) ;
#48161 = CARTESIAN_POINT('Origin',(26.74375,0.565685424949238,44.1656854249492)) ;
#48162 = CARTESIAN_POINT('',(26.5943789970792,0.560434100627802,44.1783632433465)) ;
#48163 = CARTESIAN_POINT('Origin',(26.74375,0.565685424949238,44.1656854249492)) ;
#48164 = CARTESIAN_POINT('Origin',(26.74375,0.565685424949238,44.1656854249492)) ;
#48165 = CARTESIAN_POINT('Origin',(26.6875,0.8,43.6)) ;
#48166 = CARTESIAN_POINT('',(26.5382361227066,0.800000000000001,43.6148423359122)) ;
#48167 = CARTESIAN_POINT('',(26.8367638772934,0.800000000000002,43.5851576640877)) ;
#48168 = CARTESIAN_POINT('Origin',(26.6875,0.8,43.6)) ;
#48169 = CARTESIAN_POINT('',(26.5381289970792,0.805251324321436,43.6126778183972)) ;
#48170 = CARTESIAN_POINT('Origin',(26.6875,0.8,43.6)) ;
#48171 = CARTESIAN_POINT('Origin',(26.6875,0.8,43.6)) ;
#48172 = CARTESIAN_POINT('Origin',(26.63125,0.565685424949237,43.0343145750508)) ;
#48173 = CARTESIAN_POINT('',(26.4819861227066,0.57618054132144,43.0448096914229)) ;
#48174 = CARTESIAN_POINT('',(26.7805138772934,0.555190308577052,43.0238194586786)) ;
#48175 = CARTESIAN_POINT('Origin',(26.63125,0.565685424949237,43.0343145750508)) ;
#48176 = CARTESIAN_POINT('',(26.4818789970792,0.578363243346473,43.0395658993722)) ;
#48177 = CARTESIAN_POINT('Origin',(26.63125,0.565685424949238,43.0343145750508)) ;
#48178 = CARTESIAN_POINT('Origin',(26.63125,0.565685424949238,43.0343145750508)) ;
#48179 = CARTESIAN_POINT('Origin',(26.575,-4.31174710201723E-15,42.8)) ;
#48180 = CARTESIAN_POINT('',(26.4257361227066,0.0148423359122368,42.8)) ;
#48181 = CARTESIAN_POINT('',(26.7242638772934,-0.0148423359122456,42.8)) ;
#48182 = CARTESIAN_POINT('Origin',(26.575,-4.38538094726937E-15,42.8)) ;
#48183 = CARTESIAN_POINT('',(26.4291439534833,-4.32960931606752E-15,42.7649855216442)) ;
#48184 = CARTESIAN_POINT('Origin',(26.575,-4.32986979603811E-15,42.8)) ;
#48185 = CARTESIAN_POINT('',(26.575,-4.31174710201723E-15,42.65)) ;
#48186 = CARTESIAN_POINT('Origin',(26.575,-4.31174710201723E-15,42.8)) ;
#48187 = CARTESIAN_POINT('',(26.4256289970792,0.0126778183972232,42.7947486756786)) ;
#48188 = CARTESIAN_POINT('Origin',(26.575,-4.32986979603811E-15,42.8)) ;
#48189 = CARTESIAN_POINT('Origin',(26.575,-4.32986979603811E-15,42.8)) ;
#48190 = CARTESIAN_POINT('Origin',(26.51875,-0.56568542494924,43.0343145750508)) ;
#48191 = CARTESIAN_POINT('',(26.3694861227066,-0.555190308577044,43.0238194586786)) ;
#48192 = CARTESIAN_POINT('',(26.6680138772934,-0.576180541321435,43.044809691423)) ;
#48193 = CARTESIAN_POINT('Origin',(26.51875,-0.56568542494924,43.0343145750508)) ;
#48194 = CARTESIAN_POINT('',(26.3693789970792,-0.560434100627805,43.0216367566535)) ;
#48195 = CARTESIAN_POINT('Origin',(26.51875,-0.56568542494924,43.0343145750508)) ;
#48196 = CARTESIAN_POINT('Origin',(26.51875,-0.56568542494924,43.0343145750508)) ;
#48197 = CARTESIAN_POINT('Origin',(26.4625,-0.8,43.6)) ;
#48198 = CARTESIAN_POINT('',(26.3132361227066,-0.8,43.5851576640878)) ;
#48199 = CARTESIAN_POINT('',(26.6117638772934,-0.799999999999997,43.6148423359123)) ;
#48200 = CARTESIAN_POINT('Origin',(26.4625,-0.8,43.6)) ;
#48201 = CARTESIAN_POINT('',(26.3131289970792,-0.805251324321436,43.5873221816028)) ;
#48202 = CARTESIAN_POINT('Origin',(26.4625,-0.8,43.6)) ;
#48203 = CARTESIAN_POINT('Origin',(26.4625,-0.8,43.6)) ;
#48204 = CARTESIAN_POINT('Origin',(26.40625,-0.565685424949235,44.1656854249492)) ;
#48205 = CARTESIAN_POINT('',(26.2569861227066,-0.576180541321437,44.1551903085771)) ;
#48206 = CARTESIAN_POINT('',(26.5555138772934,-0.55519030857705,44.1761805413215)) ;
#48207 = CARTESIAN_POINT('Origin',(26.40625,-0.565685424949235,44.1656854249493)) ;
#48208 = CARTESIAN_POINT('',(26.2568789970792,-0.578363243346465,44.1604341006278)) ;
#48209 = CARTESIAN_POINT('Origin',(26.40625,-0.565685424949235,44.1656854249492)) ;
#48210 = CARTESIAN_POINT('Origin',(26.40625,-0.565685424949235,44.1656854249492)) ;
#48211 = CARTESIAN_POINT('Origin',(26.35,1.37160441504504E-15,44.4)) ;
#48212 = CARTESIAN_POINT('',(26.2007361227066,-0.0148423359122412,44.4)) ;
#48213 = CARTESIAN_POINT('',(26.4992638772934,0.0148423359122403,44.4)) ;
#48214 = CARTESIAN_POINT('Origin',(26.35,1.33226762955019E-15,44.4)) ;
#48215 = CARTESIAN_POINT('',(26.2041439534833,1.35374220099474E-15,44.4350144783558)) ;
#48216 = CARTESIAN_POINT('Origin',(26.35,1.33226762955019E-15,44.4)) ;
#48217 = CARTESIAN_POINT('',(26.35,1.37160441504504E-15,44.55)) ;
#48218 = CARTESIAN_POINT('Origin',(26.35,1.37160441504504E-15,44.4)) ;
#48219 = CARTESIAN_POINT('',(26.2006289970792,-0.012677818397228,44.4052513243214)) ;
#48220 = CARTESIAN_POINT('Origin',(26.35,1.33226762955019E-15,44.4)) ;
#48221 = CARTESIAN_POINT('Origin',(26.35,1.33226762955019E-15,44.4)) ;
#48222 = CARTESIAN_POINT('Origin',(26.29375,0.565685424949237,44.1656854249492)) ;
#48223 = CARTESIAN_POINT('',(26.1444861227066,0.555190308577042,44.1761805413214)) ;
#48224 = CARTESIAN_POINT('',(26.4430138772934,0.576180541321429,44.155190308577)) ;
#48225 = CARTESIAN_POINT('Origin',(26.29375,0.565685424949237,44.1656854249492)) ;
#48226 = CARTESIAN_POINT('',(26.1443789970792,0.560434100627804,44.1783632433465)) ;
#48227 = CARTESIAN_POINT('Origin',(26.29375,0.565685424949238,44.1656854249492)) ;
#48228 = CARTESIAN_POINT('Origin',(26.29375,0.565685424949238,44.1656854249492)) ;
#48229 = CARTESIAN_POINT('Origin',(26.2375,0.8,43.6)) ;
#48230 = CARTESIAN_POINT('',(26.0882361227066,0.799999999999999,43.6148423359122)) ;
#48231 = CARTESIAN_POINT('',(26.3867638772934,0.800000000000001,43.5851576640878)) ;
#48232 = CARTESIAN_POINT('Origin',(26.2375,0.8,43.6)) ;
#48233 = CARTESIAN_POINT('',(26.0881289970792,0.805251324321434,43.6126778183972)) ;
#48234 = CARTESIAN_POINT('Origin',(26.2375,0.8,43.6)) ;
#48235 = CARTESIAN_POINT('Origin',(26.2375,0.8,43.6)) ;
#48236 = CARTESIAN_POINT('Origin',(26.18125,0.565685424949238,43.0343145750508)) ;
#48237 = CARTESIAN_POINT('',(26.0319861227066,0.576180541321433,43.044809691423)) ;
#48238 = CARTESIAN_POINT('',(26.3305138772934,0.555190308577043,43.0238194586786)) ;
#48239 = CARTESIAN_POINT('Origin',(26.18125,0.565685424949238,43.0343145750508)) ;
#48240 = CARTESIAN_POINT('',(26.0318789970792,0.578363243346464,43.0395658993722)) ;
#48241 = CARTESIAN_POINT('Origin',(26.18125,0.565685424949238,43.0343145750508)) ;
#48242 = CARTESIAN_POINT('Origin',(26.18125,0.565685424949238,43.0343145750508)) ;
#48243 = CARTESIAN_POINT('Origin',(26.125,1.56853827192715E-15,42.8)) ;
#48244 = CARTESIAN_POINT('',(25.9757361227066,0.0148423359122427,42.8)) ;
#48245 = CARTESIAN_POINT('',(26.2742638772934,-0.0148423359122397,42.8)) ;
#48246 = CARTESIAN_POINT('Origin',(26.125,1.55431223447522E-15,42.8)) ;
#48247 = CARTESIAN_POINT('',(25.9791439534833,1.55067605787686E-15,42.7649855216442)) ;
#48248 = CARTESIAN_POINT('Origin',(26.125,1.60982338570648E-15,42.8)) ;
#48249 = CARTESIAN_POINT('',(26.125,1.56853827192715E-15,42.65)) ;
#48250 = CARTESIAN_POINT('Origin',(26.125,1.56853827192715E-15,42.8)) ;
#48251 = CARTESIAN_POINT('',(25.9756289970792,0.0126778183972272,42.7947486756786)) ;
#48252 = CARTESIAN_POINT('Origin',(26.125,1.60982338570648E-15,42.8)) ;
#48253 = CARTESIAN_POINT('Origin',(26.125,1.60982338570648E-15,42.8)) ;
#48254 = CARTESIAN_POINT('Origin',(26.06875,-0.565685424949239,43.0343145750508)) ;
#48255 = CARTESIAN_POINT('',(25.9194861227066,-0.555190308577046,43.0238194586786)) ;
#48256 = CARTESIAN_POINT('',(26.2180138772934,-0.576180541321434,43.044809691423)) ;
#48257 = CARTESIAN_POINT('Origin',(26.06875,-0.56568542494924,43.0343145750508)) ;
#48258 = CARTESIAN_POINT('',(25.9193789970792,-0.560434100627805,43.0216367566535)) ;
#48259 = CARTESIAN_POINT('Origin',(26.06875,-0.565685424949239,43.0343145750508)) ;
#48260 = CARTESIAN_POINT('Origin',(26.06875,-0.565685424949239,43.0343145750508)) ;
#48261 = CARTESIAN_POINT('Origin',(26.0125,-0.8,43.6)) ;
#48262 = CARTESIAN_POINT('',(25.8632361227066,-0.799999999999999,43.5851576640878)) ;
#48263 = CARTESIAN_POINT('',(26.1617638772934,-0.799999999999997,43.6148423359122)) ;
#48264 = CARTESIAN_POINT('Origin',(26.0125,-0.8,43.6)) ;
#48265 = CARTESIAN_POINT('',(25.8631289970792,-0.805251324321436,43.5873221816028)) ;
#48266 = CARTESIAN_POINT('Origin',(26.0125,-0.8,43.6)) ;
#48267 = CARTESIAN_POINT('Origin',(26.0125,-0.8,43.6)) ;
#48268 = CARTESIAN_POINT('Origin',(25.95625,-0.565685424949236,44.1656854249492)) ;
#48269 = CARTESIAN_POINT('',(25.8069861227066,-0.576180541321438,44.1551903085771)) ;
#48270 = CARTESIAN_POINT('',(26.1055138772934,-0.555190308577051,44.1761805413215)) ;
#48271 = CARTESIAN_POINT('Origin',(25.95625,-0.565685424949236,44.1656854249493)) ;
#48272 = CARTESIAN_POINT('',(25.8068789970792,-0.578363243346467,44.1604341006278)) ;
#48273 = CARTESIAN_POINT('Origin',(25.95625,-0.565685424949236,44.1656854249492)) ;
#48274 = CARTESIAN_POINT('Origin',(25.95625,-0.565685424949236,44.1656854249492)) ;
#48275 = CARTESIAN_POINT('Origin',(25.9,1.17566092718146E-15,44.4)) ;
#48276 = CARTESIAN_POINT('',(25.7507361227066,-0.0148423359122419,44.4)) ;
#48277 = CARTESIAN_POINT('',(26.0492638772934,0.0148423359122407,44.4)) ;
#48278 = CARTESIAN_POINT('Origin',(25.9,1.22124532708767E-15,44.4)) ;
#48279 = CARTESIAN_POINT('',(25.7541439534833,1.15779871313117E-15,44.4350144783558)) ;
#48280 = CARTESIAN_POINT('Origin',(25.9,1.22124532708767E-15,44.4)) ;
#48281 = CARTESIAN_POINT('',(25.9,1.17566092718146E-15,44.55)) ;
#48282 = CARTESIAN_POINT('Origin',(25.9,1.17566092718146E-15,44.4)) ;
#48283 = CARTESIAN_POINT('',(25.7506289970792,-0.0126778183972336,44.4052513243214)) ;
#48284 = CARTESIAN_POINT('Origin',(25.9,1.22124532708767E-15,44.4)) ;
#48285 = CARTESIAN_POINT('Origin',(25.9,1.22124532708767E-15,44.4)) ;
#48286 = CARTESIAN_POINT('Origin',(25.84375,0.565685424949237,44.1656854249492)) ;
#48287 = CARTESIAN_POINT('',(25.6944861227066,0.555190308577042,44.1761805413214)) ;
#48288 = CARTESIAN_POINT('',(25.9930138772934,0.576180541321432,44.155190308577)) ;
#48289 = CARTESIAN_POINT('Origin',(25.84375,0.565685424949237,44.1656854249492)) ;
#48290 = CARTESIAN_POINT('',(25.6943789970792,0.560434100627803,44.1783632433465)) ;
#48291 = CARTESIAN_POINT('Origin',(25.84375,0.565685424949237,44.1656854249492)) ;
#48292 = CARTESIAN_POINT('Origin',(25.84375,0.565685424949237,44.1656854249492)) ;
#48293 = CARTESIAN_POINT('Origin',(25.7875,0.8,43.6)) ;
#48294 = CARTESIAN_POINT('',(25.6382361227066,0.8,43.6148423359122)) ;
#48295 = CARTESIAN_POINT('',(25.9367638772934,0.8,43.5851576640878)) ;
#48296 = CARTESIAN_POINT('Origin',(25.7875,0.8,43.6)) ;
#48297 = CARTESIAN_POINT('',(25.6381289970792,0.805251324321434,43.6126778183972)) ;
#48298 = CARTESIAN_POINT('Origin',(25.7875,0.8,43.6)) ;
#48299 = CARTESIAN_POINT('Origin',(25.7875,0.8,43.6)) ;
#48300 = CARTESIAN_POINT('Origin',(25.73125,0.565685424949238,43.0343145750508)) ;
#48301 = CARTESIAN_POINT('',(25.5819861227066,0.576180541321433,43.044809691423)) ;
#48302 = CARTESIAN_POINT('',(25.8805138772934,0.555190308577043,43.0238194586786)) ;
#48303 = CARTESIAN_POINT('Origin',(25.73125,0.565685424949238,43.0343145750508)) ;
#48304 = CARTESIAN_POINT('',(25.5818789970792,0.578363243346464,43.0395658993722)) ;
#48305 = CARTESIAN_POINT('Origin',(25.73125,0.565685424949238,43.0343145750508)) ;
#48306 = CARTESIAN_POINT('Origin',(25.73125,0.565685424949238,43.0343145750508)) ;
#48307 = CARTESIAN_POINT('Origin',(25.675,-3.91986012629007E-15,42.8)) ;
#48308 = CARTESIAN_POINT('',(25.5257361227066,0.0148423359122374,42.8)) ;
#48309 = CARTESIAN_POINT('',(25.8242638772934,-0.014842335912245,42.8)) ;
#48310 = CARTESIAN_POINT('Origin',(25.675,-3.88578058618805E-15,42.8)) ;
#48311 = CARTESIAN_POINT('',(25.5291439534833,-3.93772234034036E-15,42.7649855216442)) ;
#48312 = CARTESIAN_POINT('Origin',(25.675,-3.83026943495679E-15,42.8)) ;
#48313 = CARTESIAN_POINT('',(25.675,-3.91986012629007E-15,42.65)) ;
#48314 = CARTESIAN_POINT('Origin',(25.675,-3.91986012629007E-15,42.8)) ;
#48315 = CARTESIAN_POINT('',(25.5256289970792,0.0126778183972214,42.7947486756786)) ;
#48316 = CARTESIAN_POINT('Origin',(25.675,-3.83026943495679E-15,42.8)) ;
#48317 = CARTESIAN_POINT('Origin',(25.675,-3.83026943495679E-15,42.8)) ;
#48318 = CARTESIAN_POINT('Origin',(25.61875,-0.565685424949239,43.0343145750508)) ;
#48319 = CARTESIAN_POINT('',(25.4694861227066,-0.555190308577046,43.0238194586786)) ;
#48320 = CARTESIAN_POINT('',(25.7680138772934,-0.576180541321433,43.044809691423)) ;
#48321 = CARTESIAN_POINT('Origin',(25.61875,-0.565685424949239,43.0343145750508)) ;
#48322 = CARTESIAN_POINT('',(25.4693789970792,-0.560434100627804,43.0216367566535)) ;
#48323 = CARTESIAN_POINT('Origin',(25.61875,-0.565685424949239,43.0343145750508)) ;
#48324 = CARTESIAN_POINT('Origin',(25.61875,-0.565685424949239,43.0343145750508)) ;
#48325 = CARTESIAN_POINT('Origin',(25.5625,-0.8,43.6)) ;
#48326 = CARTESIAN_POINT('',(25.4132361227066,-0.799999999999997,43.5851576640878)) ;
#48327 = CARTESIAN_POINT('',(25.7117638772934,-0.799999999999999,43.6148423359122)) ;
#48328 = CARTESIAN_POINT('Origin',(25.5625,-0.8,43.6)) ;
#48329 = CARTESIAN_POINT('',(25.4131289970792,-0.805251324321435,43.5873221816028)) ;
#48330 = CARTESIAN_POINT('Origin',(25.5625,-0.8,43.6)) ;
#48331 = CARTESIAN_POINT('Origin',(25.5625,-0.8,43.6)) ;
#48332 = CARTESIAN_POINT('Origin',(25.50625,-0.565685424949236,44.1656854249492)) ;
#48333 = CARTESIAN_POINT('',(25.3569861227066,-0.57618054132143,44.155190308577)) ;
#48334 = CARTESIAN_POINT('',(25.6555138772934,-0.555190308577042,44.1761805413214)) ;
#48335 = CARTESIAN_POINT('Origin',(25.50625,-0.565685424949236,44.1656854249492)) ;
#48336 = CARTESIAN_POINT('',(25.3568789970792,-0.578363243346464,44.1604341006278)) ;
#48337 = CARTESIAN_POINT('Origin',(25.50625,-0.565685424949236,44.1656854249492)) ;
#48338 = CARTESIAN_POINT('Origin',(25.50625,-0.565685424949236,44.1656854249492)) ;
#48339 = CARTESIAN_POINT('Origin',(25.45,9.79717439317883E-16,44.4)) ;
#48340 = CARTESIAN_POINT('',(25.3007361227066,-0.014842335912242,44.4)) ;
#48341 = CARTESIAN_POINT('',(25.5992638772934,0.0148423359122405,44.4)) ;
#48342 = CARTESIAN_POINT('Origin',(25.45,9.99200722162641E-16,44.4)) ;
#48343 = CARTESIAN_POINT('',(25.3041439534833,9.6185522526759E-16,44.4350144783558)) ;
#48344 = CARTESIAN_POINT('Origin',(25.45,9.43689570931383E-16,44.4)) ;
#48345 = CARTESIAN_POINT('',(25.45,9.79717439317883E-16,44.55)) ;
#48346 = CARTESIAN_POINT('Origin',(25.45,9.79717439317883E-16,44.4)) ;
#48347 = CARTESIAN_POINT('',(25.3006289970792,-0.0126778183972314,44.4052513243214)) ;
#48348 = CARTESIAN_POINT('Origin',(25.45,9.43689570931383E-16,44.4)) ;
#48349 = CARTESIAN_POINT('Origin',(25.45,9.43689570931383E-16,44.4)) ;
#48350 = CARTESIAN_POINT('Origin',(25.39375,0.565685424949239,44.1656854249492)) ;
#48351 = CARTESIAN_POINT('',(25.2444861227066,0.555190308577043,44.1761805413214)) ;
#48352 = CARTESIAN_POINT('',(25.5430138772934,0.576180541321433,44.155190308577)) ;
#48353 = CARTESIAN_POINT('Origin',(25.39375,0.565685424949239,44.1656854249492)) ;
#48354 = CARTESIAN_POINT('',(25.2443789970792,0.560434100627806,44.1783632433465)) ;
#48355 = CARTESIAN_POINT('Origin',(25.39375,0.565685424949239,44.1656854249492)) ;
#48356 = CARTESIAN_POINT('Origin',(25.39375,0.565685424949239,44.1656854249492)) ;
#48357 = CARTESIAN_POINT('Origin',(25.3375,0.8,43.6)) ;
#48358 = CARTESIAN_POINT('',(25.1882361227066,0.800000000000002,43.6148423359122)) ;
#48359 = CARTESIAN_POINT('',(25.4867638772934,0.799999999999999,43.5851576640878)) ;
#48360 = CARTESIAN_POINT('Origin',(25.3375,0.8,43.6)) ;
#48361 = CARTESIAN_POINT('',(25.1881289970792,0.805251324321435,43.6126778183972)) ;
#48362 = CARTESIAN_POINT('Origin',(25.3375,0.8,43.6)) ;
#48363 = CARTESIAN_POINT('Origin',(25.3375,0.8,43.6)) ;
#48364 = CARTESIAN_POINT('Origin',(25.28125,0.565685424949238,43.0343145750508)) ;
#48365 = CARTESIAN_POINT('',(25.1319861227066,0.576180541321432,43.044809691423)) ;
#48366 = CARTESIAN_POINT('',(25.4305138772934,0.555190308577045,43.0238194586786)) ;
#48367 = CARTESIAN_POINT('Origin',(25.28125,0.565685424949238,43.0343145750508)) ;
#48368 = CARTESIAN_POINT('',(25.1318789970792,0.578363243346464,43.0395658993722)) ;
#48369 = CARTESIAN_POINT('Origin',(25.28125,0.565685424949238,43.0343145750508)) ;
#48370 = CARTESIAN_POINT('Origin',(25.28125,0.565685424949238,43.0343145750508)) ;
#48371 = CARTESIAN_POINT('Origin',(25.225,-8.81745695386094E-16,42.8)) ;
#48372 = CARTESIAN_POINT('',(25.0757361227066,0.0148423359122398,42.8)) ;
#48373 = CARTESIAN_POINT('',(25.3742638772934,-0.0148423359122416,42.8)) ;
#48374 = CARTESIAN_POINT('Origin',(25.225,-8.88178419700125E-16,42.8)) ;
#48375 = CARTESIAN_POINT('',(25.0791439534833,-8.99607909436387E-16,42.7649855216442)) ;
#48376 = CARTESIAN_POINT('Origin',(25.225,-8.88178419700125E-16,42.8)) ;
#48377 = CARTESIAN_POINT('',(25.225,-8.81745695386094E-16,42.65)) ;
#48378 = CARTESIAN_POINT('Origin',(25.225,-8.81745695386094E-16,42.8)) ;
#48379 = CARTESIAN_POINT('',(25.0756289970792,0.012677818397226,42.7947486756786)) ;
#48380 = CARTESIAN_POINT('Origin',(25.225,-8.88178419700125E-16,42.8)) ;
#48381 = CARTESIAN_POINT('Origin',(25.225,-8.88178419700125E-16,42.8)) ;
#48382 = CARTESIAN_POINT('Origin',(25.16875,-0.565685424949239,43.0343145750508)) ;
#48383 = CARTESIAN_POINT('',(25.0194861227066,-0.555190308577046,43.0238194586786)) ;
#48384 = CARTESIAN_POINT('',(25.3180138772934,-0.576180541321433,43.044809691423)) ;
#48385 = CARTESIAN_POINT('Origin',(25.16875,-0.565685424949239,43.0343145750508)) ;
#48386 = CARTESIAN_POINT('',(25.0193789970792,-0.560434100627804,43.0216367566535)) ;
#48387 = CARTESIAN_POINT('Origin',(25.16875,-0.565685424949239,43.0343145750508)) ;
#48388 = CARTESIAN_POINT('Origin',(25.16875,-0.565685424949239,43.0343145750508)) ;
#48389 = CARTESIAN_POINT('Origin',(25.1125,-0.8,43.6)) ;
#48390 = CARTESIAN_POINT('',(24.9632361227066,-0.799999999999999,43.5851576640878)) ;
#48391 = CARTESIAN_POINT('',(25.2617638772934,-0.800000000000001,43.6148423359122)) ;
#48392 = CARTESIAN_POINT('Origin',(25.1125,-0.8,43.6)) ;
#48393 = CARTESIAN_POINT('',(24.9631289970792,-0.805251324321434,43.5873221816028)) ;
#48394 = CARTESIAN_POINT('Origin',(25.1125,-0.8,43.6)) ;
#48395 = CARTESIAN_POINT('Origin',(25.1125,-0.8,43.6)) ;
#48396 = CARTESIAN_POINT('Origin',(25.05625,-0.565685424949238,44.1656854249492)) ;
#48397 = CARTESIAN_POINT('',(24.9069861227066,-0.576180541321437,44.155190308577)) ;
#48398 = CARTESIAN_POINT('',(25.2055138772934,-0.555190308577047,44.1761805413214)) ;
#48399 = CARTESIAN_POINT('Origin',(25.05625,-0.565685424949238,44.1656854249492)) ;
#48400 = CARTESIAN_POINT('',(24.9068789970792,-0.578363243346473,44.1604341006278)) ;
#48401 = CARTESIAN_POINT('Origin',(25.05625,-0.565685424949238,44.1656854249492)) ;
#48402 = CARTESIAN_POINT('Origin',(25.05625,-0.565685424949238,44.1656854249492)) ;
#48403 = CARTESIAN_POINT('Origin',(25.,7.83773951454306E-16,44.4)) ;
#48404 = CARTESIAN_POINT('',(24.8507361227066,-0.0148423359122422,44.4)) ;
#48405 = CARTESIAN_POINT('',(25.1492638772934,0.0148423359122402,44.4)) ;
#48406 = CARTESIAN_POINT('Origin',(25.,8.32667268468867E-16,44.4)) ;
#48407 = CARTESIAN_POINT('',(24.8541439534833,7.65911737404014E-16,44.4350144783558)) ;
#48408 = CARTESIAN_POINT('Origin',(25.,7.7715611723761E-16,44.4)) ;
#48409 = CARTESIAN_POINT('',(25.,7.83773951454306E-16,44.55)) ;
#48410 = CARTESIAN_POINT('Origin',(25.,7.83773951454306E-16,44.4)) ;
#48411 = CARTESIAN_POINT('',(24.8506289970792,-0.0126778183972275,44.4052513243214)) ;
#48412 = CARTESIAN_POINT('Origin',(25.,7.7715611723761E-16,44.4)) ;
#48413 = CARTESIAN_POINT('Origin',(25.,7.7715611723761E-16,44.4)) ;
#48414 = CARTESIAN_POINT('Origin',(24.94375,0.565685424949239,44.1656854249492)) ;
#48415 = CARTESIAN_POINT('',(24.7944861227066,0.555190308577044,44.1761805413214)) ;
#48416 = CARTESIAN_POINT('',(25.0930138772934,0.576180541321431,44.155190308577)) ;
#48417 = CARTESIAN_POINT('Origin',(24.94375,0.565685424949239,44.1656854249492)) ;
#48418 = CARTESIAN_POINT('',(24.7943789970792,0.560434100627806,44.1783632433465)) ;
#48419 = CARTESIAN_POINT('Origin',(24.94375,0.565685424949239,44.1656854249492)) ;
#48420 = CARTESIAN_POINT('Origin',(24.94375,0.565685424949239,44.1656854249492)) ;
#48421 = CARTESIAN_POINT('Origin',(24.8875,0.8,43.6)) ;
#48422 = CARTESIAN_POINT('',(24.7382361227066,0.800000000000001,43.6148423359122)) ;
#48423 = CARTESIAN_POINT('',(25.0367638772934,0.799999999999999,43.5851576640878)) ;
#48424 = CARTESIAN_POINT('Origin',(24.8875,0.8,43.6)) ;
#48425 = CARTESIAN_POINT('',(24.7381289970792,0.805251324321435,43.6126778183972)) ;
#48426 = CARTESIAN_POINT('Origin',(24.8875,0.8,43.6)) ;
#48427 = CARTESIAN_POINT('Origin',(24.8875,0.8,43.6)) ;
#48428 = CARTESIAN_POINT('Origin',(24.83125,0.565685424949238,43.0343145750508)) ;
#48429 = CARTESIAN_POINT('',(24.6819861227066,0.576180541321432,43.044809691423)) ;
#48430 = CARTESIAN_POINT('',(24.9805138772934,0.555190308577045,43.0238194586786)) ;
#48431 = CARTESIAN_POINT('Origin',(24.83125,0.565685424949238,43.0343145750508)) ;
#48432 = CARTESIAN_POINT('',(24.6818789970792,0.578363243346464,43.0395658993722)) ;
#48433 = CARTESIAN_POINT('Origin',(24.83125,0.565685424949238,43.0343145750508)) ;
#48434 = CARTESIAN_POINT('Origin',(24.83125,0.565685424949238,43.0343145750508)) ;
#48435 = CARTESIAN_POINT('Origin',(24.775,-6.85802207522518E-16,42.8)) ;
#48436 = CARTESIAN_POINT('',(24.6257361227066,0.0148423359122406,42.8)) ;
#48437 = CARTESIAN_POINT('',(24.9242638772934,-0.0148423359122418,42.8)) ;
#48438 = CARTESIAN_POINT('Origin',(24.775,-6.66133814775094E-16,42.8)) ;
#48439 = CARTESIAN_POINT('',(24.6291439534833,-7.0366442157281E-16,42.7649855216442)) ;
#48440 = CARTESIAN_POINT('Origin',(24.775,-6.10622663543836E-16,42.8)) ;
#48441 = CARTESIAN_POINT('',(24.775,-6.85802207522518E-16,42.65)) ;
#48442 = CARTESIAN_POINT('Origin',(24.775,-6.85802207522518E-16,42.8)) ;
#48443 = CARTESIAN_POINT('',(24.6256289970792,0.0126778183972263,42.7947486756786)) ;
#48444 = CARTESIAN_POINT('Origin',(24.775,-6.10622663543836E-16,42.8)) ;
#48445 = CARTESIAN_POINT('Origin',(24.775,-6.10622663543836E-16,42.8)) ;
#48446 = CARTESIAN_POINT('Origin',(24.71875,-0.565685424949239,43.0343145750508)) ;
#48447 = CARTESIAN_POINT('',(24.5694861227066,-0.555190308577044,43.0238194586786)) ;
#48448 = CARTESIAN_POINT('',(24.8680138772934,-0.576180541321434,43.044809691423)) ;
#48449 = CARTESIAN_POINT('Origin',(24.71875,-0.565685424949239,43.0343145750508)) ;
#48450 = CARTESIAN_POINT('',(24.5693789970792,-0.560434100627804,43.0216367566535)) ;
#48451 = CARTESIAN_POINT('Origin',(24.71875,-0.565685424949239,43.0343145750508)) ;
#48452 = CARTESIAN_POINT('Origin',(24.71875,-0.565685424949239,43.0343145750508)) ;
#48453 = CARTESIAN_POINT('Origin',(24.6625,-0.8,43.6)) ;
#48454 = CARTESIAN_POINT('',(24.5132361227066,-0.8,43.5851576640878)) ;
#48455 = CARTESIAN_POINT('',(24.8117638772934,-0.8,43.6148423359122)) ;
#48456 = CARTESIAN_POINT('Origin',(24.6625,-0.8,43.6)) ;
#48457 = CARTESIAN_POINT('',(24.5131289970792,-0.805251324321434,43.5873221816028)) ;
#48458 = CARTESIAN_POINT('Origin',(24.6625,-0.8,43.6)) ;
#48459 = CARTESIAN_POINT('Origin',(24.6625,-0.8,43.6)) ;
#48460 = CARTESIAN_POINT('Origin',(24.60625,-0.565685424949238,44.1656854249492)) ;
#48461 = CARTESIAN_POINT('',(24.4569861227066,-0.576180541321437,44.155190308577)) ;
#48462 = CARTESIAN_POINT('',(24.7555138772934,-0.555190308577047,44.1761805413214)) ;
#48463 = CARTESIAN_POINT('Origin',(24.60625,-0.565685424949238,44.1656854249492)) ;
#48464 = CARTESIAN_POINT('',(24.4568789970792,-0.578363243346473,44.1604341006278)) ;
#48465 = CARTESIAN_POINT('Origin',(24.60625,-0.565685424949238,44.1656854249492)) ;
#48466 = CARTESIAN_POINT('Origin',(24.60625,-0.565685424949238,44.1656854249492)) ;
#48467 = CARTESIAN_POINT('Origin',(24.55,5.8783046359073E-16,44.4)) ;
#48468 = CARTESIAN_POINT('',(24.4007361227066,-0.014842335912239,44.4)) ;
#48469 = CARTESIAN_POINT('',(24.6992638772934,0.0148423359122435,44.4)) ;
#48470 = CARTESIAN_POINT('Origin',(24.55,5.55111512312578E-16,44.4)) ;
#48471 = CARTESIAN_POINT('',(24.4041439534833,5.69968249540437E-16,44.4350144783558)) ;
#48472 = CARTESIAN_POINT('Origin',(24.55,4.9960036108132E-16,44.4)) ;
#48473 = CARTESIAN_POINT('',(24.55,5.8783046359073E-16,44.55)) ;
#48474 = CARTESIAN_POINT('Origin',(24.55,5.8783046359073E-16,44.4)) ;
#48475 = CARTESIAN_POINT('',(24.4006289970792,-0.0126778183972271,44.4052513243214)) ;
#48476 = CARTESIAN_POINT('Origin',(24.55,4.9960036108132E-16,44.4)) ;
#48477 = CARTESIAN_POINT('Origin',(24.55,4.9960036108132E-16,44.4)) ;
#48478 = CARTESIAN_POINT('Origin',(24.49375,0.565685424949239,44.1656854249492)) ;
#48479 = CARTESIAN_POINT('',(24.3444861227066,0.555190308577044,44.1761805413214)) ;
#48480 = CARTESIAN_POINT('',(24.6430138772934,0.576180541321431,44.155190308577)) ;
#48481 = CARTESIAN_POINT('Origin',(24.49375,0.565685424949239,44.1656854249492)) ;
#48482 = CARTESIAN_POINT('',(24.3443789970792,0.560434100627805,44.1783632433465)) ;
#48483 = CARTESIAN_POINT('Origin',(24.49375,0.565685424949239,44.1656854249492)) ;
#48484 = CARTESIAN_POINT('Origin',(24.49375,0.565685424949239,44.1656854249492)) ;
#48485 = CARTESIAN_POINT('Origin',(24.4375,0.8,43.6)) ;
#48486 = CARTESIAN_POINT('',(24.2882361227066,0.799999999999999,43.6148423359123)) ;
#48487 = CARTESIAN_POINT('',(24.5867638772934,0.800000000000001,43.5851576640878)) ;
#48488 = CARTESIAN_POINT('Origin',(24.4375,0.8,43.6)) ;
#48489 = CARTESIAN_POINT('',(24.2881289970792,0.805251324321434,43.6126778183972)) ;
#48490 = CARTESIAN_POINT('Origin',(24.4375,0.8,43.6)) ;
#48491 = CARTESIAN_POINT('Origin',(24.4375,0.8,43.6)) ;
#48492 = CARTESIAN_POINT('Origin',(24.38125,0.565685424949238,43.0343145750508)) ;
#48493 = CARTESIAN_POINT('',(24.2319861227066,0.576180541321432,43.044809691423)) ;
#48494 = CARTESIAN_POINT('',(24.5305138772934,0.555190308577044,43.0238194586786)) ;
#48495 = CARTESIAN_POINT('Origin',(24.38125,0.565685424949238,43.0343145750508)) ;
#48496 = CARTESIAN_POINT('',(24.2318789970792,0.578363243346464,43.0395658993722)) ;
#48497 = CARTESIAN_POINT('Origin',(24.38125,0.565685424949238,43.0343145750508)) ;
#48498 = CARTESIAN_POINT('Origin',(24.38125,0.565685424949238,43.0343145750508)) ;
#48499 = CARTESIAN_POINT('Origin',(24.325,-4.89858719658941E-16,42.8)) ;
#48500 = CARTESIAN_POINT('',(24.1757361227066,0.0148423359122407,42.8)) ;
#48501 = CARTESIAN_POINT('',(24.4742638772934,-0.0148423359122417,42.8)) ;
#48502 = CARTESIAN_POINT('Origin',(24.325,-4.44089209850063E-16,42.8)) ;
#48503 = CARTESIAN_POINT('',(24.1791439534833,-5.07720933709234E-16,42.7649855216442)) ;
#48504 = CARTESIAN_POINT('Origin',(24.325,-4.44089209850063E-16,42.8)) ;
#48505 = CARTESIAN_POINT('',(24.325,-4.89858719658941E-16,42.65)) ;
#48506 = CARTESIAN_POINT('Origin',(24.325,-4.89858719658941E-16,42.8)) ;
#48507 = CARTESIAN_POINT('',(24.1756289970792,0.0126778183972273,42.7947486756786)) ;
#48508 = CARTESIAN_POINT('Origin',(24.325,-4.44089209850063E-16,42.8)) ;
#48509 = CARTESIAN_POINT('Origin',(24.325,-4.44089209850063E-16,42.8)) ;
#48510 = CARTESIAN_POINT('Origin',(24.26875,-0.565685424949239,43.0343145750508)) ;
#48511 = CARTESIAN_POINT('',(24.1194861227066,-0.555190308577044,43.0238194586786)) ;
#48512 = CARTESIAN_POINT('',(24.4180138772934,-0.576180541321434,43.044809691423)) ;
#48513 = CARTESIAN_POINT('Origin',(24.26875,-0.565685424949239,43.0343145750508)) ;
#48514 = CARTESIAN_POINT('',(24.1193789970792,-0.560434100627804,43.0216367566535)) ;
#48515 = CARTESIAN_POINT('Origin',(24.26875,-0.565685424949239,43.0343145750508)) ;
#48516 = CARTESIAN_POINT('Origin',(24.26875,-0.565685424949239,43.0343145750508)) ;
#48517 = CARTESIAN_POINT('Origin',(24.2125,-0.8,43.6)) ;
#48518 = CARTESIAN_POINT('',(24.0632361227066,-0.800000000000001,43.5851576640878)) ;
#48519 = CARTESIAN_POINT('',(24.3617638772934,-0.799999999999999,43.6148423359122)) ;
#48520 = CARTESIAN_POINT('Origin',(24.2125,-0.8,43.6)) ;
#48521 = CARTESIAN_POINT('',(24.0631289970792,-0.805251324321435,43.5873221816028)) ;
#48522 = CARTESIAN_POINT('Origin',(24.2125,-0.8,43.6)) ;
#48523 = CARTESIAN_POINT('Origin',(24.2125,-0.8,43.6)) ;
#48524 = CARTESIAN_POINT('Origin',(24.15625,-0.565685424949238,44.1656854249492)) ;
#48525 = CARTESIAN_POINT('',(24.0069861227066,-0.576180541321436,44.155190308577)) ;
#48526 = CARTESIAN_POINT('',(24.3055138772934,-0.555190308577049,44.1761805413214)) ;
#48527 = CARTESIAN_POINT('Origin',(24.15625,-0.565685424949238,44.1656854249492)) ;
#48528 = CARTESIAN_POINT('',(24.0068789970792,-0.578363243346471,44.1604341006278)) ;
#48529 = CARTESIAN_POINT('Origin',(24.15625,-0.565685424949238,44.1656854249492)) ;
#48530 = CARTESIAN_POINT('Origin',(24.15625,-0.565685424949238,44.1656854249492)) ;
#48531 = CARTESIAN_POINT('Origin',(24.1,3.91886975727153E-16,44.4)) ;
#48532 = CARTESIAN_POINT('',(23.9507361227066,-0.014842335912242,44.4)) ;
#48533 = CARTESIAN_POINT('',(24.2492638772934,0.0148423359122394,44.4)) ;
#48534 = CARTESIAN_POINT('Origin',(24.1,4.9960036108132E-16,44.4)) ;
#48535 = CARTESIAN_POINT('',(23.9541439534833,3.74024761676861E-16,44.4350144783558)) ;
#48536 = CARTESIAN_POINT('Origin',(24.1,3.88578058618805E-16,44.4)) ;
#48537 = CARTESIAN_POINT('',(24.1,3.91886975727153E-16,44.55)) ;
#48538 = CARTESIAN_POINT('Origin',(24.1,3.91886975727153E-16,44.4)) ;
#48539 = CARTESIAN_POINT('',(23.9506289970792,-0.0126778183972283,44.4052513243214)) ;
#48540 = CARTESIAN_POINT('Origin',(24.1,3.88578058618805E-16,44.4)) ;
#48541 = CARTESIAN_POINT('Origin',(24.1,3.88578058618805E-16,44.4)) ;
#48542 = CARTESIAN_POINT('Origin',(24.04375,0.565685424949239,44.1656854249492)) ;
#48543 = CARTESIAN_POINT('',(23.8944861227066,0.555190308577044,44.1761805413214)) ;
#48544 = CARTESIAN_POINT('',(24.1930138772934,0.576180541321431,44.155190308577)) ;
#48545 = CARTESIAN_POINT('Origin',(24.04375,0.565685424949239,44.1656854249492)) ;
#48546 = CARTESIAN_POINT('',(23.8943789970792,0.560434100627805,44.1783632433465)) ;
#48547 = CARTESIAN_POINT('Origin',(24.04375,0.565685424949239,44.1656854249492)) ;
#48548 = CARTESIAN_POINT('Origin',(24.04375,0.565685424949239,44.1656854249492)) ;
#48549 = CARTESIAN_POINT('Origin',(23.9875,0.8,43.6)) ;
#48550 = CARTESIAN_POINT('',(23.8382361227066,0.8,43.6148423359122)) ;
#48551 = CARTESIAN_POINT('',(24.1367638772934,0.800000000000001,43.5851576640878)) ;
#48552 = CARTESIAN_POINT('Origin',(23.9875,0.8,43.6)) ;
#48553 = CARTESIAN_POINT('',(23.8381289970792,0.805251324321434,43.6126778183972)) ;
#48554 = CARTESIAN_POINT('Origin',(23.9875,0.8,43.6)) ;
#48555 = CARTESIAN_POINT('Origin',(23.9875,0.8,43.6)) ;
#48556 = CARTESIAN_POINT('Origin',(23.93125,0.565685424949238,43.0343145750508)) ;
#48557 = CARTESIAN_POINT('',(23.7819861227066,0.576180541321434,43.044809691423)) ;
#48558 = CARTESIAN_POINT('',(24.0805138772934,0.555190308577043,43.0238194586786)) ;
#48559 = CARTESIAN_POINT('Origin',(23.93125,0.565685424949238,43.0343145750508)) ;
#48560 = CARTESIAN_POINT('',(23.7818789970792,0.578363243346466,43.0395658993722)) ;
#48561 = CARTESIAN_POINT('Origin',(23.93125,0.565685424949238,43.0343145750508)) ;
#48562 = CARTESIAN_POINT('Origin',(23.93125,0.565685424949238,43.0343145750508)) ;
#48563 = CARTESIAN_POINT('Origin',(23.875,-2.93915231795365E-16,42.8)) ;
#48564 = CARTESIAN_POINT('',(23.7257361227066,0.0148423359122408,42.8)) ;
#48565 = CARTESIAN_POINT('',(24.0242638772934,-0.0148423359122416,42.8)) ;
#48566 = CARTESIAN_POINT('Origin',(23.875,-3.33066907387547E-16,42.8)) ;
#48567 = CARTESIAN_POINT('',(23.7291439534833,-3.11777445845657E-16,42.7649855216442)) ;
#48568 = CARTESIAN_POINT('Origin',(23.875,-2.77555756156289E-16,42.8)) ;
#48569 = CARTESIAN_POINT('',(23.875,-2.93915231795365E-16,42.65)) ;
#48570 = CARTESIAN_POINT('Origin',(23.875,-2.93915231795365E-16,42.8)) ;
#48571 = CARTESIAN_POINT('',(23.7256289970792,0.0126778183972251,42.7947486756786)) ;
#48572 = CARTESIAN_POINT('Origin',(23.875,-2.77555756156289E-16,42.8)) ;
#48573 = CARTESIAN_POINT('Origin',(23.875,-2.77555756156289E-16,42.8)) ;
#48574 = CARTESIAN_POINT('Origin',(23.81875,-0.565685424949239,43.0343145750508)) ;
#48575 = CARTESIAN_POINT('',(23.6694861227066,-0.555190308577045,43.0238194586786)) ;
#48576 = CARTESIAN_POINT('',(23.9680138772934,-0.576180541321433,43.044809691423)) ;
#48577 = CARTESIAN_POINT('Origin',(23.81875,-0.565685424949239,43.0343145750508)) ;
#48578 = CARTESIAN_POINT('',(23.6693789970792,-0.560434100627804,43.0216367566535)) ;
#48579 = CARTESIAN_POINT('Origin',(23.81875,-0.565685424949239,43.0343145750508)) ;
#48580 = CARTESIAN_POINT('Origin',(23.81875,-0.565685424949239,43.0343145750508)) ;
#48581 = CARTESIAN_POINT('Origin',(23.7625,-0.8,43.6)) ;
#48582 = CARTESIAN_POINT('',(23.6132361227066,-0.800000000000001,43.5851576640878)) ;
#48583 = CARTESIAN_POINT('',(23.9117638772934,-0.799999999999999,43.6148423359122)) ;
#48584 = CARTESIAN_POINT('Origin',(23.7625,-0.8,43.6)) ;
#48585 = CARTESIAN_POINT('',(23.6131289970792,-0.805251324321435,43.5873221816028)) ;
#48586 = CARTESIAN_POINT('Origin',(23.7625,-0.8,43.6)) ;
#48587 = CARTESIAN_POINT('Origin',(23.7625,-0.8,43.6)) ;
#48588 = CARTESIAN_POINT('Origin',(23.70625,-0.565685424949238,44.1656854249492)) ;
#48589 = CARTESIAN_POINT('',(23.5569861227066,-0.576180541321436,44.155190308577)) ;
#48590 = CARTESIAN_POINT('',(23.8555138772934,-0.555190308577049,44.1761805413214)) ;
#48591 = CARTESIAN_POINT('Origin',(23.70625,-0.565685424949238,44.1656854249492)) ;
#48592 = CARTESIAN_POINT('',(23.5568789970792,-0.57836324334647,44.1604341006278)) ;
#48593 = CARTESIAN_POINT('Origin',(23.70625,-0.565685424949238,44.1656854249492)) ;
#48594 = CARTESIAN_POINT('Origin',(23.70625,-0.565685424949238,44.1656854249492)) ;
#48595 = CARTESIAN_POINT('Origin',(23.65,1.95943487863577E-16,44.4)) ;
#48596 = CARTESIAN_POINT('',(23.5007361227066,-0.0148423359122428,44.4)) ;
#48597 = CARTESIAN_POINT('',(23.7992638772934,0.0148423359122396,44.4)) ;
#48598 = CARTESIAN_POINT('Origin',(23.65,2.22044604925031E-16,44.4)) ;
#48599 = CARTESIAN_POINT('',(23.5041439534833,1.78081273813284E-16,44.4350144783558)) ;
#48600 = CARTESIAN_POINT('Origin',(23.65,2.22044604925031E-16,44.4)) ;
#48601 = CARTESIAN_POINT('',(23.65,1.95943487863577E-16,44.55)) ;
#48602 = CARTESIAN_POINT('Origin',(23.65,1.95943487863577E-16,44.4)) ;
#48603 = CARTESIAN_POINT('',(23.5006289970792,-0.012677818397231,44.4052513243214)) ;
#48604 = CARTESIAN_POINT('Origin',(23.65,2.22044604925031E-16,44.4)) ;
#48605 = CARTESIAN_POINT('Origin',(23.65,2.22044604925031E-16,44.4)) ;
#48606 = CARTESIAN_POINT('Origin',(23.59375,0.565685424949238,44.1656854249492)) ;
#48607 = CARTESIAN_POINT('',(23.4444861227066,0.555190308577043,44.1761805413214)) ;
#48608 = CARTESIAN_POINT('',(23.7430138772934,0.576180541321433,44.155190308577)) ;
#48609 = CARTESIAN_POINT('Origin',(23.59375,0.565685424949238,44.1656854249492)) ;
#48610 = CARTESIAN_POINT('',(23.4443789970792,0.560434100627803,44.1783632433465)) ;
#48611 = CARTESIAN_POINT('Origin',(23.59375,0.565685424949238,44.1656854249492)) ;
#48612 = CARTESIAN_POINT('Origin',(23.59375,0.565685424949238,44.1656854249492)) ;
#48613 = CARTESIAN_POINT('Origin',(23.5375,0.8,43.6)) ;
#48614 = CARTESIAN_POINT('',(23.3882361227066,0.8,43.6148423359122)) ;
#48615 = CARTESIAN_POINT('',(23.6867638772934,0.8,43.5851576640878)) ;
#48616 = CARTESIAN_POINT('Origin',(23.5375,0.8,43.6)) ;
#48617 = CARTESIAN_POINT('',(23.3881289970792,0.805251324321434,43.6126778183972)) ;
#48618 = CARTESIAN_POINT('Origin',(23.5375,0.8,43.6)) ;
#48619 = CARTESIAN_POINT('Origin',(23.5375,0.8,43.6)) ;
#48620 = CARTESIAN_POINT('Origin',(23.48125,0.565685424949238,43.0343145750508)) ;
#48621 = CARTESIAN_POINT('',(23.3319861227066,0.576180541321433,43.044809691423)) ;
#48622 = CARTESIAN_POINT('',(23.6305138772934,0.555190308577043,43.0238194586786)) ;
#48623 = CARTESIAN_POINT('Origin',(23.48125,0.565685424949238,43.0343145750508)) ;
#48624 = CARTESIAN_POINT('',(23.3318789970792,0.578363243346464,43.0395658993722)) ;
#48625 = CARTESIAN_POINT('Origin',(23.48125,0.565685424949238,43.0343145750508)) ;
#48626 = CARTESIAN_POINT('Origin',(23.48125,0.565685424949238,43.0343145750508)) ;
#48627 = CARTESIAN_POINT('Origin',(23.425,-9.79717439317883E-17,42.8)) ;
#48628 = CARTESIAN_POINT('',(23.2757361227066,0.0148423359122411,42.8)) ;
#48629 = CARTESIAN_POINT('',(23.5742638772934,-0.0148423359122413,42.8)) ;
#48630 = CARTESIAN_POINT('Origin',(23.425,-1.11022302462516E-16,42.8)) ;
#48631 = CARTESIAN_POINT('',(23.2791439534833,-1.15833957982081E-16,42.7649855216442)) ;
#48632 = CARTESIAN_POINT('Origin',(23.425,-5.55111512312578E-17,42.8)) ;
#48633 = CARTESIAN_POINT('',(23.425,-9.79717439317883E-17,42.65)) ;
#48634 = CARTESIAN_POINT('Origin',(23.425,-9.79717439317883E-17,42.8)) ;
#48635 = CARTESIAN_POINT('',(23.2756289970792,0.0126778183972252,42.7947486756786)) ;
#48636 = CARTESIAN_POINT('Origin',(23.425,-5.55111512312578E-17,42.8)) ;
#48637 = CARTESIAN_POINT('Origin',(23.425,-5.55111512312578E-17,42.8)) ;
#48638 = CARTESIAN_POINT('Origin',(23.36875,-0.565685424949238,43.0343145750508)) ;
#48639 = CARTESIAN_POINT('',(23.2194861227066,-0.555190308577045,43.0238194586786)) ;
#48640 = CARTESIAN_POINT('',(23.5180138772934,-0.576180541321432,43.044809691423)) ;
#48641 = CARTESIAN_POINT('Origin',(23.36875,-0.565685424949238,43.0343145750508)) ;
#48642 = CARTESIAN_POINT('',(23.2193789970792,-0.560434100627803,43.0216367566535)) ;
#48643 = CARTESIAN_POINT('Origin',(23.36875,-0.565685424949238,43.0343145750508)) ;
#48644 = CARTESIAN_POINT('Origin',(23.36875,-0.565685424949238,43.0343145750508)) ;
#48645 = CARTESIAN_POINT('Origin',(23.3125,-0.8,43.6)) ;
#48646 = CARTESIAN_POINT('',(23.1632361227066,-0.799999999999999,43.5851576640878)) ;
#48647 = CARTESIAN_POINT('',(23.4617638772934,-0.800000000000001,43.6148423359122)) ;
#48648 = CARTESIAN_POINT('Origin',(23.3125,-0.8,43.6)) ;
#48649 = CARTESIAN_POINT('',(23.1631289970792,-0.805251324321434,43.5873221816028)) ;
#48650 = CARTESIAN_POINT('Origin',(23.3125,-0.8,43.6)) ;
#48651 = CARTESIAN_POINT('Origin',(23.3125,-0.8,43.6)) ;
#48652 = CARTESIAN_POINT('Origin',(23.25625,-0.565685424949238,44.1656854249492)) ;
#48653 = CARTESIAN_POINT('',(23.1069861227066,-0.576180541321436,44.155190308577)) ;
#48654 = CARTESIAN_POINT('',(23.4055138772934,-0.555190308577049,44.1761805413214)) ;
#48655 = CARTESIAN_POINT('Origin',(23.25625,-0.565685424949238,44.1656854249492)) ;
#48656 = CARTESIAN_POINT('',(23.1068789970792,-0.578363243346471,44.1604341006278)) ;
#48657 = CARTESIAN_POINT('Origin',(23.25625,-0.565685424949238,44.1656854249492)) ;
#48658 = CARTESIAN_POINT('Origin',(23.25625,-0.565685424949238,44.1656854249492)) ;
#48659 = CARTESIAN_POINT('Origin',(30.371875,0.282842712474621,44.2828427124746)) ;
#48660 = CARTESIAN_POINT('Origin',(30.34375,0.565685424949243,44.1656854249492)) ;
#48661 = CARTESIAN_POINT('Origin',(30.315625,0.682842712474619,43.8828427124746)) ;
#48662 = CARTESIAN_POINT('Origin',(30.2875,0.8,43.6)) ;
#48663 = CARTESIAN_POINT('Origin',(30.259375,0.682842712474616,43.3171572875254)) ;
#48664 = CARTESIAN_POINT('',(30.0820931715058,0.571828912643789,43.0491462663632)) ;
#48665 = CARTESIAN_POINT('',(30.1100039970792,0.68809403679605,43.3298351059226)) ;
#48666 = CARTESIAN_POINT('Origin',(30.23125,0.565685424949236,43.0343145750508)) ;
#48667 = CARTESIAN_POINT('Origin',(30.23125,0.565685424949236,43.0343145750508)) ;
#48668 = CARTESIAN_POINT('Origin',(30.203125,0.282842712474613,42.9171572875254)) ;
#48669 = CARTESIAN_POINT('',(30.0258431715057,0.0148316913124444,42.8061434876946)) ;
#48670 = CARTESIAN_POINT('',(30.0537539970792,0.295520530871838,42.9224086118468)) ;
#48671 = CARTESIAN_POINT('Origin',(30.175,-1.0325074129014E-14,42.8)) ;
#48672 = CARTESIAN_POINT('Origin',(30.175,-1.0325074129014E-14,42.8)) ;
#48673 = CARTESIAN_POINT('Origin',(30.146875,-0.282842712474623,42.9171572875254)) ;
#48674 = CARTESIAN_POINT('',(29.9695931715058,-0.550853733636784,43.0281710873562)) ;
#48675 = CARTESIAN_POINT('',(29.9975039970792,-0.270164894077399,42.9119059632039)) ;
#48676 = CARTESIAN_POINT('Origin',(30.11875,-0.56568542494924,43.0343145750508)) ;
#48677 = CARTESIAN_POINT('Origin',(30.11875,-0.56568542494924,43.0343145750508)) ;
#48678 = CARTESIAN_POINT('Origin',(30.090625,-0.68284271247462,43.3171572875254)) ;
#48679 = CARTESIAN_POINT('',(29.9133431715058,-0.793856512305449,43.5851683086875)) ;
#48680 = CARTESIAN_POINT('',(29.9412539970792,-0.677591388153187,43.3044794691282)) ;
#48681 = CARTESIAN_POINT('Origin',(30.0625,-0.8,43.6)) ;
#48682 = CARTESIAN_POINT('Origin',(30.0625,-0.8,43.6)) ;
#48683 = CARTESIAN_POINT('Origin',(30.034375,-0.682842712474619,43.8828427124746)) ;
#48684 = CARTESIAN_POINT('',(29.8570931715057,-0.57182891264379,44.1508537336368)) ;
#48685 = CARTESIAN_POINT('',(29.8850039970792,-0.688094036796053,43.8701648940774)) ;
#48686 = CARTESIAN_POINT('Origin',(30.00625,-0.565685424949241,44.1656854249492)) ;
#48687 = CARTESIAN_POINT('Origin',(30.00625,-0.565685424949241,44.1656854249492)) ;
#48688 = CARTESIAN_POINT('Origin',(29.978125,-0.282842712474615,44.2828427124746)) ;
#48689 = CARTESIAN_POINT('',(29.8008431715058,-0.0148316913124417,44.3938565123055)) ;
#48690 = CARTESIAN_POINT('',(29.8287539970792,-0.295520530871839,44.2775913881532)) ;
#48691 = CARTESIAN_POINT('Origin',(29.95,1.26565424807268E-14,44.4)) ;
#48692 = CARTESIAN_POINT('Origin',(29.95,1.26565424807268E-14,44.4)) ;
#48693 = CARTESIAN_POINT('Origin',(29.921875,0.282842712474626,44.2828427124746)) ;
#48694 = CARTESIAN_POINT('',(29.7445931715057,0.55085373363679,44.1718289126438)) ;
#48695 = CARTESIAN_POINT('',(29.7725039970792,0.270164894077401,44.2880940367961)) ;
#48696 = CARTESIAN_POINT('Origin',(29.89375,0.565685424949242,44.1656854249492)) ;
#48697 = CARTESIAN_POINT('Origin',(29.89375,0.565685424949242,44.1656854249492)) ;
#48698 = CARTESIAN_POINT('Origin',(29.865625,0.682842712474621,43.8828427124746)) ;
#48699 = CARTESIAN_POINT('',(29.6883431715058,0.793856512305448,43.6148316913125)) ;
#48700 = CARTESIAN_POINT('',(29.7162539970792,0.677591388153188,43.8955205308718)) ;
#48701 = CARTESIAN_POINT('Origin',(29.8375,0.8,43.6)) ;
#48702 = CARTESIAN_POINT('Origin',(29.8375,0.8,43.6)) ;
#48703 = CARTESIAN_POINT('Origin',(29.809375,0.682842712474618,43.3171572875254)) ;
#48704 = CARTESIAN_POINT('',(29.6320931715058,0.57182891264379,43.0491462663632)) ;
#48705 = CARTESIAN_POINT('',(29.6600039970792,0.688094036796052,43.3298351059226)) ;
#48706 = CARTESIAN_POINT('Origin',(29.78125,0.565685424949238,43.0343145750508)) ;
#48707 = CARTESIAN_POINT('Origin',(29.78125,0.565685424949238,43.0343145750508)) ;
#48708 = CARTESIAN_POINT('Origin',(29.753125,0.282842712474618,42.9171572875254)) ;
#48709 = CARTESIAN_POINT('',(29.5758431715058,0.0148316913124541,42.8061434876946)) ;
#48710 = CARTESIAN_POINT('',(29.6037539970792,0.295520530871842,42.9224086118468)) ;
#48711 = CARTESIAN_POINT('Origin',(29.725,5.55111512312578E-17,42.8)) ;
#48712 = CARTESIAN_POINT('Origin',(29.725,5.55111512312578E-17,42.8)) ;
#48713 = CARTESIAN_POINT('Origin',(29.696875,-0.282842712474618,42.9171572875254)) ;
#48714 = CARTESIAN_POINT('',(29.5195931715058,-0.55085373363678,43.0281710873562)) ;
#48715 = CARTESIAN_POINT('',(29.5475039970792,-0.270164894077394,42.9119059632039)) ;
#48716 = CARTESIAN_POINT('Origin',(29.66875,-0.565685424949235,43.0343145750508)) ;
#48717 = CARTESIAN_POINT('Origin',(29.66875,-0.565685424949235,43.0343145750508)) ;
#48718 = CARTESIAN_POINT('Origin',(29.640625,-0.682842712474618,43.3171572875254)) ;
#48719 = CARTESIAN_POINT('',(29.4633431715058,-0.793856512305448,43.5851683086876)) ;
#48720 = CARTESIAN_POINT('',(29.4912539970792,-0.677591388153185,43.3044794691282)) ;
#48721 = CARTESIAN_POINT('Origin',(29.6125,-0.799999999999998,43.6)) ;
#48722 = CARTESIAN_POINT('Origin',(29.6125,-0.799999999999998,43.6)) ;
#48723 = CARTESIAN_POINT('Origin',(29.584375,-0.682842712474617,43.8828427124746)) ;
#48724 = CARTESIAN_POINT('',(29.4070931715057,-0.571828912643784,44.1508537336368)) ;
#48725 = CARTESIAN_POINT('',(29.4350039970792,-0.688094036796051,43.8701648940774)) ;
#48726 = CARTESIAN_POINT('Origin',(29.55625,-0.565685424949235,44.1656854249492)) ;
#48727 = CARTESIAN_POINT('Origin',(29.55625,-0.565685424949235,44.1656854249492)) ;
#48728 = CARTESIAN_POINT('Origin',(29.528125,-0.282842712474616,44.2828427124746)) ;
#48729 = CARTESIAN_POINT('',(29.3508431715058,-0.0148316913124563,44.3938565123055)) ;
#48730 = CARTESIAN_POINT('',(29.3787539970792,-0.295520530871841,44.2775913881532)) ;
#48731 = CARTESIAN_POINT('Origin',(29.5,-1.49880108324396E-15,44.4)) ;
#48732 = CARTESIAN_POINT('Origin',(29.5,-1.49880108324396E-15,44.4)) ;
#48733 = CARTESIAN_POINT('Origin',(29.471875,0.282842712474621,44.2828427124746)) ;
#48734 = CARTESIAN_POINT('',(29.2945931715057,0.550853733636796,44.1718289126438)) ;
#48735 = CARTESIAN_POINT('',(29.3225039970792,0.270164894077397,44.2880940367961)) ;
#48736 = CARTESIAN_POINT('Origin',(29.44375,0.565685424949242,44.1656854249492)) ;
#48737 = CARTESIAN_POINT('Origin',(29.44375,0.565685424949242,44.1656854249492)) ;
#48738 = CARTESIAN_POINT('Origin',(29.415625,0.682842712474619,43.8828427124746)) ;
#48739 = CARTESIAN_POINT('',(29.2383431715058,0.79385651230545,43.6148316913125)) ;
#48740 = CARTESIAN_POINT('',(29.2662539970792,0.677591388153186,43.8955205308718)) ;
#48741 = CARTESIAN_POINT('Origin',(29.3875,0.8,43.6)) ;
#48742 = CARTESIAN_POINT('Origin',(29.3875,0.8,43.6)) ;
#48743 = CARTESIAN_POINT('Origin',(29.359375,0.682842712474616,43.3171572875254)) ;
#48744 = CARTESIAN_POINT('',(29.1820931715058,0.571828912643789,43.0491462663632)) ;
#48745 = CARTESIAN_POINT('',(29.2100039970792,0.68809403679605,43.3298351059226)) ;
#48746 = CARTESIAN_POINT('Origin',(29.33125,0.565685424949237,43.0343145750508)) ;
#48747 = CARTESIAN_POINT('Origin',(29.33125,0.565685424949237,43.0343145750508)) ;
#48748 = CARTESIAN_POINT('Origin',(29.303125,0.282842712474614,42.9171572875254)) ;
#48749 = CARTESIAN_POINT('',(29.1258431715058,0.0148316913124456,42.8061434876946)) ;
#48750 = CARTESIAN_POINT('',(29.1537539970792,0.295520530871838,42.9224086118468)) ;
#48751 = CARTESIAN_POINT('Origin',(29.275,-9.38138455808257E-15,42.8)) ;
#48752 = CARTESIAN_POINT('Origin',(29.275,-9.38138455808257E-15,42.8)) ;
#48753 = CARTESIAN_POINT('Origin',(29.246875,-0.282842712474623,42.9171572875254)) ;
#48754 = CARTESIAN_POINT('',(29.0695931715058,-0.550853733636788,43.0281710873562)) ;
#48755 = CARTESIAN_POINT('',(29.0975039970792,-0.270164894077398,42.9119059632039)) ;
#48756 = CARTESIAN_POINT('Origin',(29.21875,-0.56568542494924,43.0343145750508)) ;
#48757 = CARTESIAN_POINT('Origin',(29.21875,-0.56568542494924,43.0343145750508)) ;
#48758 = CARTESIAN_POINT('Origin',(29.190625,-0.68284271247462,43.3171572875254)) ;
#48759 = CARTESIAN_POINT('',(29.0133431715058,-0.79385651230545,43.5851683086875)) ;
#48760 = CARTESIAN_POINT('',(29.0412539970792,-0.677591388153187,43.3044794691282)) ;
#48761 = CARTESIAN_POINT('Origin',(29.1625,-0.8,43.6)) ;
#48762 = CARTESIAN_POINT('Origin',(29.1625,-0.8,43.6)) ;
#48763 = CARTESIAN_POINT('Origin',(29.134375,-0.682842712474619,43.8828427124746)) ;
#48764 = CARTESIAN_POINT('',(28.9570931715058,-0.571828912643791,44.1508537336368)) ;
#48765 = CARTESIAN_POINT('',(28.9850039970792,-0.688094036796053,43.8701648940774)) ;
#48766 = CARTESIAN_POINT('Origin',(29.10625,-0.565685424949241,44.1656854249492)) ;
#48767 = CARTESIAN_POINT('Origin',(29.10625,-0.565685424949241,44.1656854249492)) ;
#48768 = CARTESIAN_POINT('Origin',(29.078125,-0.282842712474621,44.2828427124746)) ;
#48769 = CARTESIAN_POINT('',(28.9008431715057,-0.014831691312453,44.3938565123055)) ;
#48770 = CARTESIAN_POINT('',(28.9287539970792,-0.295520530871846,44.2775913881532)) ;
#48771 = CARTESIAN_POINT('Origin',(29.05,1.11022302462516E-15,44.4)) ;
#48772 = CARTESIAN_POINT('Origin',(29.05,1.11022302462516E-15,44.4)) ;
#48773 = CARTESIAN_POINT('Origin',(29.021875,0.28284271247462,44.2828427124746)) ;
#48774 = CARTESIAN_POINT('',(28.8445931715058,0.55085373363679,44.1718289126438)) ;
#48775 = CARTESIAN_POINT('',(28.8725039970792,0.270164894077396,44.2880940367961)) ;
#48776 = CARTESIAN_POINT('Origin',(28.99375,0.565685424949242,44.1656854249492)) ;
#48777 = CARTESIAN_POINT('Origin',(28.99375,0.565685424949242,44.1656854249492)) ;
#48778 = CARTESIAN_POINT('Origin',(28.965625,0.682842712474621,43.8828427124746)) ;
#48779 = CARTESIAN_POINT('',(28.7883431715058,0.793856512305448,43.6148316913125)) ;
#48780 = CARTESIAN_POINT('',(28.8162539970792,0.677591388153188,43.8955205308718)) ;
#48781 = CARTESIAN_POINT('Origin',(28.9375,0.8,43.6)) ;
#48782 = CARTESIAN_POINT('Origin',(28.9375,0.8,43.6)) ;
#48783 = CARTESIAN_POINT('Origin',(28.909375,0.682842712474618,43.3171572875254)) ;
#48784 = CARTESIAN_POINT('',(28.7320931715057,0.571828912643787,43.0491462663632)) ;
#48785 = CARTESIAN_POINT('',(28.7600039970792,0.688094036796052,43.3298351059226)) ;
#48786 = CARTESIAN_POINT('Origin',(28.88125,0.565685424949238,43.0343145750508)) ;
#48787 = CARTESIAN_POINT('Origin',(28.88125,0.565685424949238,43.0343145750508)) ;
#48788 = CARTESIAN_POINT('Origin',(28.853125,0.282842712474619,42.9171572875254)) ;
#48789 = CARTESIAN_POINT('',(28.6758431715058,0.0148316913124594,42.8061434876946)) ;
#48790 = CARTESIAN_POINT('',(28.7037539970792,0.295520530871843,42.9224086118468)) ;
#48791 = CARTESIAN_POINT('Origin',(28.825,4.77395900588817E-15,42.8)) ;
#48792 = CARTESIAN_POINT('Origin',(28.825,4.77395900588817E-15,42.8)) ;
#48793 = CARTESIAN_POINT('Origin',(28.796875,-0.282842712474618,42.9171572875254)) ;
#48794 = CARTESIAN_POINT('',(28.6195931715057,-0.55085373363679,43.0281710873562)) ;
#48795 = CARTESIAN_POINT('',(28.6475039970792,-0.270164894077393,42.9119059632039)) ;
#48796 = CARTESIAN_POINT('Origin',(28.76875,-0.56568542494924,43.0343145750508)) ;
#48797 = CARTESIAN_POINT('Origin',(28.76875,-0.56568542494924,43.0343145750508)) ;
#48798 = CARTESIAN_POINT('Origin',(28.740625,-0.682842712474618,43.3171572875254)) ;
#48799 = CARTESIAN_POINT('',(28.5633431715058,-0.793856512305451,43.5851683086876)) ;
#48800 = CARTESIAN_POINT('',(28.5912539970792,-0.677591388153185,43.3044794691282)) ;
#48801 = CARTESIAN_POINT('Origin',(28.7125,-0.8,43.6)) ;
#48802 = CARTESIAN_POINT('Origin',(28.7125,-0.8,43.6)) ;
#48803 = CARTESIAN_POINT('Origin',(28.684375,-0.682842712474617,43.8828427124746)) ;
#48804 = CARTESIAN_POINT('',(28.5070931715058,-0.571828912643787,44.1508537336368)) ;
#48805 = CARTESIAN_POINT('',(28.5350039970792,-0.688094036796051,43.8701648940774)) ;
#48806 = CARTESIAN_POINT('Origin',(28.65625,-0.565685424949235,44.1656854249492)) ;
#48807 = CARTESIAN_POINT('Origin',(28.65625,-0.565685424949235,44.1656854249492)) ;
#48808 = CARTESIAN_POINT('Origin',(28.628125,-0.282842712474616,44.2828427124746)) ;
#48809 = CARTESIAN_POINT('',(28.4508431715058,-0.0148316913124563,44.3938565123055)) ;
#48810 = CARTESIAN_POINT('',(28.4787539970792,-0.29552053087184,44.2775913881532)) ;
#48811 = CARTESIAN_POINT('Origin',(28.6,-2.22044604925031E-15,44.4)) ;
#48812 = CARTESIAN_POINT('Origin',(28.6,-2.22044604925031E-15,44.4)) ;
#48813 = CARTESIAN_POINT('Origin',(28.571875,0.28284271247462,44.2828427124746)) ;
#48814 = CARTESIAN_POINT('',(28.3945931715058,0.550853733636788,44.1718289126438)) ;
#48815 = CARTESIAN_POINT('',(28.4225039970792,0.270164894077396,44.2880940367961)) ;
#48816 = CARTESIAN_POINT('Origin',(28.54375,0.565685424949242,44.1656854249492)) ;
#48817 = CARTESIAN_POINT('Origin',(28.54375,0.565685424949242,44.1656854249492)) ;
#48818 = CARTESIAN_POINT('Origin',(28.515625,0.682842712474619,43.8828427124746)) ;
#48819 = CARTESIAN_POINT('',(28.3383431715057,0.793856512305449,43.6148316913125)) ;
#48820 = CARTESIAN_POINT('',(28.3662539970792,0.677591388153185,43.8955205308718)) ;
#48821 = CARTESIAN_POINT('Origin',(28.4875,0.8,43.6)) ;
#48822 = CARTESIAN_POINT('Origin',(28.4875,0.8,43.6)) ;
#48823 = CARTESIAN_POINT('Origin',(28.459375,0.682842712474616,43.3171572875254)) ;
#48824 = CARTESIAN_POINT('',(28.2820931715057,0.571828912643789,43.0491462663632)) ;
#48825 = CARTESIAN_POINT('',(28.3100039970792,0.68809403679605,43.3298351059226)) ;
#48826 = CARTESIAN_POINT('Origin',(28.43125,0.565685424949237,43.0343145750508)) ;
#48827 = CARTESIAN_POINT('Origin',(28.43125,0.565685424949237,43.0343145750508)) ;
#48828 = CARTESIAN_POINT('Origin',(28.403125,0.282842712474614,42.9171572875254)) ;
#48829 = CARTESIAN_POINT('',(28.2258431715058,0.0148316913124452,42.8061434876946)) ;
#48830 = CARTESIAN_POINT('',(28.2537539970792,0.295520530871839,42.9224086118468)) ;
#48831 = CARTESIAN_POINT('Origin',(28.375,-9.54791801177635E-15,42.8)) ;
#48832 = CARTESIAN_POINT('Origin',(28.375,-9.54791801177635E-15,42.8)) ;
#48833 = CARTESIAN_POINT('Origin',(28.346875,-0.282842712474623,42.9171572875254)) ;
#48834 = CARTESIAN_POINT('',(28.1695931715057,-0.550853733636789,43.0281710873562)) ;
#48835 = CARTESIAN_POINT('',(28.1975039970792,-0.270164894077398,42.9119059632039)) ;
#48836 = CARTESIAN_POINT('Origin',(28.31875,-0.56568542494924,43.0343145750508)) ;
#48837 = CARTESIAN_POINT('Origin',(28.31875,-0.56568542494924,43.0343145750508)) ;
#48838 = CARTESIAN_POINT('Origin',(28.290625,-0.68284271247462,43.3171572875254)) ;
#48839 = CARTESIAN_POINT('',(28.1133431715058,-0.79385651230545,43.5851683086875)) ;
#48840 = CARTESIAN_POINT('',(28.1412539970792,-0.677591388153187,43.3044794691282)) ;
#48841 = CARTESIAN_POINT('Origin',(28.2625,-0.8,43.6)) ;
#48842 = CARTESIAN_POINT('Origin',(28.2625,-0.8,43.6)) ;
#48843 = CARTESIAN_POINT('Origin',(28.234375,-0.682842712474619,43.8828427124746)) ;
#48844 = CARTESIAN_POINT('',(28.0570931715058,-0.571828912643794,44.1508537336368)) ;
#48845 = CARTESIAN_POINT('',(28.0850039970792,-0.688094036796053,43.8701648940774)) ;
#48846 = CARTESIAN_POINT('Origin',(28.20625,-0.565685424949242,44.1656854249492)) ;
#48847 = CARTESIAN_POINT('Origin',(28.20625,-0.565685424949242,44.1656854249492)) ;
#48848 = CARTESIAN_POINT('Origin',(28.178125,-0.282842712474616,44.2828427124746)) ;
#48849 = CARTESIAN_POINT('',(28.0008431715058,-0.0148316913124424,44.3938565123055)) ;
#48850 = CARTESIAN_POINT('',(28.0287539970792,-0.295520530871839,44.2775913881532)) ;
#48851 = CARTESIAN_POINT('Origin',(28.15,1.19904086659517E-14,44.4)) ;
#48852 = CARTESIAN_POINT('Origin',(28.15,1.19904086659517E-14,44.4)) ;
#48853 = CARTESIAN_POINT('Origin',(28.121875,0.282842712474625,44.2828427124746)) ;
#48854 = CARTESIAN_POINT('',(27.9445931715057,0.55085373363679,44.1718289126438)) ;
#48855 = CARTESIAN_POINT('',(27.9725039970792,0.2701648940774,44.2880940367961)) ;
#48856 = CARTESIAN_POINT('Origin',(28.09375,0.565685424949242,44.1656854249492)) ;
#48857 = CARTESIAN_POINT('Origin',(28.09375,0.565685424949242,44.1656854249492)) ;
#48858 = CARTESIAN_POINT('Origin',(28.065625,0.682842712474621,43.8828427124746)) ;
#48859 = CARTESIAN_POINT('',(27.8883431715058,0.793856512305448,43.6148316913124)) ;
#48860 = CARTESIAN_POINT('',(27.9162539970792,0.677591388153188,43.8955205308718)) ;
#48861 = CARTESIAN_POINT('Origin',(28.0375,0.8,43.6)) ;
#48862 = CARTESIAN_POINT('Origin',(28.0375,0.8,43.6)) ;
#48863 = CARTESIAN_POINT('Origin',(28.009375,0.682842712474619,43.3171572875254)) ;
#48864 = CARTESIAN_POINT('',(27.8320931715058,0.571828912643788,43.0491462663632)) ;
#48865 = CARTESIAN_POINT('',(27.8600039970792,0.688094036796052,43.3298351059226)) ;
#48866 = CARTESIAN_POINT('Origin',(27.98125,0.565685424949239,43.0343145750508)) ;
#48867 = CARTESIAN_POINT('Origin',(27.98125,0.565685424949239,43.0343145750508)) ;
#48868 = CARTESIAN_POINT('Origin',(27.953125,0.282842712474619,42.9171572875254)) ;
#48869 = CARTESIAN_POINT('',(27.7758431715058,0.01483169131246,42.8061434876946)) ;
#48870 = CARTESIAN_POINT('',(27.8037539970792,0.295520530871844,42.9224086118468)) ;
#48871 = CARTESIAN_POINT('Origin',(27.925,5.21804821573824E-15,42.8)) ;
#48872 = CARTESIAN_POINT('Origin',(27.925,5.21804821573824E-15,42.8)) ;
#48873 = CARTESIAN_POINT('Origin',(27.896875,-0.282842712474618,42.9171572875254)) ;
#48874 = CARTESIAN_POINT('',(27.7195931715058,-0.550853733636787,43.0281710873562)) ;
#48875 = CARTESIAN_POINT('',(27.7475039970792,-0.270164894077393,42.9119059632039)) ;
#48876 = CARTESIAN_POINT('Origin',(27.86875,-0.565685424949239,43.0343145750508)) ;
#48877 = CARTESIAN_POINT('Origin',(27.86875,-0.565685424949239,43.0343145750508)) ;
#48878 = CARTESIAN_POINT('Origin',(27.840625,-0.682842712474618,43.3171572875254)) ;
#48879 = CARTESIAN_POINT('',(27.6633431715058,-0.793856512305451,43.5851683086875)) ;
#48880 = CARTESIAN_POINT('',(27.6912539970792,-0.677591388153184,43.3044794691282)) ;
#48881 = CARTESIAN_POINT('Origin',(27.8125,-0.8,43.6)) ;
#48882 = CARTESIAN_POINT('Origin',(27.8125,-0.8,43.6)) ;
#48883 = CARTESIAN_POINT('Origin',(27.784375,-0.682842712474618,43.8828427124746)) ;
#48884 = CARTESIAN_POINT('',(27.6070931715057,-0.571828912643784,44.1508537336368)) ;
#48885 = CARTESIAN_POINT('',(27.6350039970792,-0.688094036796051,43.8701648940774)) ;
#48886 = CARTESIAN_POINT('Origin',(27.75625,-0.565685424949235,44.1656854249492)) ;
#48887 = CARTESIAN_POINT('Origin',(27.75625,-0.565685424949235,44.1656854249492)) ;
#48888 = CARTESIAN_POINT('Origin',(27.728125,-0.282842712474617,44.2828427124746)) ;
#48889 = CARTESIAN_POINT('',(27.5508431715058,-0.0148316913124567,44.3938565123055)) ;
#48890 = CARTESIAN_POINT('',(27.5787539970792,-0.295520530871841,44.2775913881532)) ;
#48891 = CARTESIAN_POINT('Origin',(27.7,-1.94289029309402E-15,44.4)) ;
#48892 = CARTESIAN_POINT('Origin',(27.7,-1.94289029309402E-15,44.4)) ;
#48893 = CARTESIAN_POINT('Origin',(27.671875,0.28284271247462,44.2828427124746)) ;
#48894 = CARTESIAN_POINT('',(27.4945931715057,0.550853733636784,44.1718289126438)) ;
#48895 = CARTESIAN_POINT('',(27.5225039970792,0.270164894077395,44.2880940367961)) ;
#48896 = CARTESIAN_POINT('Origin',(27.64375,0.565685424949235,44.1656854249492)) ;
#48897 = CARTESIAN_POINT('Origin',(27.64375,0.565685424949235,44.1656854249492)) ;
#48898 = CARTESIAN_POINT('Origin',(27.615625,0.682842712474619,43.8828427124746)) ;
#48899 = CARTESIAN_POINT('',(27.4383431715057,0.79385651230545,43.6148316913124)) ;
#48900 = CARTESIAN_POINT('',(27.4662539970792,0.677591388153186,43.8955205308718)) ;
#48901 = CARTESIAN_POINT('Origin',(27.5875,0.799999999999999,43.6)) ;
#48902 = CARTESIAN_POINT('Origin',(27.5875,0.799999999999999,43.6)) ;
#48903 = CARTESIAN_POINT('Origin',(27.559375,0.682842712474619,43.3171572875254)) ;
#48904 = CARTESIAN_POINT('',(27.3820931715058,0.571828912643791,43.0491462663632)) ;
#48905 = CARTESIAN_POINT('',(27.4100039970792,0.688094036796052,43.3298351059226)) ;
#48906 = CARTESIAN_POINT('Origin',(27.53125,0.565685424949239,43.0343145750508)) ;
#48907 = CARTESIAN_POINT('Origin',(27.53125,0.565685424949239,43.0343145750508)) ;
#48908 = CARTESIAN_POINT('Origin',(27.503125,0.282842712474616,42.9171572875254)) ;
#48909 = CARTESIAN_POINT('',(27.3258431715058,0.0148316913124495,42.8061434876946)) ;
#48910 = CARTESIAN_POINT('',(27.3537539970792,0.29552053087184,42.9224086118468)) ;
#48911 = CARTESIAN_POINT('Origin',(27.475,-4.49640324973188E-15,42.8)) ;
#48912 = CARTESIAN_POINT('Origin',(27.475,-4.49640324973188E-15,42.8)) ;
#48913 = CARTESIAN_POINT('Origin',(27.446875,-0.282842712474622,42.9171572875254)) ;
#48914 = CARTESIAN_POINT('',(27.2695931715058,-0.550853733636784,43.0281710873562)) ;
#48915 = CARTESIAN_POINT('',(27.2975039970792,-0.270164894077398,42.9119059632039)) ;
#48916 = CARTESIAN_POINT('Origin',(27.41875,-0.56568542494924,43.0343145750508)) ;
#48917 = CARTESIAN_POINT('Origin',(27.41875,-0.56568542494924,43.0343145750508)) ;
#48918 = CARTESIAN_POINT('Origin',(27.390625,-0.68284271247462,43.3171572875254)) ;
#48919 = CARTESIAN_POINT('',(27.2133431715057,-0.793856512305449,43.5851683086875)) ;
#48920 = CARTESIAN_POINT('',(27.2412539970792,-0.677591388153186,43.3044794691282)) ;
#48921 = CARTESIAN_POINT('Origin',(27.3625,-0.8,43.6)) ;
#48922 = CARTESIAN_POINT('Origin',(27.3625,-0.8,43.6)) ;
#48923 = CARTESIAN_POINT('Origin',(27.334375,-0.682842712474618,43.8828427124746)) ;
#48924 = CARTESIAN_POINT('',(27.1570931715057,-0.571828912643786,44.1508537336368)) ;
#48925 = CARTESIAN_POINT('',(27.1850039970792,-0.688094036796051,43.8701648940774)) ;
#48926 = CARTESIAN_POINT('Origin',(27.30625,-0.565685424949237,44.1656854249492)) ;
#48927 = CARTESIAN_POINT('Origin',(27.30625,-0.565685424949237,44.1656854249492)) ;
#48928 = CARTESIAN_POINT('Origin',(27.278125,-0.282842712474617,44.2828427124746)) ;
#48929 = CARTESIAN_POINT('',(27.1008431715058,-0.0148316913124573,44.3938565123055)) ;
#48930 = CARTESIAN_POINT('',(27.1287539970792,-0.295520530871842,44.2775913881532)) ;
#48931 = CARTESIAN_POINT('Origin',(27.25,-2.55351295663786E-15,44.4)) ;
#48932 = CARTESIAN_POINT('Origin',(27.25,-2.55351295663786E-15,44.4)) ;
#48933 = CARTESIAN_POINT('Origin',(27.221875,0.28284271247462,44.2828427124746)) ;
#48934 = CARTESIAN_POINT('',(27.0445931715057,0.550853733636785,44.1718289126438)) ;
#48935 = CARTESIAN_POINT('',(27.0725039970792,0.270164894077396,44.2880940367961)) ;
#48936 = CARTESIAN_POINT('Origin',(27.19375,0.565685424949235,44.1656854249492)) ;
#48937 = CARTESIAN_POINT('Origin',(27.19375,0.565685424949235,44.1656854249492)) ;
#48938 = CARTESIAN_POINT('Origin',(27.165625,0.682842712474619,43.8828427124746)) ;
#48939 = CARTESIAN_POINT('',(26.9883431715058,0.793856512305447,43.6148316913124)) ;
#48940 = CARTESIAN_POINT('',(27.0162539970792,0.677591388153186,43.8955205308718)) ;
#48941 = CARTESIAN_POINT('Origin',(27.1375,0.799999999999999,43.6)) ;
#48942 = CARTESIAN_POINT('Origin',(27.1375,0.799999999999999,43.6)) ;
#48943 = CARTESIAN_POINT('Origin',(27.109375,0.682842712474619,43.3171572875254)) ;
#48944 = CARTESIAN_POINT('',(26.9320931715058,0.571828912643791,43.0491462663632)) ;
#48945 = CARTESIAN_POINT('',(26.9600039970792,0.688094036796053,43.3298351059226)) ;
#48946 = CARTESIAN_POINT('Origin',(27.08125,0.565685424949239,43.0343145750508)) ;
#48947 = CARTESIAN_POINT('Origin',(27.08125,0.565685424949239,43.0343145750508)) ;
#48948 = CARTESIAN_POINT('Origin',(27.053125,0.282842712474619,42.9171572875254)) ;
#48949 = CARTESIAN_POINT('',(26.8758431715058,0.0148316913124561,42.8061434876946)) ;
#48950 = CARTESIAN_POINT('',(26.9037539970792,0.295520530871843,42.9224086118468)) ;
#48951 = CARTESIAN_POINT('Origin',(27.025,1.49880108324396E-15,42.8)) ;
#48952 = CARTESIAN_POINT('Origin',(27.025,1.49880108324396E-15,42.8)) ;
#48953 = CARTESIAN_POINT('Origin',(26.996875,-0.282842712474619,42.9171572875254)) ;
#48954 = CARTESIAN_POINT('',(26.8195931715057,-0.550853733636788,43.0281710873562)) ;
#48955 = CARTESIAN_POINT('',(26.8475039970792,-0.270164894077394,42.9119059632039)) ;
#48956 = CARTESIAN_POINT('Origin',(26.96875,-0.56568542494924,43.0343145750508)) ;
#48957 = CARTESIAN_POINT('Origin',(26.96875,-0.56568542494924,43.0343145750508)) ;
#48958 = CARTESIAN_POINT('Origin',(26.940625,-0.68284271247462,43.3171572875254)) ;
#48959 = CARTESIAN_POINT('',(26.7633431715058,-0.79385651230545,43.5851683086875)) ;
#48960 = CARTESIAN_POINT('',(26.7912539970792,-0.677591388153187,43.3044794691282)) ;
#48961 = CARTESIAN_POINT('Origin',(26.9125,-0.8,43.6)) ;
#48962 = CARTESIAN_POINT('Origin',(26.9125,-0.8,43.6)) ;
#48963 = CARTESIAN_POINT('Origin',(26.884375,-0.682842712474618,43.8828427124746)) ;
#48964 = CARTESIAN_POINT('',(26.7070931715058,-0.571828912643786,44.1508537336368)) ;
#48965 = CARTESIAN_POINT('',(26.7350039970792,-0.688094036796051,43.8701648940774)) ;
#48966 = CARTESIAN_POINT('Origin',(26.85625,-0.565685424949237,44.1656854249492)) ;
#48967 = CARTESIAN_POINT('Origin',(26.85625,-0.565685424949237,44.1656854249492)) ;
#48968 = CARTESIAN_POINT('Origin',(26.828125,-0.282842712474617,44.2828427124746)) ;
#48969 = CARTESIAN_POINT('',(26.6508431715058,-0.0148316913124579,44.3938565123055)) ;
#48970 = CARTESIAN_POINT('',(26.6787539970792,-0.295520530871842,44.2775913881532)) ;
#48971 = CARTESIAN_POINT('Origin',(26.8,-2.99760216648792E-15,44.4)) ;
#48972 = CARTESIAN_POINT('Origin',(26.8,-2.99760216648792E-15,44.4)) ;
#48973 = CARTESIAN_POINT('Origin',(26.771875,0.28284271247462,44.2828427124746)) ;
#48974 = CARTESIAN_POINT('',(26.5945931715058,0.550853733636778,44.1718289126438)) ;
#48975 = CARTESIAN_POINT('',(26.6225039970792,0.270164894077396,44.2880940367961)) ;
#48976 = CARTESIAN_POINT('Origin',(26.74375,0.565685424949235,44.1656854249492)) ;
#48977 = CARTESIAN_POINT('Origin',(26.74375,0.565685424949235,44.1656854249492)) ;
#48978 = CARTESIAN_POINT('Origin',(26.715625,0.682842712474619,43.8828427124746)) ;
#48979 = CARTESIAN_POINT('',(26.5383431715058,0.79385651230545,43.6148316913124)) ;
#48980 = CARTESIAN_POINT('',(26.5662539970792,0.677591388153185,43.8955205308718)) ;
#48981 = CARTESIAN_POINT('Origin',(26.6875,0.799999999999999,43.6)) ;
#48982 = CARTESIAN_POINT('Origin',(26.6875,0.799999999999999,43.6)) ;
#48983 = CARTESIAN_POINT('Origin',(26.659375,0.682842712474619,43.3171572875254)) ;
#48984 = CARTESIAN_POINT('',(26.4820931715057,0.571828912643788,43.0491462663632)) ;
#48985 = CARTESIAN_POINT('',(26.5100039970792,0.688094036796052,43.3298351059226)) ;
#48986 = CARTESIAN_POINT('Origin',(26.63125,0.565685424949239,43.0343145750508)) ;
#48987 = CARTESIAN_POINT('Origin',(26.63125,0.565685424949239,43.0343145750508)) ;
#48988 = CARTESIAN_POINT('Origin',(26.603125,0.282842712474617,42.9171572875254)) ;
#48989 = CARTESIAN_POINT('',(26.4258431715058,0.0148316913124502,42.8061434876946)) ;
#48990 = CARTESIAN_POINT('',(26.4537539970792,0.295520530871841,42.9224086118468)) ;
#48991 = CARTESIAN_POINT('Origin',(26.575,-4.44089209850063E-15,42.8)) ;
#48992 = CARTESIAN_POINT('Origin',(26.575,-4.44089209850063E-15,42.8)) ;
#48993 = CARTESIAN_POINT('Origin',(26.546875,-0.282842712474622,42.9171572875254)) ;
#48994 = CARTESIAN_POINT('',(26.3695931715057,-0.550853733636787,43.0281710873562)) ;
#48995 = CARTESIAN_POINT('',(26.3975039970792,-0.270164894077397,42.9119059632039)) ;
#48996 = CARTESIAN_POINT('Origin',(26.51875,-0.565685424949239,43.0343145750508)) ;
#48997 = CARTESIAN_POINT('Origin',(26.51875,-0.565685424949239,43.0343145750508)) ;
#48998 = CARTESIAN_POINT('Origin',(26.490625,-0.68284271247462,43.3171572875254)) ;
#48999 = CARTESIAN_POINT('',(26.3133431715058,-0.79385651230545,43.5851683086875)) ;
#49000 = CARTESIAN_POINT('',(26.3412539970792,-0.677591388153186,43.3044794691282)) ;
#49001 = CARTESIAN_POINT('Origin',(26.4625,-0.8,43.6)) ;
#49002 = CARTESIAN_POINT('Origin',(26.4625,-0.8,43.6)) ;
#49003 = CARTESIAN_POINT('Origin',(26.434375,-0.682842712474618,43.8828427124746)) ;
#49004 = CARTESIAN_POINT('',(26.2570931715058,-0.571828912643789,44.1508537336368)) ;
#49005 = CARTESIAN_POINT('',(26.2850039970792,-0.688094036796051,43.8701648940774)) ;
#49006 = CARTESIAN_POINT('Origin',(26.40625,-0.565685424949237,44.1656854249492)) ;
#49007 = CARTESIAN_POINT('Origin',(26.40625,-0.565685424949237,44.1656854249492)) ;
#49008 = CARTESIAN_POINT('Origin',(26.378125,-0.282842712474617,44.2828427124746)) ;
#49009 = CARTESIAN_POINT('',(26.2008431715058,-0.0148316913124567,44.3938565123055)) ;
#49010 = CARTESIAN_POINT('',(26.2287539970792,-0.295520530871841,44.2775913881532)) ;
#49011 = CARTESIAN_POINT('Origin',(26.35,-2.66453525910038E-15,44.4)) ;
#49012 = CARTESIAN_POINT('Origin',(26.35,-2.66453525910038E-15,44.4)) ;
#49013 = CARTESIAN_POINT('Origin',(26.321875,0.282842712474619,44.2828427124746)) ;
#49014 = CARTESIAN_POINT('',(26.1445931715058,0.550853733636787,44.1718289126438)) ;
#49015 = CARTESIAN_POINT('',(26.1725039970792,0.270164894077395,44.2880940367961)) ;
#49016 = CARTESIAN_POINT('Origin',(26.29375,0.565685424949241,44.1656854249492)) ;
#49017 = CARTESIAN_POINT('Origin',(26.29375,0.565685424949241,44.1656854249492)) ;
#49018 = CARTESIAN_POINT('Origin',(26.265625,0.682842712474619,43.8828427124746)) ;
#49019 = CARTESIAN_POINT('',(26.0883431715058,0.79385651230545,43.6148316913125)) ;
#49020 = CARTESIAN_POINT('',(26.1162539970792,0.677591388153185,43.8955205308718)) ;
#49021 = CARTESIAN_POINT('Origin',(26.2375,0.8,43.6)) ;
#49022 = CARTESIAN_POINT('Origin',(26.2375,0.8,43.6)) ;
#49023 = CARTESIAN_POINT('Origin',(26.209375,0.682842712474619,43.3171572875254)) ;
#49024 = CARTESIAN_POINT('',(26.0320931715057,0.571828912643787,43.0491462663632)) ;
#49025 = CARTESIAN_POINT('',(26.0600039970792,0.688094036796052,43.3298351059226)) ;
#49026 = CARTESIAN_POINT('Origin',(26.18125,0.565685424949238,43.0343145750508)) ;
#49027 = CARTESIAN_POINT('Origin',(26.18125,0.565685424949238,43.0343145750508)) ;
#49028 = CARTESIAN_POINT('Origin',(26.153125,0.28284271247462,42.9171572875254)) ;
#49029 = CARTESIAN_POINT('',(25.9758431715058,0.0148316913124558,42.8061434876946)) ;
#49030 = CARTESIAN_POINT('',(26.0037539970792,0.295520530871845,42.9224086118468)) ;
#49031 = CARTESIAN_POINT('Origin',(26.125,1.33226762955019E-15,42.8)) ;
#49032 = CARTESIAN_POINT('Origin',(26.125,1.33226762955019E-15,42.8)) ;
#49033 = CARTESIAN_POINT('Origin',(26.096875,-0.282842712474619,42.9171572875254)) ;
#49034 = CARTESIAN_POINT('',(25.9195931715057,-0.550853733636788,43.0281710873562)) ;
#49035 = CARTESIAN_POINT('',(25.9475039970792,-0.270164894077395,42.9119059632039)) ;
#49036 = CARTESIAN_POINT('Origin',(26.06875,-0.565685424949239,43.0343145750508)) ;
#49037 = CARTESIAN_POINT('Origin',(26.06875,-0.565685424949239,43.0343145750508)) ;
#49038 = CARTESIAN_POINT('Origin',(26.040625,-0.68284271247462,43.3171572875254)) ;
#49039 = CARTESIAN_POINT('',(25.8633431715058,-0.79385651230545,43.5851683086875)) ;
#49040 = CARTESIAN_POINT('',(25.8912539970792,-0.677591388153186,43.3044794691282)) ;
#49041 = CARTESIAN_POINT('Origin',(26.0125,-0.8,43.6)) ;
#49042 = CARTESIAN_POINT('Origin',(26.0125,-0.8,43.6)) ;
#49043 = CARTESIAN_POINT('Origin',(25.984375,-0.682842712474618,43.8828427124746)) ;
#49044 = CARTESIAN_POINT('',(25.8070931715058,-0.571828912643789,44.1508537336368)) ;
#49045 = CARTESIAN_POINT('',(25.8350039970792,-0.688094036796052,43.8701648940774)) ;
#49046 = CARTESIAN_POINT('Origin',(25.95625,-0.565685424949237,44.1656854249492)) ;
#49047 = CARTESIAN_POINT('Origin',(25.95625,-0.565685424949237,44.1656854249492)) ;
#49048 = CARTESIAN_POINT('Origin',(25.928125,-0.282842712474617,44.2828427124746)) ;
#49049 = CARTESIAN_POINT('',(25.7508431715058,-0.0148316913124584,44.3938565123055)) ;
#49050 = CARTESIAN_POINT('',(25.7787539970792,-0.295520530871841,44.2775913881532)) ;
#49051 = CARTESIAN_POINT('Origin',(25.9,-3.44169137633799E-15,44.4)) ;
#49052 = CARTESIAN_POINT('Origin',(25.9,-3.44169137633799E-15,44.4)) ;
#49053 = CARTESIAN_POINT('Origin',(25.871875,0.282842712474619,44.2828427124746)) ;
#49054 = CARTESIAN_POINT('',(25.6945931715057,0.550853733636793,44.1718289126438)) ;
#49055 = CARTESIAN_POINT('',(25.7225039970792,0.270164894077394,44.2880940367961)) ;
#49056 = CARTESIAN_POINT('Origin',(25.84375,0.565685424949241,44.1656854249492)) ;
#49057 = CARTESIAN_POINT('Origin',(25.84375,0.565685424949241,44.1656854249492)) ;
#49058 = CARTESIAN_POINT('Origin',(25.815625,0.682842712474619,43.8828427124746)) ;
#49059 = CARTESIAN_POINT('',(25.6383431715058,0.79385651230545,43.6148316913125)) ;
#49060 = CARTESIAN_POINT('',(25.6662539970792,0.677591388153185,43.8955205308718)) ;
#49061 = CARTESIAN_POINT('Origin',(25.7875,0.8,43.6)) ;
#49062 = CARTESIAN_POINT('Origin',(25.7875,0.8,43.6)) ;
#49063 = CARTESIAN_POINT('Origin',(25.759375,0.682842712474619,43.3171572875254)) ;
#49064 = CARTESIAN_POINT('',(25.5820931715058,0.571828912643787,43.0491462663632)) ;
#49065 = CARTESIAN_POINT('',(25.6100039970792,0.688094036796052,43.3298351059226)) ;
#49066 = CARTESIAN_POINT('Origin',(25.73125,0.565685424949238,43.0343145750508)) ;
#49067 = CARTESIAN_POINT('Origin',(25.73125,0.565685424949238,43.0343145750508)) ;
#49068 = CARTESIAN_POINT('Origin',(25.703125,0.282842712474617,42.9171572875254)) ;
#49069 = CARTESIAN_POINT('',(25.5258431715058,0.0148316913124512,42.8061434876946)) ;
#49070 = CARTESIAN_POINT('',(25.5537539970792,0.295520530871842,42.9224086118468)) ;
#49071 = CARTESIAN_POINT('Origin',(25.675,-3.60822483003176E-15,42.8)) ;
#49072 = CARTESIAN_POINT('Origin',(25.675,-3.60822483003176E-15,42.8)) ;
#49073 = CARTESIAN_POINT('Origin',(25.646875,-0.282842712474622,42.9171572875254)) ;
#49074 = CARTESIAN_POINT('',(25.4695931715058,-0.550853733636783,43.0281710873562)) ;
#49075 = CARTESIAN_POINT('',(25.4975039970792,-0.270164894077397,42.9119059632039)) ;
#49076 = CARTESIAN_POINT('Origin',(25.61875,-0.565685424949239,43.0343145750508)) ;
#49077 = CARTESIAN_POINT('Origin',(25.61875,-0.565685424949239,43.0343145750508)) ;
#49078 = CARTESIAN_POINT('Origin',(25.590625,-0.68284271247462,43.3171572875254)) ;
#49079 = CARTESIAN_POINT('',(25.4133431715058,-0.793856512305449,43.5851683086875)) ;
#49080 = CARTESIAN_POINT('',(25.4412539970792,-0.677591388153186,43.3044794691282)) ;
#49081 = CARTESIAN_POINT('Origin',(25.5625,-0.8,43.6)) ;
#49082 = CARTESIAN_POINT('Origin',(25.5625,-0.8,43.6)) ;
#49083 = CARTESIAN_POINT('Origin',(25.534375,-0.682842712474618,43.8828427124746)) ;
#49084 = CARTESIAN_POINT('',(25.3570931715057,-0.571828912643786,44.1508537336368)) ;
#49085 = CARTESIAN_POINT('',(25.3850039970792,-0.688094036796051,43.8701648940774)) ;
#49086 = CARTESIAN_POINT('Origin',(25.50625,-0.565685424949237,44.1656854249492)) ;
#49087 = CARTESIAN_POINT('Origin',(25.50625,-0.565685424949237,44.1656854249492)) ;
#49088 = CARTESIAN_POINT('Origin',(25.478125,-0.282842712474617,44.2828427124746)) ;
#49089 = CARTESIAN_POINT('',(25.3008431715058,-0.0148316913124581,44.3938565123055)) ;
#49090 = CARTESIAN_POINT('',(25.3287539970792,-0.295520530871842,44.2775913881532)) ;
#49091 = CARTESIAN_POINT('Origin',(25.45,-3.38618022510673E-15,44.4)) ;
#49092 = CARTESIAN_POINT('Origin',(25.45,-3.38618022510673E-15,44.4)) ;
#49093 = CARTESIAN_POINT('Origin',(25.421875,0.28284271247462,44.2828427124746)) ;
#49094 = CARTESIAN_POINT('',(25.2445931715057,0.550853733636795,44.1718289126438)) ;
#49095 = CARTESIAN_POINT('',(25.2725039970792,0.270164894077395,44.2880940367961)) ;
#49096 = CARTESIAN_POINT('Origin',(25.39375,0.565685424949243,44.1656854249492)) ;
#49097 = CARTESIAN_POINT('Origin',(25.39375,0.565685424949243,44.1656854249492)) ;
#49098 = CARTESIAN_POINT('Origin',(25.365625,0.68284271247462,43.8828427124746)) ;
#49099 = CARTESIAN_POINT('',(25.1883431715058,0.79385651230545,43.6148316913125)) ;
#49100 = CARTESIAN_POINT('',(25.2162539970792,0.677591388153186,43.8955205308718)) ;
#49101 = CARTESIAN_POINT('Origin',(25.3375,0.8,43.6)) ;
#49102 = CARTESIAN_POINT('Origin',(25.3375,0.8,43.6)) ;
#49103 = CARTESIAN_POINT('Origin',(25.309375,0.682842712474619,43.3171572875254)) ;
#49104 = CARTESIAN_POINT('',(25.1320931715058,0.57182891264379,43.0491462663632)) ;
#49105 = CARTESIAN_POINT('',(25.1600039970792,0.688094036796053,43.3298351059226)) ;
#49106 = CARTESIAN_POINT('Origin',(25.28125,0.565685424949238,43.0343145750508)) ;
#49107 = CARTESIAN_POINT('Origin',(25.28125,0.565685424949238,43.0343145750508)) ;
#49108 = CARTESIAN_POINT('Origin',(25.253125,0.282842712474619,42.9171572875254)) ;
#49109 = CARTESIAN_POINT('',(25.0758431715058,0.0148316913124534,42.8061434876946)) ;
#49110 = CARTESIAN_POINT('',(25.1037539970792,0.295520530871843,42.9224086118468)) ;
#49111 = CARTESIAN_POINT('Origin',(25.225,-5.55111512312578E-16,42.8)) ;
#49112 = CARTESIAN_POINT('Origin',(25.225,-5.55111512312578E-16,42.8)) ;
#49113 = CARTESIAN_POINT('Origin',(25.196875,-0.28284271247462,42.9171572875254)) ;
#49114 = CARTESIAN_POINT('',(25.0195931715058,-0.550853733636783,43.0281710873562)) ;
#49115 = CARTESIAN_POINT('',(25.0475039970792,-0.270164894077396,42.9119059632039)) ;
#49116 = CARTESIAN_POINT('Origin',(25.16875,-0.565685424949239,43.0343145750508)) ;
#49117 = CARTESIAN_POINT('Origin',(25.16875,-0.565685424949239,43.0343145750508)) ;
#49118 = CARTESIAN_POINT('Origin',(25.140625,-0.68284271247462,43.3171572875254)) ;
#49119 = CARTESIAN_POINT('',(24.9633431715058,-0.79385651230545,43.5851683086875)) ;
#49120 = CARTESIAN_POINT('',(24.9912539970792,-0.677591388153186,43.3044794691282)) ;
#49121 = CARTESIAN_POINT('Origin',(25.1125,-0.8,43.6)) ;
#49122 = CARTESIAN_POINT('Origin',(25.1125,-0.8,43.6)) ;
#49123 = CARTESIAN_POINT('Origin',(25.084375,-0.682842712474619,43.8828427124746)) ;
#49124 = CARTESIAN_POINT('',(24.9070931715057,-0.571828912643791,44.1508537336368)) ;
#49125 = CARTESIAN_POINT('',(24.9350039970792,-0.688094036796052,43.8701648940774)) ;
#49126 = CARTESIAN_POINT('Origin',(25.05625,-0.565685424949241,44.1656854249492)) ;
#49127 = CARTESIAN_POINT('Origin',(25.05625,-0.565685424949241,44.1656854249492)) ;
#49128 = CARTESIAN_POINT('Origin',(25.028125,-0.282842712474619,44.2828427124746)) ;
#49129 = CARTESIAN_POINT('',(24.8508431715058,-0.0148316913124536,44.3938565123055)) ;
#49130 = CARTESIAN_POINT('',(24.8787539970792,-0.295520530871843,44.2775913881532)) ;
#49131 = CARTESIAN_POINT('Origin',(25.,8.88178419700125E-16,44.4)) ;
#49132 = CARTESIAN_POINT('Origin',(25.,8.88178419700125E-16,44.4)) ;
#49133 = CARTESIAN_POINT('Origin',(24.971875,0.28284271247462,44.2828427124746)) ;
#49134 = CARTESIAN_POINT('',(24.7945931715057,0.550853733636796,44.1718289126438)) ;
#49135 = CARTESIAN_POINT('',(24.8225039970792,0.270164894077396,44.2880940367961)) ;
#49136 = CARTESIAN_POINT('Origin',(24.94375,0.565685424949243,44.1656854249492)) ;
#49137 = CARTESIAN_POINT('Origin',(24.94375,0.565685424949243,44.1656854249492)) ;
#49138 = CARTESIAN_POINT('Origin',(24.915625,0.682842712474619,43.8828427124746)) ;
#49139 = CARTESIAN_POINT('',(24.7383431715058,0.79385651230545,43.6148316913125)) ;
#49140 = CARTESIAN_POINT('',(24.7662539970792,0.677591388153186,43.8955205308718)) ;
#49141 = CARTESIAN_POINT('Origin',(24.8875,0.8,43.6)) ;
#49142 = CARTESIAN_POINT('Origin',(24.8875,0.8,43.6)) ;
#49143 = CARTESIAN_POINT('Origin',(24.859375,0.682842712474619,43.3171572875254)) ;
#49144 = CARTESIAN_POINT('',(24.6820931715058,0.57182891264379,43.0491462663632)) ;
#49145 = CARTESIAN_POINT('',(24.7100039970792,0.688094036796053,43.3298351059226)) ;
#49146 = CARTESIAN_POINT('Origin',(24.83125,0.565685424949238,43.0343145750508)) ;
#49147 = CARTESIAN_POINT('Origin',(24.83125,0.565685424949238,43.0343145750508)) ;
#49148 = CARTESIAN_POINT('Origin',(24.803125,0.282842712474619,42.9171572875254)) ;
#49149 = CARTESIAN_POINT('',(24.6258431715058,0.0148316913124541,42.8061434876946)) ;
#49150 = CARTESIAN_POINT('',(24.6537539970792,0.295520530871843,42.9224086118468)) ;
#49151 = CARTESIAN_POINT('Origin',(24.775,-7.21644966006352E-16,42.8)) ;
#49152 = CARTESIAN_POINT('Origin',(24.775,-7.21644966006352E-16,42.8)) ;
#49153 = CARTESIAN_POINT('Origin',(24.746875,-0.28284271247462,42.9171572875254)) ;
#49154 = CARTESIAN_POINT('',(24.5695931715057,-0.550853733636787,43.0281710873562)) ;
#49155 = CARTESIAN_POINT('',(24.5975039970792,-0.270164894077395,42.9119059632039)) ;
#49156 = CARTESIAN_POINT('Origin',(24.71875,-0.565685424949239,43.0343145750508)) ;
#49157 = CARTESIAN_POINT('Origin',(24.71875,-0.565685424949239,43.0343145750508)) ;
#49158 = CARTESIAN_POINT('Origin',(24.690625,-0.682842712474619,43.3171572875254)) ;
#49159 = CARTESIAN_POINT('',(24.5133431715058,-0.79385651230545,43.5851683086875)) ;
#49160 = CARTESIAN_POINT('',(24.5412539970792,-0.677591388153186,43.3044794691282)) ;
#49161 = CARTESIAN_POINT('Origin',(24.6625,-0.8,43.6)) ;
#49162 = CARTESIAN_POINT('Origin',(24.6625,-0.8,43.6)) ;
#49163 = CARTESIAN_POINT('Origin',(24.634375,-0.682842712474619,43.8828427124746)) ;
#49164 = CARTESIAN_POINT('',(24.4570931715058,-0.57182891264379,44.1508537336368)) ;
#49165 = CARTESIAN_POINT('',(24.4850039970792,-0.688094036796052,43.8701648940774)) ;
#49166 = CARTESIAN_POINT('Origin',(24.60625,-0.565685424949241,44.1656854249492)) ;
#49167 = CARTESIAN_POINT('Origin',(24.60625,-0.565685424949241,44.1656854249492)) ;
#49168 = CARTESIAN_POINT('Origin',(24.578125,-0.282842712474619,44.2828427124746)) ;
#49169 = CARTESIAN_POINT('',(24.4008431715058,-0.0148316913124548,44.3938565123055)) ;
#49170 = CARTESIAN_POINT('',(24.4287539970792,-0.295520530871844,44.2775913881532)) ;
#49171 = CARTESIAN_POINT('Origin',(24.55,5.55111512312578E-17,44.4)) ;
#49172 = CARTESIAN_POINT('Origin',(24.55,5.55111512312578E-17,44.4)) ;
#49173 = CARTESIAN_POINT('Origin',(24.521875,0.28284271247462,44.2828427124746)) ;
#49174 = CARTESIAN_POINT('',(24.3445931715058,0.550853733636791,44.1718289126438)) ;
#49175 = CARTESIAN_POINT('',(24.3725039970792,0.270164894077396,44.2880940367961)) ;
#49176 = CARTESIAN_POINT('Origin',(24.49375,0.565685424949243,44.1656854249492)) ;
#49177 = CARTESIAN_POINT('Origin',(24.49375,0.565685424949243,44.1656854249492)) ;
#49178 = CARTESIAN_POINT('Origin',(24.465625,0.682842712474619,43.8828427124746)) ;
#49179 = CARTESIAN_POINT('',(24.2883431715058,0.793856512305449,43.6148316913125)) ;
#49180 = CARTESIAN_POINT('',(24.3162539970792,0.677591388153186,43.8955205308718)) ;
#49181 = CARTESIAN_POINT('Origin',(24.4375,0.8,43.6)) ;
#49182 = CARTESIAN_POINT('Origin',(24.4375,0.8,43.6)) ;
#49183 = CARTESIAN_POINT('Origin',(24.409375,0.682842712474619,43.3171572875254)) ;
#49184 = CARTESIAN_POINT('',(24.2320931715057,0.571828912643786,43.0491462663632)) ;
#49185 = CARTESIAN_POINT('',(24.2600039970792,0.688094036796052,43.3298351059226)) ;
#49186 = CARTESIAN_POINT('Origin',(24.38125,0.565685424949238,43.0343145750508)) ;
#49187 = CARTESIAN_POINT('Origin',(24.38125,0.565685424949238,43.0343145750508)) ;
#49188 = CARTESIAN_POINT('Origin',(24.353125,0.282842712474619,42.9171572875254)) ;
#49189 = CARTESIAN_POINT('',(24.1758431715058,0.0148316913124543,42.8061434876946)) ;
#49190 = CARTESIAN_POINT('',(24.2037539970792,0.295520530871843,42.9224086118468)) ;
#49191 = CARTESIAN_POINT('Origin',(24.325,-2.77555756156289E-16,42.8)) ;
#49192 = CARTESIAN_POINT('Origin',(24.325,-2.77555756156289E-16,42.8)) ;
#49193 = CARTESIAN_POINT('Origin',(24.296875,-0.28284271247462,42.9171572875254)) ;
#49194 = CARTESIAN_POINT('',(24.1195931715057,-0.550853733636786,43.0281710873562)) ;
#49195 = CARTESIAN_POINT('',(24.1475039970792,-0.270164894077395,42.9119059632039)) ;
#49196 = CARTESIAN_POINT('Origin',(24.26875,-0.565685424949238,43.0343145750508)) ;
#49197 = CARTESIAN_POINT('Origin',(24.26875,-0.565685424949238,43.0343145750508)) ;
#49198 = CARTESIAN_POINT('Origin',(24.240625,-0.682842712474619,43.3171572875254)) ;
#49199 = CARTESIAN_POINT('',(24.0633431715058,-0.79385651230545,43.5851683086875)) ;
#49200 = CARTESIAN_POINT('',(24.0912539970792,-0.677591388153186,43.3044794691282)) ;
#49201 = CARTESIAN_POINT('Origin',(24.2125,-0.8,43.6)) ;
#49202 = CARTESIAN_POINT('Origin',(24.2125,-0.8,43.6)) ;
#49203 = CARTESIAN_POINT('Origin',(24.184375,-0.682842712474619,43.8828427124746)) ;
#49204 = CARTESIAN_POINT('',(24.0070931715058,-0.571828912643794,44.1508537336368)) ;
#49205 = CARTESIAN_POINT('',(24.0350039970792,-0.688094036796053,43.8701648940774)) ;
#49206 = CARTESIAN_POINT('Origin',(24.15625,-0.565685424949241,44.1656854249492)) ;
#49207 = CARTESIAN_POINT('Origin',(24.15625,-0.565685424949241,44.1656854249492)) ;
#49208 = CARTESIAN_POINT('Origin',(24.128125,-0.282842712474619,44.2828427124746)) ;
#49209 = CARTESIAN_POINT('',(23.9508431715058,-0.0148316913124537,44.3938565123055)) ;
#49210 = CARTESIAN_POINT('',(23.9787539970792,-0.295520530871843,44.2775913881532)) ;
#49211 = CARTESIAN_POINT('Origin',(24.1,3.33066907387547E-16,44.4)) ;
#49212 = CARTESIAN_POINT('Origin',(24.1,3.33066907387547E-16,44.4)) ;
#49213 = CARTESIAN_POINT('Origin',(24.071875,0.28284271247462,44.2828427124746)) ;
#49214 = CARTESIAN_POINT('',(23.8945931715058,0.550853733636791,44.1718289126438)) ;
#49215 = CARTESIAN_POINT('',(23.9225039970792,0.270164894077396,44.2880940367961)) ;
#49216 = CARTESIAN_POINT('Origin',(24.04375,0.565685424949242,44.1656854249492)) ;
#49217 = CARTESIAN_POINT('Origin',(24.04375,0.565685424949242,44.1656854249492)) ;
#49218 = CARTESIAN_POINT('Origin',(24.015625,0.682842712474619,43.8828427124746)) ;
#49219 = CARTESIAN_POINT('',(23.8383431715058,0.79385651230545,43.6148316913125)) ;
#49220 = CARTESIAN_POINT('',(23.8662539970792,0.677591388153186,43.8955205308718)) ;
#49221 = CARTESIAN_POINT('Origin',(23.9875,0.8,43.6)) ;
#49222 = CARTESIAN_POINT('Origin',(23.9875,0.8,43.6)) ;
#49223 = CARTESIAN_POINT('Origin',(23.959375,0.682842712474619,43.3171572875254)) ;
#49224 = CARTESIAN_POINT('',(23.7820931715057,0.571828912643788,43.0491462663632)) ;
#49225 = CARTESIAN_POINT('',(23.8100039970792,0.688094036796053,43.3298351059226)) ;
#49226 = CARTESIAN_POINT('Origin',(23.93125,0.565685424949238,43.0343145750508)) ;
#49227 = CARTESIAN_POINT('Origin',(23.93125,0.565685424949238,43.0343145750508)) ;
#49228 = CARTESIAN_POINT('Origin',(23.903125,0.282842712474619,42.9171572875254)) ;
#49229 = CARTESIAN_POINT('',(23.7258431715058,0.0148316913124538,42.8061434876946)) ;
#49230 = CARTESIAN_POINT('',(23.7537539970792,0.295520530871844,42.9224086118468)) ;
#49231 = CARTESIAN_POINT('Origin',(23.875,-6.66133814775094E-16,42.8)) ;
#49232 = CARTESIAN_POINT('Origin',(23.875,-6.66133814775094E-16,42.8)) ;
#49233 = CARTESIAN_POINT('Origin',(23.846875,-0.28284271247462,42.9171572875254)) ;
#49234 = CARTESIAN_POINT('',(23.6695931715057,-0.550853733636787,43.0281710873562)) ;
#49235 = CARTESIAN_POINT('',(23.6975039970792,-0.270164894077395,42.9119059632039)) ;
#49236 = CARTESIAN_POINT('Origin',(23.81875,-0.565685424949239,43.0343145750508)) ;
#49237 = CARTESIAN_POINT('Origin',(23.81875,-0.565685424949239,43.0343145750508)) ;
#49238 = CARTESIAN_POINT('Origin',(23.790625,-0.682842712474619,43.3171572875254)) ;
#49239 = CARTESIAN_POINT('',(23.6133431715058,-0.79385651230545,43.5851683086875)) ;
#49240 = CARTESIAN_POINT('',(23.6412539970792,-0.677591388153186,43.3044794691282)) ;
#49241 = CARTESIAN_POINT('Origin',(23.7625,-0.8,43.6)) ;
#49242 = CARTESIAN_POINT('Origin',(23.7625,-0.8,43.6)) ;
#49243 = CARTESIAN_POINT('Origin',(23.734375,-0.682842712474619,43.8828427124746)) ;
#49244 = CARTESIAN_POINT('',(23.5570931715058,-0.571828912643793,44.1508537336368)) ;
#49245 = CARTESIAN_POINT('',(23.5850039970792,-0.688094036796053,43.8701648940774)) ;
#49246 = CARTESIAN_POINT('Origin',(23.70625,-0.565685424949241,44.1656854249492)) ;
#49247 = CARTESIAN_POINT('Origin',(23.70625,-0.565685424949241,44.1656854249492)) ;
#49248 = CARTESIAN_POINT('Origin',(23.678125,-0.282842712474619,44.2828427124746)) ;
#49249 = CARTESIAN_POINT('',(23.5008431715058,-0.0148316913124547,44.3938565123055)) ;
#49250 = CARTESIAN_POINT('',(23.5287539970792,-0.295520530871843,44.2775913881532)) ;
#49251 = CARTESIAN_POINT('Origin',(23.65,1.66533453693773E-16,44.4)) ;
#49252 = CARTESIAN_POINT('Origin',(23.65,1.66533453693773E-16,44.4)) ;
#49253 = CARTESIAN_POINT('Origin',(23.621875,0.282842712474619,44.2828427124746)) ;
#49254 = CARTESIAN_POINT('',(23.4445931715057,0.550853733636794,44.1718289126438)) ;
#49255 = CARTESIAN_POINT('',(23.4725039970792,0.270164894077394,44.2880940367961)) ;
#49256 = CARTESIAN_POINT('Origin',(23.59375,0.565685424949242,44.1656854249492)) ;
#49257 = CARTESIAN_POINT('Origin',(23.59375,0.565685424949242,44.1656854249492)) ;
#49258 = CARTESIAN_POINT('Origin',(23.565625,0.682842712474619,43.8828427124746)) ;
#49259 = CARTESIAN_POINT('',(23.3883431715058,0.79385651230545,43.6148316913125)) ;
#49260 = CARTESIAN_POINT('',(23.4162539970792,0.677591388153186,43.8955205308718)) ;
#49261 = CARTESIAN_POINT('Origin',(23.5375,0.8,43.6)) ;
#49262 = CARTESIAN_POINT('Origin',(23.5375,0.8,43.6)) ;
#49263 = CARTESIAN_POINT('Origin',(23.509375,0.682842712474619,43.3171572875254)) ;
#49264 = CARTESIAN_POINT('',(23.3320931715058,0.571828912643787,43.0491462663632)) ;
#49265 = CARTESIAN_POINT('',(23.3600039970792,0.688094036796052,43.3298351059226)) ;
#49266 = CARTESIAN_POINT('Origin',(23.48125,0.565685424949238,43.0343145750508)) ;
#49267 = CARTESIAN_POINT('Origin',(23.48125,0.565685424949238,43.0343145750508)) ;
#49268 = CARTESIAN_POINT('Origin',(23.453125,0.282842712474619,42.9171572875254)) ;
#49269 = CARTESIAN_POINT('',(23.2758431715058,0.0148316913124553,42.8061434876946)) ;
#49270 = CARTESIAN_POINT('',(23.3037539970792,0.295520530871844,42.9224086118468)) ;
#49271 = CARTESIAN_POINT('Origin',(23.425,4.9960036108132E-16,42.8)) ;
#49272 = CARTESIAN_POINT('Origin',(23.425,4.9960036108132E-16,42.8)) ;
#49273 = CARTESIAN_POINT('Origin',(23.396875,-0.282842712474619,42.9171572875254)) ;
#49274 = CARTESIAN_POINT('',(23.2195931715058,-0.550853733636782,43.0281710873562)) ;
#49275 = CARTESIAN_POINT('',(23.2475039970792,-0.270164894077395,42.9119059632039)) ;
#49276 = CARTESIAN_POINT('Origin',(23.36875,-0.565685424949238,43.0343145750508)) ;
#49277 = CARTESIAN_POINT('Origin',(23.36875,-0.565685424949238,43.0343145750508)) ;
#49278 = CARTESIAN_POINT('Origin',(23.340625,-0.682842712474619,43.3171572875254)) ;
#49279 = CARTESIAN_POINT('',(23.1633431715058,-0.793856512305449,43.5851683086875)) ;
#49280 = CARTESIAN_POINT('',(23.1912539970792,-0.677591388153185,43.3044794691282)) ;
#49281 = CARTESIAN_POINT('Origin',(23.3125,-0.8,43.6)) ;
#49282 = CARTESIAN_POINT('Origin',(23.3125,-0.8,43.6)) ;
#49283 = CARTESIAN_POINT('Origin',(23.284375,-0.682842712474619,43.8828427124746)) ;
#49284 = CARTESIAN_POINT('',(23.1070931715057,-0.57182891264379,44.1508537336368)) ;
#49285 = CARTESIAN_POINT('',(23.1350039970792,-0.688094036796052,43.8701648940774)) ;
#49286 = CARTESIAN_POINT('Origin',(23.25625,-0.565685424949241,44.1656854249492)) ;
#49287 = CARTESIAN_POINT('Origin',(23.25625,-0.565685424949241,44.1656854249492)) ;
#49288 = CARTESIAN_POINT('Origin',(23.228125,-0.282842712474619,44.2828427124746)) ;
#49289 = CARTESIAN_POINT('',(23.0506289970792,-0.0126778183972212,44.3947486756786)) ;
#49290 = CARTESIAN_POINT('',(23.0787539970792,-0.295520530871843,44.2775913881532)) ;
#49291 = CARTESIAN_POINT('Origin',(23.2,0.,44.4)) ;
#49292 = CARTESIAN_POINT('Origin',(23.2,0.,44.4)) ;
#49293 = CARTESIAN_POINT('Origin',(31.9,0.,43.2)) ;
#49294 = CARTESIAN_POINT('',(31.35,-6.73555739531044E-17,43.6)) ;
#49295 = CARTESIAN_POINT('Origin',(31.9,0.,43.6)) ;
#49296 = CARTESIAN_POINT('',(31.35,-5.36271069502855E-17,43.4747805496751)) ;
#49297 = CARTESIAN_POINT('',(31.35,-6.73555739531044E-17,43.2)) ;
#49298 = CARTESIAN_POINT('',(31.35,-1.6551677115079E-16,43.1585527836583)) ;
#49299 = CARTESIAN_POINT('Ctrl Pts',(31.35,-2.63677968348475E-16,43.1585527836583)) ;
#49300 = CARTESIAN_POINT('Ctrl Pts',(31.35,-0.0188191332662162,43.1585527836583)) ;
#49301 = CARTESIAN_POINT('Ctrl Pts',(31.3510631096512,-0.0388916191458831,
43.1621613787556)) ;
#49302 = CARTESIAN_POINT('Ctrl Pts',(31.3549322157784,-0.0757982758665373,
43.1769669116142)) ;
#49303 = CARTESIAN_POINT('Ctrl Pts',(31.3576877759068,-0.0926307743041964,
43.1881811506715)) ;
#49304 = CARTESIAN_POINT('Ctrl Pts',(31.3629682744752,-0.119540791091898,
43.2147010690475)) ;
#49305 = CARTESIAN_POINT('Ctrl Pts',(31.3658184898934,-0.131194409953506,
43.2318737514959)) ;
#49306 = CARTESIAN_POINT('Ctrl Pts',(31.3697883951301,-0.146415562473201,
43.2697170608075)) ;
#49307 = CARTESIAN_POINT('Ctrl Pts',(31.3708497377871,-0.15,43.2903869851339)) ;
#49308 = CARTESIAN_POINT('Ctrl Pts',(31.3708497377871,-0.15,43.3299223679419)) ;
#49309 = CARTESIAN_POINT('Ctrl Pts',(31.3697109017808,-0.146136718812717,
43.3514677287737)) ;
#49310 = CARTESIAN_POINT('Ctrl Pts',(31.3657306796926,-0.130838683604474,
43.3915453490939)) ;
#49311 = CARTESIAN_POINT('Ctrl Pts',(31.3629471493545,-0.1194120242323,43.4100864224367)) ;
#49312 = CARTESIAN_POINT('Ctrl Pts',(31.3577971876893,-0.093208439870651,
43.4394240794729)) ;
#49313 = CARTESIAN_POINT('Ctrl Pts',(31.3550634167387,-0.0767307277487665,
43.4524660649886)) ;
#49314 = CARTESIAN_POINT('Ctrl Pts',(31.3511342241156,-0.0398728705117728,
43.47016523252)) ;
#49315 = CARTESIAN_POINT('Ctrl Pts',(31.35,-0.0194661400469685,43.4747805496751)) ;
#49316 = CARTESIAN_POINT('Ctrl Pts',(31.35,-6.27969898303604E-16,43.4747805496751)) ;
#49317 = CARTESIAN_POINT('',(31.35,-6.73555739531044E-17,42.8)) ;
#49318 = CARTESIAN_POINT('',(31.35,-6.73555739531044E-17,43.2)) ;
#49319 = CARTESIAN_POINT('Origin',(31.9,0.,42.8)) ;
#49320 = CARTESIAN_POINT('',(31.3708497377871,0.15,43.309716754071)) ;
#49321 = CARTESIAN_POINT('Ctrl Pts',(31.3708497377871,0.15,43.309716754071)) ;
#49322 = CARTESIAN_POINT('Ctrl Pts',(31.3708497377871,0.15,43.2903869851339)) ;
#49323 = CARTESIAN_POINT('Ctrl Pts',(31.3697883951301,0.146415562473201,43.2697170608075)) ;
#49324 = CARTESIAN_POINT('Ctrl Pts',(31.3658184898934,0.131194409953506,43.2318737514959)) ;
#49325 = CARTESIAN_POINT('Ctrl Pts',(31.3629682744752,0.119540791091898,43.2147010690475)) ;
#49326 = CARTESIAN_POINT('Ctrl Pts',(31.3576877759068,0.0926307743041964,
43.1881811506715)) ;
#49327 = CARTESIAN_POINT('Ctrl Pts',(31.3549322157784,0.0757982758665373,
43.1769669116142)) ;
#49328 = CARTESIAN_POINT('Ctrl Pts',(31.3510631096512,0.0388916191458832,
43.1621613787556)) ;
#49329 = CARTESIAN_POINT('Ctrl Pts',(31.35,0.0188191332662163,43.1585527836583)) ;
#49330 = CARTESIAN_POINT('Ctrl Pts',(31.35,3.88578058618805E-16,43.1585527836583)) ;
#49331 = CARTESIAN_POINT('Ctrl Pts',(31.35,-3.98986399474666E-17,43.4747805496751)) ;
#49332 = CARTESIAN_POINT('Ctrl Pts',(31.35,0.0194661400469678,43.4747805496751)) ;
#49333 = CARTESIAN_POINT('Ctrl Pts',(31.3511342241156,0.0398728705117756,
43.47016523252)) ;
#49334 = CARTESIAN_POINT('Ctrl Pts',(31.3550634167387,0.0767307277487687,
43.4524660649886)) ;
#49335 = CARTESIAN_POINT('Ctrl Pts',(31.3577971876893,0.0932084398706509,
43.4394240794729)) ;
#49336 = CARTESIAN_POINT('Ctrl Pts',(31.3629471493545,0.1194120242323,43.4100864224367)) ;
#49337 = CARTESIAN_POINT('Ctrl Pts',(31.3657306796926,0.130838683604474,43.3915453490939)) ;
#49338 = CARTESIAN_POINT('Ctrl Pts',(31.3697109017808,0.146136718812717,43.3514677287737)) ;
#49339 = CARTESIAN_POINT('Ctrl Pts',(31.3708497377871,0.15,43.3299223679419)) ;
#49340 = CARTESIAN_POINT('Ctrl Pts',(31.3708497377871,0.15,43.309716754071)) ;
#49341 = CARTESIAN_POINT('Origin',(31.9,0.,43.2)) ;
#49342 = CARTESIAN_POINT('',(31.65,-3.06161699786838E-17,42.8)) ;
#49343 = CARTESIAN_POINT('Origin',(31.9,0.,42.8)) ;
#49344 = CARTESIAN_POINT('',(31.65,3.06161699786838E-17,43.6)) ;
#49345 = CARTESIAN_POINT('',(31.65,-3.06161699786838E-17,43.2)) ;
#49346 = CARTESIAN_POINT('Origin',(31.9,0.,43.6)) ;
#49347 = CARTESIAN_POINT('Origin',(31.9,0.,42.8)) ;
#49348 = CARTESIAN_POINT('Origin',(31.9,0.,43.6)) ;
#49349 = CARTESIAN_POINT('Origin',(30.95,0.,43.45)) ;
#49350 = CARTESIAN_POINT('',(30.4525658350975,1.83697019872103E-17,43.4576975052924)) ;
#49351 = CARTESIAN_POINT('',(30.9025658350975,1.83697019872103E-17,43.3076975052924)) ;
#49352 = CARTESIAN_POINT('Origin',(30.5,0.,43.6)) ;
#49353 = CARTESIAN_POINT('Origin',(30.5,0.,43.6)) ;
#49354 = CARTESIAN_POINT('',(0.,0.,0.)) ;
#49355 = CARTESIAN_POINT('',(0.,0.,0.)) ;
#49356 = CARTESIAN_POINT('',(0.,0.,0.)) ;
#49357 = CARTESIAN_POINT('',(0.,0.,0.)) ;
#49358 = CARTESIAN_POINT('',(0.,0.,0.)) ;
#49359 = CARTESIAN_POINT('',(0.,0.,0.)) ;
#49360 = CARTESIAN_POINT('',(0.,0.,0.)) ;
#49361 = CARTESIAN_POINT('',(0.,0.,0.)) ;
#49362 = CARTESIAN_POINT('',(0.,0.,0.)) ;
#49363 = CARTESIAN_POINT('',(0.,0.,0.)) ;
#49364 = CARTESIAN_POINT('',(0.,0.,0.)) ;
#49365 = CARTESIAN_POINT('',(0.,0.,0.)) ;
#49366 = CARTESIAN_POINT('',(0.,0.,0.)) ;
#49367 = CARTESIAN_POINT('',(0.,0.,0.)) ;
#49368 = CARTESIAN_POINT('',(0.,0.,0.)) ;
#49369 = CARTESIAN_POINT('',(0.,0.,0.)) ;
#49370 = CARTESIAN_POINT('Origin',(0.,0.,15.)) ;
#49371 = CARTESIAN_POINT('',(-2.02066721859313E-16,-2.47460364139207E-32,
11.7)) ;
#49372 = CARTESIAN_POINT('',(-2.02066721859313E-16,-2.47460364139207E-32,
18.3)) ;
#49373 = CARTESIAN_POINT('Origin',(0.,0.,15.)) ;
#49374 = CARTESIAN_POINT('Origin',(0.,0.,15.)) ;
#49375 = CARTESIAN_POINT('',(1.24135277324074,-3.05762052785618,16.1661903789691)) ;
#49376 = CARTESIAN_POINT('',(1.24135277324074,3.05762052785618,16.1661903789691)) ;
#49377 = CARTESIAN_POINT('Origin',(1.16391931473201,0.,14.9272550428293)) ;
#49378 = CARTESIAN_POINT('Origin',(0.,0.,16.1661903789691)) ;
#49379 = CARTESIAN_POINT('Origin',(0.,0.,20.3)) ;
#49380 = CARTESIAN_POINT('Origin',(-7.105427357601E-15,0.,15.)) ;
#49381 = CARTESIAN_POINT('Origin',(32.,0.,13.)) ;
#49382 = CARTESIAN_POINT('Origin',(0.,0.,25.6)) ;
#49383 = CARTESIAN_POINT('',(-3.5,4.28626379701574E-16,25.6)) ;
#49384 = CARTESIAN_POINT('Origin',(0.,0.,25.6)) ;
#49385 = CARTESIAN_POINT('',(-3.3,4.04133443718627E-16,25.6)) ;
#49386 = CARTESIAN_POINT('Origin',(0.,0.,25.6)) ;
#49387 = CARTESIAN_POINT('Origin',(0.,0.,20.3)) ;
#49388 = CARTESIAN_POINT('',(1.16846587455518,3.2991949775665,15.)) ;
#49389 = CARTESIAN_POINT('',(1.16846587455518,-3.2991949775665,15.)) ;
#49390 = CARTESIAN_POINT('Ctrl Pts',(1.16846587455518,3.2991949775665,15.)) ;
#49391 = CARTESIAN_POINT('Ctrl Pts',(1.17442519254118,3.29708438399758,15.095349087776)) ;
#49392 = CARTESIAN_POINT('Ctrl Pts',(1.19175023527009,3.29096616123353,15.1857170921028)) ;
#49393 = CARTESIAN_POINT('Ctrl Pts',(1.24866258002262,3.26985933817832,15.3815376197941)) ;
#49394 = CARTESIAN_POINT('Ctrl Pts',(1.29262895141202,3.25303416693559,15.4850971713711)) ;
#49395 = CARTESIAN_POINT('Ctrl Pts',(1.44734056737426,3.18868022291068,15.7871365053987)) ;
#49396 = CARTESIAN_POINT('Ctrl Pts',(1.57974867435124,3.12746840533713,15.9770140205015)) ;
#49397 = CARTESIAN_POINT('Ctrl Pts',(1.86407692726612,2.96679654013783,16.3464498247156)) ;
#49398 = CARTESIAN_POINT('Ctrl Pts',(2.01576973425023,2.86748054151594,16.5241537838072)) ;
#49399 = CARTESIAN_POINT('Ctrl Pts',(2.3130389850849,2.63355709436769,16.8591337253863)) ;
#49400 = CARTESIAN_POINT('Ctrl Pts',(2.45876907363751,2.49887177450341,17.0162189313947)) ;
#49401 = CARTESIAN_POINT('Ctrl Pts',(2.71598418768332,2.2151714704621,17.2886907349084)) ;
#49402 = CARTESIAN_POINT('Ctrl Pts',(2.83748562910909,2.05938117281354,17.4149058836929)) ;
#49403 = CARTESIAN_POINT('Ctrl Pts',(3.05933295429687,1.71255872522277,17.6430565099933)) ;
#49404 = CARTESIAN_POINT('Ctrl Pts',(3.15964506633327,1.52149772138736,17.744980961747)) ;
#49405 = CARTESIAN_POINT('Ctrl Pts',(3.32517088360158,1.11424924967644,17.9123789095648)) ;
#49406 = CARTESIAN_POINT('Ctrl Pts',(3.39053849186878,0.897553052697191,17.978012051174)) ;
#49407 = CARTESIAN_POINT('Ctrl Pts',(3.47797144791113,0.452843632408543,18.0656854316297)) ;
#49408 = CARTESIAN_POINT('Ctrl Pts',(3.5,0.224815952965719,18.087689030513)) ;
#49409 = CARTESIAN_POINT('Ctrl Pts',(3.5,-0.224815952965717,18.087689030513)) ;
#49410 = CARTESIAN_POINT('Ctrl Pts',(3.47797144791113,-0.452843632408542,
18.0656854316297)) ;
#49411 = CARTESIAN_POINT('Ctrl Pts',(3.39053849186878,-0.89755305269719,17.978012051174)) ;
#49412 = CARTESIAN_POINT('Ctrl Pts',(3.32517088360158,-1.11424924967644,17.9123789095648)) ;
#49413 = CARTESIAN_POINT('Ctrl Pts',(3.15964506633327,-1.52149772138736,17.744980961747)) ;
#49414 = CARTESIAN_POINT('Ctrl Pts',(3.05933295429687,-1.71255872522277,17.6430565099933)) ;
#49415 = CARTESIAN_POINT('Ctrl Pts',(2.83748562910909,-2.05938117281353,17.4149058836929)) ;
#49416 = CARTESIAN_POINT('Ctrl Pts',(2.71598418768332,-2.2151714704621,17.2886907349084)) ;
#49417 = CARTESIAN_POINT('Ctrl Pts',(2.45876907363751,-2.49887177450341,17.0162189313947)) ;
#49418 = CARTESIAN_POINT('Ctrl Pts',(2.31303898508491,-2.63355709436768,16.8591337253863)) ;
#49419 = CARTESIAN_POINT('Ctrl Pts',(2.01576973425023,-2.86748054151594,16.5241537838072)) ;
#49420 = CARTESIAN_POINT('Ctrl Pts',(1.86407692726612,-2.96679654013782,16.3464498247156)) ;
#49421 = CARTESIAN_POINT('Ctrl Pts',(1.57974867435124,-3.12746840533713,15.9770140205015)) ;
#49422 = CARTESIAN_POINT('Ctrl Pts',(1.44734056737426,-3.18868022291068,15.7871365053987)) ;
#49423 = CARTESIAN_POINT('Ctrl Pts',(1.29262895141202,-3.25303416693559,15.4850971713711)) ;
#49424 = CARTESIAN_POINT('Ctrl Pts',(1.24866258002262,-3.26985933817832,15.3815376197941)) ;
#49425 = CARTESIAN_POINT('Ctrl Pts',(1.19175023527009,-3.29096616123353,15.1857170921028)) ;
#49426 = CARTESIAN_POINT('Ctrl Pts',(1.17442519254118,-3.29708438399758,15.095349087776)) ;
#49427 = CARTESIAN_POINT('Ctrl Pts',(1.16846587455518,-3.2991949775665,15.)) ;
#49428 = CARTESIAN_POINT('Origin',(0.,0.,15.)) ;
#49429 = CARTESIAN_POINT('Origin',(0.,0.,20.3)) ;
#49430 = CARTESIAN_POINT('',(-7.13318293321663E-15,-3.5,15.)) ;
#49431 = CARTESIAN_POINT('',(-7.13318293321663E-15,3.5,15.)) ;
#49432 = CARTESIAN_POINT('Origin',(-7.105427357601E-15,0.,15.)) ;
#49433 = CARTESIAN_POINT('',(-3.5,4.28626379701574E-16,15.)) ;
#49434 = CARTESIAN_POINT('Origin',(0.,0.,15.)) ;
#49435 = CARTESIAN_POINT('',(-3.5,4.28626379701574E-16,20.3)) ;
#49436 = CARTESIAN_POINT('Origin',(0.,0.,15.)) ;
#49437 = CARTESIAN_POINT('Origin',(64.,0.,11.)) ;
#49438 = CARTESIAN_POINT('',(63.7816759984569,4.28626379701574E-16,7.50681597530989)) ;
#49439 = CARTESIAN_POINT('Origin',(64.,0.,11.)) ;
#49440 = CARTESIAN_POINT('',(63.7941516556879,-4.04133443718627E-16,7.70642649100647)) ;
#49441 = CARTESIAN_POINT('Origin',(64.,0.,11.)) ;
#49442 = CARTESIAN_POINT('Origin',(32.,0.,13.)) ;
#49443 = CARTESIAN_POINT('',(0.0728868986855592,3.2991949775665,16.1661903789691)) ;
#49444 = CARTESIAN_POINT('',(0.0728868986855592,-3.2991949775665,16.1661903789691)) ;
#49445 = CARTESIAN_POINT('Ctrl Pts',(0.0728868986855593,3.2991949775665,16.1661903789691)) ;
#49446 = CARTESIAN_POINT('Ctrl Pts',(0.168422033639041,3.29708438399758,16.1661903789691)) ;
#49447 = CARTESIAN_POINT('Ctrl Pts',(0.259694759842746,3.29096616123353,16.1778446813038)) ;
#49448 = CARTESIAN_POINT('Ctrl Pts',(0.458684036951621,3.26985933817832,16.2224312448202)) ;
#49449 = CARTESIAN_POINT('Ctrl Pts',(0.564784461325359,3.25303416693559,16.2598521278095)) ;
#49450 = CARTESIAN_POINT('Ctrl Pts',(0.87588624290687,3.18868022291068,16.3954217590338)) ;
#49451 = CARTESIAN_POINT('Ctrl Pts',(1.07365337723744,3.12746840533713,16.5157277776427)) ;
#49452 = CARTESIAN_POINT('Ctrl Pts',(1.46010564333952,2.96679654013783,16.7764575512887)) ;
#49453 = CARTESIAN_POINT('Ctrl Pts',(1.64692587523926,2.86748054151594,16.9167700800254)) ;
#49454 = CARTESIAN_POINT('Ctrl Pts',(1.99979661606603,2.63355709436769,17.1925649476725)) ;
#49455 = CARTESIAN_POINT('Ctrl Pts',(2.16566630412932,2.49887177450341,17.3282125323839)) ;
#49456 = CARTESIAN_POINT('Ctrl Pts',(2.45365212817748,2.2151714704621,17.5679304160533)) ;
#49457 = CARTESIAN_POINT('Ctrl Pts',(2.58720053454703,2.05938117281353,17.6813221582896)) ;
#49458 = CARTESIAN_POINT('Ctrl Pts',(2.82874531134193,1.71255872522277,17.888505808169)) ;
#49459 = CARTESIAN_POINT('Ctrl Pts',(2.93672857085459,1.52149772138736,17.9822646976223)) ;
#49460 = CARTESIAN_POINT('Ctrl Pts',(3.11412574110247,1.11424924967644,18.1370261692616)) ;
#49461 = CARTESIAN_POINT('Ctrl Pts',(3.18370858669324,0.897553052697192,18.1981723963534)) ;
#49462 = CARTESIAN_POINT('Ctrl Pts',(3.27666514807284,0.452843632408543,18.2799661683616)) ;
#49463 = CARTESIAN_POINT('Ctrl Pts',(3.3,0.224815952965718,18.3005792747866)) ;
#49464 = CARTESIAN_POINT('Ctrl Pts',(3.3,-0.224815952965718,18.3005792747866)) ;
#49465 = CARTESIAN_POINT('Ctrl Pts',(3.27666514807284,-0.452843632408543,
18.2799661683616)) ;
#49466 = CARTESIAN_POINT('Ctrl Pts',(3.18370858669324,-0.897553052697191,
18.1981723963534)) ;
#49467 = CARTESIAN_POINT('Ctrl Pts',(3.11412574110247,-1.11424924967644,18.1370261692616)) ;
#49468 = CARTESIAN_POINT('Ctrl Pts',(2.93672857085459,-1.52149772138736,17.9822646976223)) ;
#49469 = CARTESIAN_POINT('Ctrl Pts',(2.82874531134193,-1.71255872522277,17.888505808169)) ;
#49470 = CARTESIAN_POINT('Ctrl Pts',(2.58720053454702,-2.05938117281353,17.6813221582896)) ;
#49471 = CARTESIAN_POINT('Ctrl Pts',(2.45365212817748,-2.2151714704621,17.5679304160533)) ;
#49472 = CARTESIAN_POINT('Ctrl Pts',(2.16566630412932,-2.49887177450341,17.3282125323839)) ;
#49473 = CARTESIAN_POINT('Ctrl Pts',(1.99979661606603,-2.63355709436769,17.1925649476725)) ;
#49474 = CARTESIAN_POINT('Ctrl Pts',(1.64692587523926,-2.86748054151594,16.9167700800254)) ;
#49475 = CARTESIAN_POINT('Ctrl Pts',(1.46010564333952,-2.96679654013783,16.7764575512887)) ;
#49476 = CARTESIAN_POINT('Ctrl Pts',(1.07365337723744,-3.12746840533713,16.5157277776427)) ;
#49477 = CARTESIAN_POINT('Ctrl Pts',(0.87588624290687,-3.18868022291068,16.3954217590338)) ;
#49478 = CARTESIAN_POINT('Ctrl Pts',(0.564784461325359,-3.25303416693559,
16.2598521278095)) ;
#49479 = CARTESIAN_POINT('Ctrl Pts',(0.458684036951621,-3.26985933817832,
16.2224312448202)) ;
#49480 = CARTESIAN_POINT('Ctrl Pts',(0.259694759842746,-3.29096616123353,
16.1778446813038)) ;
#49481 = CARTESIAN_POINT('Ctrl Pts',(0.168422033639041,-3.29708438399758,
16.1661903789691)) ;
#49482 = CARTESIAN_POINT('Ctrl Pts',(0.0728868986855591,-3.2991949775665,
16.1661903789691)) ;
#49483 = CARTESIAN_POINT('Origin',(-7.105427357601E-15,0.,15.)) ;
#49484 = CARTESIAN_POINT('Origin',(32.,0.,13.)) ;
#49485 = CARTESIAN_POINT('',(-0.218324001543145,4.28626379701574E-16,11.5068159753099)) ;
#49486 = CARTESIAN_POINT('',(31.7816759984569,4.28626379701574E-16,9.50681597530989)) ;
#49487 = CARTESIAN_POINT('Origin',(-7.105427357601E-15,0.,15.)) ;
#49488 = CARTESIAN_POINT('Origin',(-7.105427357601E-15,0.,15.)) ;
#49489 = CARTESIAN_POINT('Origin',(32.,0.,13.)) ;
#49490 = CARTESIAN_POINT('',(0.9580709704199,4.04133443718627E-16,11.6336815338357)) ;
#49491 = CARTESIAN_POINT('Origin',(1.16391931473201,0.,14.9272550428293)) ;
#49492 = CARTESIAN_POINT('',(31.7941516556879,4.04133443718627E-16,9.70642649100647)) ;
#49493 = CARTESIAN_POINT('Origin',(1.16391931473201,0.,14.9272550428293)) ;
#49494 = CARTESIAN_POINT('Origin',(0.,0.,20.3)) ;
#49495 = CARTESIAN_POINT('',(-3.3,4.04133443718627E-16,16.1661903789691)) ;
#49496 = CARTESIAN_POINT('',(-3.3,4.04133443718627E-16,20.3)) ;
#49497 = CARTESIAN_POINT('Origin',(0.,0.,16.1661903789691)) ;
#49498 = CARTESIAN_POINT('Origin',(0.,0.,16.1661903789691)) ;
#49499 = CARTESIAN_POINT('Origin',(0.,0.,15.)) ;
#49500 = CARTESIAN_POINT('Origin',(0.,0.,15.)) ;
#49501 = CARTESIAN_POINT('Origin',(0.,0.,15.)) ;
#49502 = CARTESIAN_POINT('',(-2.14313189850787E-16,-2.62457961965825E-32,
18.5)) ;
#49503 = CARTESIAN_POINT('Origin',(0.,0.,15.)) ;
#49504 = CARTESIAN_POINT('',(0.,0.,0.)) ;
#49505 = CARTESIAN_POINT('Origin',(0.,-16.,24.)) ;
#49506 = CARTESIAN_POINT('',(-0.6,-15.,24.)) ;
#49507 = CARTESIAN_POINT('Origin',(0.,-15.,24.)) ;
#49508 = CARTESIAN_POINT('',(-0.6,-17.,24.)) ;
#49509 = CARTESIAN_POINT('',(-0.6,-16.,24.)) ;
#49510 = CARTESIAN_POINT('Origin',(0.,-17.,24.)) ;
#49511 = CARTESIAN_POINT('Origin',(0.,-17.,24.)) ;
#49512 = CARTESIAN_POINT('Origin',(0.,-4.5,24.)) ;
#49513 = CARTESIAN_POINT('',(0.,-4.5,23.2)) ;
#49514 = CARTESIAN_POINT('',(0.,-4.5,24.8)) ;
#49515 = CARTESIAN_POINT('',(0.,-4.5,24.)) ;
#49516 = CARTESIAN_POINT('',(-0.8,-4.5,23.2)) ;
#49517 = CARTESIAN_POINT('',(0.,-4.5,23.2)) ;
#49518 = CARTESIAN_POINT('',(-0.8,-4.5,24.8)) ;
#49519 = CARTESIAN_POINT('',(-0.8,-4.5,24.)) ;
#49520 = CARTESIAN_POINT('',(0.,-4.5,24.8)) ;
#49521 = CARTESIAN_POINT('Origin',(0.,-9.75,24.8)) ;
#49522 = CARTESIAN_POINT('',(0.8,-15.,24.8)) ;
#49523 = CARTESIAN_POINT('',(0.8,-4.5,24.8)) ;
#49524 = CARTESIAN_POINT('',(0.8,-9.75,24.8)) ;
#49525 = CARTESIAN_POINT('',(0.,-4.5,24.8)) ;
#49526 = CARTESIAN_POINT('',(-0.8,-15.,24.8)) ;
#49527 = CARTESIAN_POINT('',(-0.8,-9.75,24.8)) ;
#49528 = CARTESIAN_POINT('',(0.,-15.,24.8)) ;
#49529 = CARTESIAN_POINT('Origin',(0.,-9.75,23.2)) ;
#49530 = CARTESIAN_POINT('',(0.8,-4.5,23.2)) ;
#49531 = CARTESIAN_POINT('',(0.8,-15.,23.2)) ;
#49532 = CARTESIAN_POINT('',(0.8,-9.75,23.2)) ;
#49533 = CARTESIAN_POINT('',(-0.8,-15.,23.2)) ;
#49534 = CARTESIAN_POINT('',(0.,-15.,23.2)) ;
#49535 = CARTESIAN_POINT('',(-0.8,-9.75,23.2)) ;
#49536 = CARTESIAN_POINT('',(0.,-4.5,23.2)) ;
#49537 = CARTESIAN_POINT('Origin',(0.,-15.,24.)) ;
#49538 = CARTESIAN_POINT('',(-0.8,-15.,24.)) ;
#49539 = CARTESIAN_POINT('',(0.8,-15.,24.)) ;
#49540 = CARTESIAN_POINT('Origin',(-0.8,-9.75,24.)) ;
#49541 = CARTESIAN_POINT('Origin',(0.,-4.5,24.)) ;
#49542 = CARTESIAN_POINT('',(0.8,-4.5,24.)) ;
#49543 = CARTESIAN_POINT('Origin',(0.8,-9.75,24.)) ;
#49544 = CARTESIAN_POINT('Origin',(12.,0.,24.)) ;
#49545 = CARTESIAN_POINT('',(12.,-1.22464679914735E-16,25.)) ;
#49546 = CARTESIAN_POINT('Origin',(12.,0.,24.)) ;
#49547 = CARTESIAN_POINT('Origin',(4.5,0.,24.)) ;
#49548 = CARTESIAN_POINT('',(4.5,0.,23.)) ;
#49549 = CARTESIAN_POINT('',(4.5,0.,25.)) ;
#49550 = CARTESIAN_POINT('',(4.5,0.,24.)) ;
#49551 = CARTESIAN_POINT('Origin',(4.5,0.,24.)) ;
#49552 = CARTESIAN_POINT('Origin',(8.25,0.,24.)) ;
#49553 = CARTESIAN_POINT('',(11.82,0.,25.)) ;
#49554 = CARTESIAN_POINT('',(8.25,-1.22464679914735E-16,25.)) ;
#49555 = CARTESIAN_POINT('',(11.18,0.,25.)) ;
#49556 = CARTESIAN_POINT('Ctrl Pts',(11.82,0.,25.)) ;
#49557 = CARTESIAN_POINT('Ctrl Pts',(11.82,-0.0404815515455362,25.)) ;
#49558 = CARTESIAN_POINT('Ctrl Pts',(11.8118517942692,-0.0834711465257763,
24.9972999591064)) ;
#49559 = CARTESIAN_POINT('Ctrl Pts',(11.7791044225004,-0.162233452253763,
24.9875499722835)) ;
#49560 = CARTESIAN_POINT('Ctrl Pts',(11.7545204234507,-0.198027916508675,
24.9806252339521)) ;
#49561 = CARTESIAN_POINT('Ctrl Pts',(11.6980168827738,-0.254531457185612,
24.9674995088223)) ;
#49562 = CARTESIAN_POINT('Ctrl Pts',(11.6622268501742,-0.279106940985719,
24.9604129001751)) ;
#49563 = CARTESIAN_POINT('Ctrl Pts',(11.583480842843,-0.311847989268857,24.9502865189927)) ;
#49564 = CARTESIAN_POINT('Ctrl Pts',(11.540497364712,-0.32,24.9474175425862)) ;
#49565 = CARTESIAN_POINT('Ctrl Pts',(11.5,-0.32,24.9474175425862)) ;
#49566 = CARTESIAN_POINT('Ctrl Pts',(11.459502635288,-0.32,24.9474175425862)) ;
#49567 = CARTESIAN_POINT('Ctrl Pts',(11.416519157157,-0.311847989268857,24.9502865189927)) ;
#49568 = CARTESIAN_POINT('Ctrl Pts',(11.3377731498258,-0.279106940985719,
24.9604129001751)) ;
#49569 = CARTESIAN_POINT('Ctrl Pts',(11.3019831172262,-0.254531457185612,
24.9674995088223)) ;
#49570 = CARTESIAN_POINT('Ctrl Pts',(11.2454795765493,-0.198027916508675,
24.9806252339521)) ;
#49571 = CARTESIAN_POINT('Ctrl Pts',(11.2208955774996,-0.162233452253763,
24.9875499722835)) ;
#49572 = CARTESIAN_POINT('Ctrl Pts',(11.1881482057308,-0.0834711465257753,
24.9972999591064)) ;
#49573 = CARTESIAN_POINT('Ctrl Pts',(11.18,-0.0404815515455361,25.)) ;
#49574 = CARTESIAN_POINT('Ctrl Pts',(11.18,8.32667268468867E-17,25.)) ;
#49575 = CARTESIAN_POINT('',(8.25,-1.22464679914735E-16,25.)) ;
#49576 = CARTESIAN_POINT('Origin',(4.5,0.,24.)) ;
#49577 = CARTESIAN_POINT('Ctrl Pts',(11.18,7.63278329429795E-17,25.)) ;
#49578 = CARTESIAN_POINT('Ctrl Pts',(11.18,0.0404815515455362,25.)) ;
#49579 = CARTESIAN_POINT('Ctrl Pts',(11.1881482057308,0.0834711465257764,
24.9972999591064)) ;
#49580 = CARTESIAN_POINT('Ctrl Pts',(11.2208955774996,0.162233452253763,24.9875499722835)) ;
#49581 = CARTESIAN_POINT('Ctrl Pts',(11.2454795765493,0.198027916508675,24.9806252339521)) ;
#49582 = CARTESIAN_POINT('Ctrl Pts',(11.3019831172262,0.254531457185612,24.9674995088223)) ;
#49583 = CARTESIAN_POINT('Ctrl Pts',(11.3377731498258,0.279106940985719,24.9604129001751)) ;
#49584 = CARTESIAN_POINT('Ctrl Pts',(11.416519157157,0.311847989268857,24.9502865189927)) ;
#49585 = CARTESIAN_POINT('Ctrl Pts',(11.459502635288,0.32,24.9474175425862)) ;
#49586 = CARTESIAN_POINT('Ctrl Pts',(11.540497364712,0.32,24.9474175425862)) ;
#49587 = CARTESIAN_POINT('Ctrl Pts',(11.583480842843,0.311847989268857,24.9502865189927)) ;
#49588 = CARTESIAN_POINT('Ctrl Pts',(11.6622268501742,0.279106940985719,24.9604129001751)) ;
#49589 = CARTESIAN_POINT('Ctrl Pts',(11.6980168827738,0.254531457185612,24.9674995088223)) ;
#49590 = CARTESIAN_POINT('Ctrl Pts',(11.7545204234507,0.198027916508675,24.9806252339521)) ;
#49591 = CARTESIAN_POINT('Ctrl Pts',(11.7791044225004,0.162233452253763,24.9875499722835)) ;
#49592 = CARTESIAN_POINT('Ctrl Pts',(11.8118517942692,0.0834711465257763,
24.9972999591064)) ;
#49593 = CARTESIAN_POINT('Ctrl Pts',(11.82,0.0404815515455362,25.)) ;
#49594 = CARTESIAN_POINT('Ctrl Pts',(11.82,0.,25.)) ;
#49595 = CARTESIAN_POINT('',(11.82,0.,23.)) ;
#49596 = CARTESIAN_POINT('',(11.18,0.,23.)) ;
#49597 = CARTESIAN_POINT('Ctrl Pts',(11.82,-6.93889390390723E-17,23.)) ;
#49598 = CARTESIAN_POINT('Ctrl Pts',(11.82,0.0404815515455361,23.)) ;
#49599 = CARTESIAN_POINT('Ctrl Pts',(11.8118517942692,0.0834711465257763,
23.0027000408936)) ;
#49600 = CARTESIAN_POINT('Ctrl Pts',(11.7791044225004,0.162233452253763,23.0124500277165)) ;
#49601 = CARTESIAN_POINT('Ctrl Pts',(11.7545204234507,0.198027916508675,23.0193747660479)) ;
#49602 = CARTESIAN_POINT('Ctrl Pts',(11.6980168827738,0.254531457185612,23.0325004911777)) ;
#49603 = CARTESIAN_POINT('Ctrl Pts',(11.6622268501742,0.279106940985719,23.0395870998249)) ;
#49604 = CARTESIAN_POINT('Ctrl Pts',(11.583480842843,0.311847989268857,23.0497134810073)) ;
#49605 = CARTESIAN_POINT('Ctrl Pts',(11.540497364712,0.32,23.0525824574138)) ;
#49606 = CARTESIAN_POINT('Ctrl Pts',(11.459502635288,0.32,23.0525824574138)) ;
#49607 = CARTESIAN_POINT('Ctrl Pts',(11.416519157157,0.311847989268857,23.0497134810073)) ;
#49608 = CARTESIAN_POINT('Ctrl Pts',(11.3377731498258,0.279106940985719,23.0395870998249)) ;
#49609 = CARTESIAN_POINT('Ctrl Pts',(11.3019831172262,0.254531457185612,23.0325004911777)) ;
#49610 = CARTESIAN_POINT('Ctrl Pts',(11.2454795765493,0.198027916508675,23.0193747660479)) ;
#49611 = CARTESIAN_POINT('Ctrl Pts',(11.2208955774996,0.162233452253763,23.0124500277165)) ;
#49612 = CARTESIAN_POINT('Ctrl Pts',(11.1881482057308,0.0834711465257763,
23.0027000408936)) ;
#49613 = CARTESIAN_POINT('Ctrl Pts',(11.18,0.0404815515455361,23.)) ;
#49614 = CARTESIAN_POINT('Ctrl Pts',(11.18,0.,23.)) ;
#49615 = CARTESIAN_POINT('Ctrl Pts',(11.18,1.80411241501588E-16,23.)) ;
#49616 = CARTESIAN_POINT('Ctrl Pts',(11.18,-0.040481551545536,23.)) ;
#49617 = CARTESIAN_POINT('Ctrl Pts',(11.1881482057308,-0.0834711465257763,
23.0027000408936)) ;
#49618 = CARTESIAN_POINT('Ctrl Pts',(11.2208955774996,-0.162233452253763,
23.0124500277165)) ;
#49619 = CARTESIAN_POINT('Ctrl Pts',(11.2454795765493,-0.198027916508675,
23.0193747660479)) ;
#49620 = CARTESIAN_POINT('Ctrl Pts',(11.3019831172262,-0.254531457185612,
23.0325004911777)) ;
#49621 = CARTESIAN_POINT('Ctrl Pts',(11.3377731498258,-0.279106940985719,
23.0395870998249)) ;
#49622 = CARTESIAN_POINT('Ctrl Pts',(11.416519157157,-0.311847989268857,23.0497134810073)) ;
#49623 = CARTESIAN_POINT('Ctrl Pts',(11.459502635288,-0.32,23.0525824574138)) ;
#49624 = CARTESIAN_POINT('Ctrl Pts',(11.5,-0.32,23.0525824574138)) ;
#49625 = CARTESIAN_POINT('Ctrl Pts',(11.540497364712,-0.32,23.0525824574138)) ;
#49626 = CARTESIAN_POINT('Ctrl Pts',(11.583480842843,-0.311847989268857,23.0497134810073)) ;
#49627 = CARTESIAN_POINT('Ctrl Pts',(11.6622268501742,-0.279106940985719,
23.0395870998249)) ;
#49628 = CARTESIAN_POINT('Ctrl Pts',(11.6980168827738,-0.254531457185612,
23.0325004911777)) ;
#49629 = CARTESIAN_POINT('Ctrl Pts',(11.7545204234507,-0.198027916508675,
23.0193747660479)) ;
#49630 = CARTESIAN_POINT('Ctrl Pts',(11.7791044225004,-0.162233452253763,
23.0124500277165)) ;
#49631 = CARTESIAN_POINT('Ctrl Pts',(11.8118517942692,-0.0834711465257763,
23.0027000408936)) ;
#49632 = CARTESIAN_POINT('Ctrl Pts',(11.82,-0.0404815515455362,23.)) ;
#49633 = CARTESIAN_POINT('Ctrl Pts',(11.82,-6.93889390390723E-18,23.)) ;
#49634 = CARTESIAN_POINT('Origin',(4.5,0.,24.)) ;
#49635 = CARTESIAN_POINT('Origin',(11.5,0.,24.)) ;
#49636 = CARTESIAN_POINT('',(11.18,-3.91886975727153E-17,24.)) ;
#49637 = CARTESIAN_POINT('Origin',(-11.5,0.,24.)) ;
#49638 = CARTESIAN_POINT('',(-11.18,0.,23.)) ;
#49639 = CARTESIAN_POINT('',(-11.82,0.,23.)) ;
#49640 = CARTESIAN_POINT('Ctrl Pts',(-11.18,-6.24500451351651E-17,23.)) ;
#49641 = CARTESIAN_POINT('Ctrl Pts',(-11.18,0.0404815515455361,23.)) ;
#49642 = CARTESIAN_POINT('Ctrl Pts',(-11.1881482057308,0.0834711465257763,
23.0027000408936)) ;
#49643 = CARTESIAN_POINT('Ctrl Pts',(-11.2208955774996,0.162233452253763,
23.0124500277165)) ;
#49644 = CARTESIAN_POINT('Ctrl Pts',(-11.2454795765493,0.198027916508675,
23.0193747660479)) ;
#49645 = CARTESIAN_POINT('Ctrl Pts',(-11.3019831172262,0.254531457185612,
23.0325004911777)) ;
#49646 = CARTESIAN_POINT('Ctrl Pts',(-11.3377731498258,0.279106940985719,
23.0395870998249)) ;
#49647 = CARTESIAN_POINT('Ctrl Pts',(-11.416519157157,0.311847989268857,23.0497134810073)) ;
#49648 = CARTESIAN_POINT('Ctrl Pts',(-11.459502635288,0.32,23.0525824574138)) ;
#49649 = CARTESIAN_POINT('Ctrl Pts',(-11.540497364712,0.32,23.0525824574138)) ;
#49650 = CARTESIAN_POINT('Ctrl Pts',(-11.583480842843,0.311847989268857,23.0497134810073)) ;
#49651 = CARTESIAN_POINT('Ctrl Pts',(-11.6622268501742,0.279106940985719,
23.0395870998249)) ;
#49652 = CARTESIAN_POINT('Ctrl Pts',(-11.6980168827738,0.254531457185612,
23.0325004911777)) ;
#49653 = CARTESIAN_POINT('Ctrl Pts',(-11.7545204234507,0.198027916508675,
23.0193747660479)) ;
#49654 = CARTESIAN_POINT('Ctrl Pts',(-11.7791044225004,0.162233452253763,
23.0124500277165)) ;
#49655 = CARTESIAN_POINT('Ctrl Pts',(-11.8118517942692,0.0834711465257763,
23.0027000408936)) ;
#49656 = CARTESIAN_POINT('Ctrl Pts',(-11.82,0.0404815515455362,23.)) ;
#49657 = CARTESIAN_POINT('Ctrl Pts',(-11.82,4.16333634234434E-17,23.)) ;
#49658 = CARTESIAN_POINT('Ctrl Pts',(-11.82,2.08166817117217E-17,23.)) ;
#49659 = CARTESIAN_POINT('Ctrl Pts',(-11.82,-0.0404815515455362,23.)) ;
#49660 = CARTESIAN_POINT('Ctrl Pts',(-11.8118517942692,-0.0834711465257763,
23.0027000408936)) ;
#49661 = CARTESIAN_POINT('Ctrl Pts',(-11.7791044225004,-0.162233452253763,
23.0124500277165)) ;
#49662 = CARTESIAN_POINT('Ctrl Pts',(-11.7545204234507,-0.198027916508675,
23.0193747660479)) ;
#49663 = CARTESIAN_POINT('Ctrl Pts',(-11.6980168827738,-0.254531457185612,
23.0325004911777)) ;
#49664 = CARTESIAN_POINT('Ctrl Pts',(-11.6622268501742,-0.279106940985719,
23.0395870998249)) ;
#49665 = CARTESIAN_POINT('Ctrl Pts',(-11.583480842843,-0.311847989268857,
23.0497134810073)) ;
#49666 = CARTESIAN_POINT('Ctrl Pts',(-11.540497364712,-0.32,23.0525824574138)) ;
#49667 = CARTESIAN_POINT('Ctrl Pts',(-11.5,-0.32,23.0525824574138)) ;
#49668 = CARTESIAN_POINT('Ctrl Pts',(-11.459502635288,-0.32,23.0525824574138)) ;
#49669 = CARTESIAN_POINT('Ctrl Pts',(-11.416519157157,-0.311847989268857,
23.0497134810073)) ;
#49670 = CARTESIAN_POINT('Ctrl Pts',(-11.3377731498258,-0.279106940985719,
23.0395870998249)) ;
#49671 = CARTESIAN_POINT('Ctrl Pts',(-11.3019831172262,-0.254531457185612,
23.0325004911777)) ;
#49672 = CARTESIAN_POINT('Ctrl Pts',(-11.2454795765493,-0.198027916508675,
23.0193747660479)) ;
#49673 = CARTESIAN_POINT('Ctrl Pts',(-11.2208955774996,-0.162233452253763,
23.0124500277165)) ;
#49674 = CARTESIAN_POINT('Ctrl Pts',(-11.1881482057308,-0.0834711465257763,
23.0027000408936)) ;
#49675 = CARTESIAN_POINT('Ctrl Pts',(-11.18,-0.040481551545536,23.)) ;
#49676 = CARTESIAN_POINT('Ctrl Pts',(-11.18,1.80411241501588E-16,23.)) ;
#49677 = CARTESIAN_POINT('',(-11.82,0.,25.)) ;
#49678 = CARTESIAN_POINT('',(-11.82,-3.91886975727153E-17,24.)) ;
#49679 = CARTESIAN_POINT('',(-11.18,0.,25.)) ;
#49680 = CARTESIAN_POINT('Ctrl Pts',(-11.18,1.66533453693773E-16,25.)) ;
#49681 = CARTESIAN_POINT('Ctrl Pts',(-11.18,-0.040481551545536,25.)) ;
#49682 = CARTESIAN_POINT('Ctrl Pts',(-11.1881482057308,-0.0834711465257763,
24.9972999591064)) ;
#49683 = CARTESIAN_POINT('Ctrl Pts',(-11.2208955774996,-0.162233452253763,
24.9875499722835)) ;
#49684 = CARTESIAN_POINT('Ctrl Pts',(-11.2454795765493,-0.198027916508675,
24.9806252339521)) ;
#49685 = CARTESIAN_POINT('Ctrl Pts',(-11.3019831172262,-0.254531457185612,
24.9674995088223)) ;
#49686 = CARTESIAN_POINT('Ctrl Pts',(-11.3377731498258,-0.279106940985719,
24.9604129001751)) ;
#49687 = CARTESIAN_POINT('Ctrl Pts',(-11.416519157157,-0.311847989268857,
24.9502865189927)) ;
#49688 = CARTESIAN_POINT('Ctrl Pts',(-11.459502635288,-0.32,24.9474175425862)) ;
#49689 = CARTESIAN_POINT('Ctrl Pts',(-11.5,-0.32,24.9474175425862)) ;
#49690 = CARTESIAN_POINT('Ctrl Pts',(-11.540497364712,-0.32,24.9474175425862)) ;
#49691 = CARTESIAN_POINT('Ctrl Pts',(-11.583480842843,-0.311847989268857,
24.9502865189927)) ;
#49692 = CARTESIAN_POINT('Ctrl Pts',(-11.6622268501742,-0.279106940985719,
24.9604129001751)) ;
#49693 = CARTESIAN_POINT('Ctrl Pts',(-11.6980168827738,-0.254531457185612,
24.9674995088223)) ;
#49694 = CARTESIAN_POINT('Ctrl Pts',(-11.7545204234507,-0.198027916508675,
24.9806252339521)) ;
#49695 = CARTESIAN_POINT('Ctrl Pts',(-11.7791044225004,-0.162233452253764,
24.9875499722835)) ;
#49696 = CARTESIAN_POINT('Ctrl Pts',(-11.8118517942692,-0.0834711465257764,
24.9972999591064)) ;
#49697 = CARTESIAN_POINT('Ctrl Pts',(-11.82,-0.0404815515455361,25.)) ;
#49698 = CARTESIAN_POINT('Ctrl Pts',(-11.82,4.16333634234434E-17,25.)) ;
#49699 = CARTESIAN_POINT('Ctrl Pts',(-11.82,-1.04083408558608E-17,25.)) ;
#49700 = CARTESIAN_POINT('Ctrl Pts',(-11.82,0.0404815515455361,25.)) ;
#49701 = CARTESIAN_POINT('Ctrl Pts',(-11.8118517942692,0.0834711465257764,
24.9972999591064)) ;
#49702 = CARTESIAN_POINT('Ctrl Pts',(-11.7791044225004,0.162233452253763,
24.9875499722835)) ;
#49703 = CARTESIAN_POINT('Ctrl Pts',(-11.7545204234507,0.198027916508675,
24.9806252339521)) ;
#49704 = CARTESIAN_POINT('Ctrl Pts',(-11.6980168827738,0.254531457185612,
24.9674995088223)) ;
#49705 = CARTESIAN_POINT('Ctrl Pts',(-11.6622268501742,0.279106940985719,
24.9604129001751)) ;
#49706 = CARTESIAN_POINT('Ctrl Pts',(-11.583480842843,0.311847989268857,24.9502865189927)) ;
#49707 = CARTESIAN_POINT('Ctrl Pts',(-11.540497364712,0.32,24.9474175425862)) ;
#49708 = CARTESIAN_POINT('Ctrl Pts',(-11.459502635288,0.32,24.9474175425862)) ;
#49709 = CARTESIAN_POINT('Ctrl Pts',(-11.416519157157,0.311847989268857,24.9502865189927)) ;
#49710 = CARTESIAN_POINT('Ctrl Pts',(-11.3377731498258,0.279106940985719,
24.9604129001751)) ;
#49711 = CARTESIAN_POINT('Ctrl Pts',(-11.3019831172262,0.254531457185612,
24.9674995088223)) ;
#49712 = CARTESIAN_POINT('Ctrl Pts',(-11.2454795765493,0.198027916508675,
24.9806252339521)) ;
#49713 = CARTESIAN_POINT('Ctrl Pts',(-11.2208955774996,0.162233452253763,
24.9875499722835)) ;
#49714 = CARTESIAN_POINT('Ctrl Pts',(-11.1881482057308,0.0834711465257763,
24.9972999591064)) ;
#49715 = CARTESIAN_POINT('Ctrl Pts',(-11.18,0.040481551545536,25.)) ;
#49716 = CARTESIAN_POINT('Ctrl Pts',(-11.18,-1.66533453693773E-16,25.)) ;
#49717 = CARTESIAN_POINT('Origin',(-4.5,0.,24.)) ;
#49718 = CARTESIAN_POINT('',(-4.5,0.,23.)) ;
#49719 = CARTESIAN_POINT('',(-4.5,0.,25.)) ;
#49720 = CARTESIAN_POINT('',(-4.5,0.,24.)) ;
#49721 = CARTESIAN_POINT('Origin',(-4.5,0.,24.)) ;
#49722 = CARTESIAN_POINT('Origin',(-8.25,0.,24.)) ;
#49723 = CARTESIAN_POINT('Origin',(-4.5,0.,24.)) ;
#49724 = CARTESIAN_POINT('',(-8.25,-1.22464679914735E-16,25.)) ;
#49725 = CARTESIAN_POINT('',(-12.,-1.22464679914735E-16,25.)) ;
#49726 = CARTESIAN_POINT('',(-8.25,-1.22464679914735E-16,25.)) ;
#49727 = CARTESIAN_POINT('Origin',(-12.,0.,24.)) ;
#49728 = CARTESIAN_POINT('Origin',(-12.,0.,24.)) ;
#49729 = CARTESIAN_POINT('Origin',(-4.5,0.,24.)) ;
#49730 = CARTESIAN_POINT('Origin',(0.,0.,24.)) ;
#49731 = CARTESIAN_POINT('',(0.,-4.5,24.8)) ;
#49732 = CARTESIAN_POINT('',(2.75545529808154E-16,-4.5,25.5)) ;
#49733 = CARTESIAN_POINT('',(2.75545529808154E-16,-4.5,24.)) ;
#49734 = CARTESIAN_POINT('',(0.,-4.5,23.2)) ;
#49735 = CARTESIAN_POINT('',(0.,-4.5,24.)) ;
#49736 = CARTESIAN_POINT('',(2.75545529808154E-16,-4.5,22.5)) ;
#49737 = CARTESIAN_POINT('',(2.75545529808154E-16,-4.5,24.)) ;
#49738 = CARTESIAN_POINT('',(-4.5,-5.51091059616309E-16,22.5)) ;
#49739 = CARTESIAN_POINT('Origin',(0.,0.,22.5)) ;
#49740 = CARTESIAN_POINT('',(-4.5,0.,23.)) ;
#49741 = CARTESIAN_POINT('',(-4.5,-5.51091059616309E-16,24.)) ;
#49742 = CARTESIAN_POINT('',(-4.5,0.,25.)) ;
#49743 = CARTESIAN_POINT('',(-4.5,0.,24.)) ;
#49744 = CARTESIAN_POINT('',(-4.5,-5.51091059616309E-16,25.5)) ;
#49745 = CARTESIAN_POINT('',(-4.5,-5.51091059616309E-16,24.)) ;
#49746 = CARTESIAN_POINT('Origin',(0.,0.,25.5)) ;
#49747 = CARTESIAN_POINT('',(4.5,0.,23.)) ;
#49748 = CARTESIAN_POINT('',(4.5,0.,25.)) ;
#49749 = CARTESIAN_POINT('',(4.5,0.,24.)) ;
#49750 = CARTESIAN_POINT('Origin',(0.,0.,25.5)) ;
#49751 = CARTESIAN_POINT('Origin',(0.,0.,25.5)) ;
#49752 = CARTESIAN_POINT('',(-3.5,4.28626379701574E-16,25.5)) ;
#49753 = CARTESIAN_POINT('Origin',(0.,0.,25.5)) ;
#49754 = CARTESIAN_POINT('Origin',(0.,0.,22.5)) ;
#49755 = CARTESIAN_POINT('Origin',(0.,0.,22.5)) ;
#49756 = CARTESIAN_POINT('',(-3.5,-4.28626379701574E-16,22.5)) ;
#49757 = CARTESIAN_POINT('Origin',(0.,0.,22.5)) ;
#49758 = CARTESIAN_POINT('Origin',(0.,0.,24.)) ;
#49759 = CARTESIAN_POINT('Origin',(0.,0.,24.)) ;
#49760 = CARTESIAN_POINT('',(-3.5,-4.28626379701574E-16,24.)) ;
#49761 = CARTESIAN_POINT('',(0.,0.,0.)) ;
#49762 = CARTESIAN_POINT('Origin',(10.,0.,24.)) ;
#49763 = CARTESIAN_POINT('',(9.5,-1.22464679914735E-16,25.)) ;
#49764 = CARTESIAN_POINT('Origin',(9.5,0.,24.)) ;
#49765 = CARTESIAN_POINT('',(10.5,1.22464679914735E-16,25.)) ;
#49766 = CARTESIAN_POINT('',(10.,-1.22464679914735E-16,25.)) ;
#49767 = CARTESIAN_POINT('Origin',(10.5,0.,24.)) ;
#49768 = CARTESIAN_POINT('Origin',(10.,0.,24.)) ;
#49769 = CARTESIAN_POINT('',(10.5,-1.2491397351303E-16,25.02)) ;
#49770 = CARTESIAN_POINT('Origin',(10.5,0.,24.)) ;
#49771 = CARTESIAN_POINT('',(9.5,-1.2491397351303E-16,25.02)) ;
#49772 = CARTESIAN_POINT('',(10.,-1.2491397351303E-16,25.02)) ;
#49773 = CARTESIAN_POINT('Origin',(9.5,0.,24.)) ;
#49774 = CARTESIAN_POINT('Origin',(9.5,0.,24.)) ;
#49775 = CARTESIAN_POINT('Origin',(10.5,0.,24.)) ;
#49776 = CARTESIAN_POINT('',(0.,0.,0.)) ;
#49777 = CARTESIAN_POINT('Origin',(63.,0.,11.0625)) ;
#49778 = CARTESIAN_POINT('',(64.2183240015431,3.49999336320522,10.9931840246901)) ;
#49779 = CARTESIAN_POINT('',(64.6175450329363,3.49999336320522,10.968232710228)) ;
#49780 = CARTESIAN_POINT('',(63.0004251688583,3.49999336320522,11.0693027017329)) ;
#49781 = CARTESIAN_POINT('',(64.2183240015431,-3.49999336320522,10.9931840246901)) ;
#49782 = CARTESIAN_POINT('Origin',(64.2178988326848,0.,10.9863813229572)) ;
#49783 = CARTESIAN_POINT('',(64.6175450329363,-3.49999336320522,10.968232710228)) ;
#49784 = CARTESIAN_POINT('',(63.0004251688583,-3.49999336320522,11.0693027017329)) ;
#49785 = CARTESIAN_POINT('Origin',(64.617119864078,0.,10.9614300084951)) ;
#49786 = CARTESIAN_POINT('Origin',(64.,0.,7.5)) ;
#49787 = CARTESIAN_POINT('',(64.2183240015431,5.5,10.9931840246901)) ;
#49788 = CARTESIAN_POINT('',(64.2183240015431,0.,10.9931840246901)) ;
#49789 = CARTESIAN_POINT('',(63.7816759984569,5.5,4.00681597530989)) ;
#49790 = CARTESIAN_POINT('',(64.,5.5,7.5)) ;
#49791 = CARTESIAN_POINT('',(63.7816759984569,-5.5,4.00681597530989)) ;
#49792 = CARTESIAN_POINT('',(63.7816759984569,0.,4.00681597530989)) ;
#49793 = CARTESIAN_POINT('',(64.2183240015431,-5.5,10.9931840246901)) ;
#49794 = CARTESIAN_POINT('',(64.,-5.5,7.5)) ;
#49795 = CARTESIAN_POINT('',(64.2183240015431,0.,10.9931840246901)) ;
#49796 = CARTESIAN_POINT('Origin',(64.4179345172397,0.,10.9807083674591)) ;
#49797 = CARTESIAN_POINT('',(64.6175450329363,5.5,10.968232710228)) ;
#49798 = CARTESIAN_POINT('',(64.6175450329363,0.,10.968232710228)) ;
#49799 = CARTESIAN_POINT('',(64.4179345172397,5.5,10.9807083674591)) ;
#49800 = CARTESIAN_POINT('Origin',(64.4179345172397,0.,10.9807083674591)) ;
#49801 = CARTESIAN_POINT('',(64.6175450329363,-5.5,10.968232710228)) ;
#49802 = CARTESIAN_POINT('',(64.4179345172397,-5.5,10.9807083674591)) ;
#49803 = CARTESIAN_POINT('',(64.6175450329363,0.,10.968232710228)) ;
#49804 = CARTESIAN_POINT('Origin',(63.9812865141534,0.,3.99434031807885)) ;
#49805 = CARTESIAN_POINT('',(64.18089702985,5.5,3.98186466084782)) ;
#49806 = CARTESIAN_POINT('',(64.18089702985,-5.5,3.98186466084782)) ;
#49807 = CARTESIAN_POINT('',(64.18089702985,0.,3.98186466084782)) ;
#49808 = CARTESIAN_POINT('',(63.9812865141534,-5.5,3.99434031807885)) ;
#49809 = CARTESIAN_POINT('',(63.9812865141534,5.5,3.99434031807885)) ;
#49810 = CARTESIAN_POINT('Origin',(64.1996105156966,-5.5,7.48752434276896)) ;
#49811 = CARTESIAN_POINT('',(64.3992210313932,-5.5,7.47504868553793)) ;
#49812 = CARTESIAN_POINT('Origin',(64.1996105156966,5.5,7.48752434276896)) ;
#49813 = CARTESIAN_POINT('',(64.3992210313932,5.5,7.47504868553793)) ;
#49814 = CARTESIAN_POINT('Origin',(64.3992210313932,0.,7.47504868553793)) ;
#49815 = CARTESIAN_POINT('Origin',(67.5044881891305,0.,6.99376217138448)) ;
#49816 = CARTESIAN_POINT('',(70.4986459245792,-5.5,6.80662731291894)) ;
#49817 = CARTESIAN_POINT('',(70.4986459245792,5.5,6.80662731291894)) ;
#49818 = CARTESIAN_POINT('',(70.4986459245792,0.,6.80662731291894)) ;
#49819 = CARTESIAN_POINT('',(64.5103304536818,5.5,7.18089702985002)) ;
#49820 = CARTESIAN_POINT('',(67.5044881891305,5.5,6.99376217138448)) ;
#49821 = CARTESIAN_POINT('',(64.5103304536818,-5.5,7.18089702985002)) ;
#49822 = CARTESIAN_POINT('',(64.5103304536818,0.,7.18089702985002)) ;
#49823 = CARTESIAN_POINT('',(67.5044881891305,-5.5,6.99376217138448)) ;
#49824 = CARTESIAN_POINT('Origin',(67.485774703284,0.,6.69434639783962)) ;
#49825 = CARTESIAN_POINT('',(70.4799324387326,5.5,6.50721153937407)) ;
#49826 = CARTESIAN_POINT('',(70.4799324387326,-5.5,6.50721153937407)) ;
#49827 = CARTESIAN_POINT('',(70.4799324387326,0.,6.50721153937407)) ;
#49828 = CARTESIAN_POINT('',(64.4916169678353,-5.5,6.88148125630516)) ;
#49829 = CARTESIAN_POINT('',(67.485774703284,-5.5,6.69434639783962)) ;
#49830 = CARTESIAN_POINT('',(64.4916169678353,5.5,6.88148125630516)) ;
#49831 = CARTESIAN_POINT('',(64.4916169678353,0.,6.88148125630516)) ;
#49832 = CARTESIAN_POINT('',(67.485774703284,5.5,6.69434639783962)) ;
#49833 = CARTESIAN_POINT('Origin',(67.4951314462072,-5.5,6.84405428461205)) ;
#49834 = CARTESIAN_POINT('',(64.5009737107586,-5.5,7.03118914307759)) ;
#49835 = CARTESIAN_POINT('',(70.4892891816559,-5.5,6.65691942614651)) ;
#49836 = CARTESIAN_POINT('Origin',(64.5009737107586,0.,7.03118914307759)) ;
#49837 = CARTESIAN_POINT('',(64.5009737107586,5.5,7.03118914307759)) ;
#49838 = CARTESIAN_POINT('Origin',(67.4951314462072,5.5,6.84405428461205)) ;
#49839 = CARTESIAN_POINT('',(70.4892891816559,5.5,6.65691942614651)) ;
#49840 = CARTESIAN_POINT('Origin',(70.4892891816559,0.,6.65691942614651)) ;
#49841 = CARTESIAN_POINT('',(0.,0.,0.)) ;
#49842 = CARTESIAN_POINT('Origin',(60.4,-0.3,15.5)) ;
#49843 = CARTESIAN_POINT('',(60.2362976425517,-0.3,15.030762280827)) ;
#49844 = CARTESIAN_POINT('',(60.221875,-0.3,14.8)) ;
#49845 = CARTESIAN_POINT('',(60.1330739299611,-0.3,13.3791828793774)) ;
#49846 = CARTESIAN_POINT('',(60.8,-0.3,14.9955308834865)) ;
#49847 = CARTESIAN_POINT('',(60.6362976425517,-0.3,15.005762280827)) ;
#49848 = CARTESIAN_POINT('',(60.8,-0.3,16.2)) ;
#49849 = CARTESIAN_POINT('',(60.8,-0.3,15.5)) ;
#49850 = CARTESIAN_POINT('',(60.,-0.3,16.2)) ;
#49851 = CARTESIAN_POINT('',(60.4,-0.3,16.2)) ;
#49852 = CARTESIAN_POINT('',(60.,-0.3,14.8)) ;
#49853 = CARTESIAN_POINT('',(60.,-0.3,15.5)) ;
#49854 = CARTESIAN_POINT('',(60.4,-0.3,14.8)) ;
#49855 = CARTESIAN_POINT('Origin',(60.8,0.,15.5)) ;
#49856 = CARTESIAN_POINT('',(60.8,0.3,14.9955308834865)) ;
#49857 = CARTESIAN_POINT('Origin',(60.8,0.,11.2)) ;
#49858 = CARTESIAN_POINT('',(60.8,0.3,16.2)) ;
#49859 = CARTESIAN_POINT('',(60.8,0.3,15.5)) ;
#49860 = CARTESIAN_POINT('',(60.8,0.,16.2)) ;
#49861 = CARTESIAN_POINT('Origin',(60.4,0.,16.2)) ;
#49862 = CARTESIAN_POINT('',(60.,0.3,16.2)) ;
#49863 = CARTESIAN_POINT('',(60.4,0.3,16.2)) ;
#49864 = CARTESIAN_POINT('',(60.,0.,16.2)) ;
#49865 = CARTESIAN_POINT('Origin',(60.4,0.,14.8)) ;
#49866 = CARTESIAN_POINT('',(60.221875,0.3,14.8)) ;
#49867 = CARTESIAN_POINT('',(60.221875,0.,14.8)) ;
#49868 = CARTESIAN_POINT('',(60.,0.3,14.8)) ;
#49869 = CARTESIAN_POINT('',(60.,0.,14.8)) ;
#49870 = CARTESIAN_POINT('',(60.4,0.3,14.8)) ;
#49871 = CARTESIAN_POINT('Origin',(60.,0.,15.5)) ;
#49872 = CARTESIAN_POINT('',(60.,0.3,15.5)) ;
#49873 = CARTESIAN_POINT('Origin',(60.4,0.3,15.5)) ;
#49874 = CARTESIAN_POINT('',(60.2362976425517,0.3,15.030762280827)) ;
#49875 = CARTESIAN_POINT('',(60.1330739299611,0.3,13.3791828793774)) ;
#49876 = CARTESIAN_POINT('',(60.6362976425517,0.3,15.005762280827)) ;
#49877 = CARTESIAN_POINT('Origin',(60.,0.,11.25)) ;
#49878 = CARTESIAN_POINT('',(59.7629625126103,4.65365783675994E-16,7.45740020176502)) ;
#49879 = CARTESIAN_POINT('Origin',(60.,0.,11.25)) ;
#49880 = CARTESIAN_POINT('Origin',(60.,0.,11.25)) ;
#49881 = CARTESIAN_POINT('',(59.7816759984569,4.28626379701574E-16,7.75681597530989)) ;
#49882 = CARTESIAN_POINT('Origin',(60.,0.,11.25)) ;
#49883 = CARTESIAN_POINT('Origin',(60.4,0.,11.225)) ;
#49884 = CARTESIAN_POINT('',(60.5816759984569,-4.28626379701574E-16,7.70681597530989)) ;
#49885 = CARTESIAN_POINT('',(60.1816759984569,4.28626379701574E-16,7.73181597530989)) ;
#49886 = CARTESIAN_POINT('Origin',(60.8,0.,11.2)) ;
#49887 = CARTESIAN_POINT('Origin',(60.4,0.,11.225)) ;
#49888 = CARTESIAN_POINT('',(60.5629625126103,4.65365783675994E-16,7.40740020176502)) ;
#49889 = CARTESIAN_POINT('Origin',(60.8,0.,11.2)) ;
#49890 = CARTESIAN_POINT('',(60.1629625126103,4.65365783675994E-16,7.43240020176502)) ;
#49891 = CARTESIAN_POINT('Origin',(60.8,0.,11.2)) ;
#49892 = CARTESIAN_POINT('',(0.,0.,0.)) ;
#49893 = CARTESIAN_POINT('',(0.,0.,0.)) ;
#49894 = CARTESIAN_POINT('',(0.,0.,0.)) ;
#49895 = CARTESIAN_POINT('',(-20.,0.,0.)) ;
#49896 = CARTESIAN_POINT('',(0.,0.,0.)) ;
#49897 = CARTESIAN_POINT('',(0.,0.,0.)) ;
#49898 = CARTESIAN_POINT('',(0.,0.,0.)) ;
#49899 = CARTESIAN_POINT('',(0.,0.,0.)) ;
#49900 = CARTESIAN_POINT('Origin',(0.,0.,-3.1)) ;
#49901 = CARTESIAN_POINT('',(-0.6,7.34788079488412E-17,-6.2)) ;
#49902 = CARTESIAN_POINT('Origin',(0.,0.,-6.2)) ;
#49903 = CARTESIAN_POINT('',(-0.6,7.34788079488412E-17,0.)) ;
#49904 = CARTESIAN_POINT('',(-0.6,7.34788079488412E-17,-3.1)) ;
#49905 = CARTESIAN_POINT('Origin',(0.,0.,0.)) ;
#49906 = CARTESIAN_POINT('Origin',(0.,0.,-6.2)) ;
#49907 = CARTESIAN_POINT('Origin',(0.475,0.822724133595217,0.375)) ;
#49908 = CARTESIAN_POINT('',(-2.77555756156289E-16,1.09696551146029,0.75)) ;
#49909 = CARTESIAN_POINT('',(-2.77555756156289E-16,1.09696551146029,0.)) ;
#49910 = CARTESIAN_POINT('',(-2.77555756156289E-16,1.09696551146029,0.375)) ;
#49911 = CARTESIAN_POINT('',(0.95,0.548482755730144,0.75)) ;
#49912 = CARTESIAN_POINT('',(0.475,0.822724133595217,0.75)) ;
#49913 = CARTESIAN_POINT('',(0.95,0.548482755730144,0.)) ;
#49914 = CARTESIAN_POINT('',(0.95,0.548482755730144,0.375)) ;
#49915 = CARTESIAN_POINT('',(0.475,0.822724133595217,2.77555756156289E-17)) ;
#49916 = CARTESIAN_POINT('Origin',(-0.475,-0.822724133595217,0.375)) ;
#49917 = CARTESIAN_POINT('',(2.77555756156289E-16,-1.09696551146029,0.75)) ;
#49918 = CARTESIAN_POINT('',(2.77555756156289E-16,-1.09696551146029,0.)) ;
#49919 = CARTESIAN_POINT('',(2.77555756156289E-16,-1.09696551146029,0.375)) ;
#49920 = CARTESIAN_POINT('',(-0.95,-0.548482755730144,0.75)) ;
#49921 = CARTESIAN_POINT('',(-0.475,-0.822724133595217,0.75)) ;
#49922 = CARTESIAN_POINT('',(-0.95,-0.548482755730144,0.)) ;
#49923 = CARTESIAN_POINT('',(-0.95,-0.548482755730144,0.375)) ;
#49924 = CARTESIAN_POINT('',(-0.475,-0.822724133595217,2.77555756156289E-17)) ;
#49925 = CARTESIAN_POINT('Origin',(0.,0.,0.75)) ;
#49926 = CARTESIAN_POINT('',(-0.95,0.548482755730144,0.75)) ;
#49927 = CARTESIAN_POINT('',(-0.475,0.822724133595217,0.75)) ;
#49928 = CARTESIAN_POINT('',(-0.95,0.,0.75)) ;
#49929 = CARTESIAN_POINT('',(0.95,-0.548482755730144,0.75)) ;
#49930 = CARTESIAN_POINT('',(0.475,-0.822724133595217,0.75)) ;
#49931 = CARTESIAN_POINT('',(0.95,0.,0.75)) ;
#49932 = CARTESIAN_POINT('Origin',(-0.475,0.822724133595217,0.375)) ;
#49933 = CARTESIAN_POINT('',(-0.95,0.548482755730144,0.)) ;
#49934 = CARTESIAN_POINT('',(-0.95,0.548482755730144,0.375)) ;
#49935 = CARTESIAN_POINT('',(-0.475,0.822724133595217,-2.77555756156289E-17)) ;
#49936 = CARTESIAN_POINT('Origin',(0.475,-0.822724133595217,0.375)) ;
#49937 = CARTESIAN_POINT('',(0.95,-0.548482755730144,0.)) ;
#49938 = CARTESIAN_POINT('',(0.95,-0.548482755730144,0.375)) ;
#49939 = CARTESIAN_POINT('',(0.475,-0.822724133595217,-2.77555756156289E-17)) ;
#49940 = CARTESIAN_POINT('Origin',(-0.95,0.,0.375)) ;
#49941 = CARTESIAN_POINT('',(-0.95,0.,0.)) ;
#49942 = CARTESIAN_POINT('Origin',(0.95,0.,0.375)) ;
#49943 = CARTESIAN_POINT('',(0.95,0.,0.)) ;
#49944 = CARTESIAN_POINT('Origin',(0.,0.,0.)) ;
#49945 = CARTESIAN_POINT('',(0.,0.,0.)) ;
#49946 = CARTESIAN_POINT('Origin',(0.,0.,0.)) ;
#49947 = CARTESIAN_POINT('',(-0.6,-7.34788079488412E-17,-0.5)) ;
#49948 = CARTESIAN_POINT('Origin',(0.,0.,-0.5)) ;
#49949 = CARTESIAN_POINT('',(-0.6,7.34788079488412E-17,0.5)) ;
#49950 = CARTESIAN_POINT('',(-0.6,-7.34788079488412E-17,0.)) ;
#49951 = CARTESIAN_POINT('Origin',(0.,0.,0.5)) ;
#49952 = CARTESIAN_POINT('Origin',(0.475,-0.822724133595217,0.)) ;
#49953 = CARTESIAN_POINT('',(-2.77555756156289E-16,-1.09696551146029,-0.5)) ;
#49954 = CARTESIAN_POINT('',(-2.77555756156289E-16,-1.09696551146029,0.5)) ;
#49955 = CARTESIAN_POINT('',(-2.77555756156289E-16,-1.09696551146029,0.)) ;
#49956 = CARTESIAN_POINT('',(0.95,-0.548482755730144,-0.5)) ;
#49957 = CARTESIAN_POINT('',(0.475,-0.822724133595217,-0.5)) ;
#49958 = CARTESIAN_POINT('',(0.95,-0.548482755730144,0.5)) ;
#49959 = CARTESIAN_POINT('',(0.95,-0.548482755730144,0.)) ;
#49960 = CARTESIAN_POINT('',(0.475,-0.822724133595217,0.5)) ;
#49961 = CARTESIAN_POINT('Origin',(-0.475,0.822724133595217,0.)) ;
#49962 = CARTESIAN_POINT('',(2.77555756156289E-16,1.09696551146029,-0.5)) ;
#49963 = CARTESIAN_POINT('',(2.77555756156289E-16,1.09696551146029,0.5)) ;
#49964 = CARTESIAN_POINT('',(2.77555756156289E-16,1.09696551146029,0.)) ;
#49965 = CARTESIAN_POINT('',(-0.95,0.548482755730144,-0.5)) ;
#49966 = CARTESIAN_POINT('',(-0.475,0.822724133595217,-0.5)) ;
#49967 = CARTESIAN_POINT('',(-0.95,0.548482755730144,0.5)) ;
#49968 = CARTESIAN_POINT('',(-0.95,0.548482755730144,0.)) ;
#49969 = CARTESIAN_POINT('',(-0.475,0.822724133595217,0.5)) ;
#49970 = CARTESIAN_POINT('Origin',(0.,0.,-0.5)) ;
#49971 = CARTESIAN_POINT('',(-0.95,-0.548482755730144,-0.5)) ;
#49972 = CARTESIAN_POINT('',(-0.475,-0.822724133595217,-0.5)) ;
#49973 = CARTESIAN_POINT('',(-0.95,0.,-0.5)) ;
#49974 = CARTESIAN_POINT('',(0.95,0.548482755730144,-0.5)) ;
#49975 = CARTESIAN_POINT('',(0.475,0.822724133595217,-0.5)) ;
#49976 = CARTESIAN_POINT('',(0.95,0.,-0.5)) ;
#49977 = CARTESIAN_POINT('Origin',(-0.475,-0.822724133595217,0.)) ;
#49978 = CARTESIAN_POINT('',(-0.95,-0.548482755730144,0.5)) ;
#49979 = CARTESIAN_POINT('',(-0.95,-0.548482755730144,0.)) ;
#49980 = CARTESIAN_POINT('',(-0.475,-0.822724133595217,0.5)) ;
#49981 = CARTESIAN_POINT('Origin',(0.475,0.822724133595217,0.)) ;
#49982 = CARTESIAN_POINT('',(0.95,0.548482755730144,0.5)) ;
#49983 = CARTESIAN_POINT('',(0.95,0.548482755730144,0.)) ;
#49984 = CARTESIAN_POINT('',(0.475,0.822724133595217,0.5)) ;
#49985 = CARTESIAN_POINT('Origin',(-0.95,0.,0.)) ;
#49986 = CARTESIAN_POINT('',(-0.95,0.,0.5)) ;
#49987 = CARTESIAN_POINT('Origin',(0.95,0.,0.)) ;
#49988 = CARTESIAN_POINT('',(0.95,0.,0.5)) ;
#49989 = CARTESIAN_POINT('Origin',(0.,0.,0.5)) ;
#49990 = CARTESIAN_POINT('',(0.,0.,0.)) ;
#49991 = CARTESIAN_POINT('Origin',(0.,0.,-1.5)) ;
#49992 = CARTESIAN_POINT('',(-0.4,4.89858719658941E-17,-3.)) ;
#49993 = CARTESIAN_POINT('Origin',(0.,0.,-3.)) ;
#49994 = CARTESIAN_POINT('',(-0.4,4.89858719658941E-17,0.)) ;
#49995 = CARTESIAN_POINT('',(-0.4,4.89858719658941E-17,-1.5)) ;
#49996 = CARTESIAN_POINT('Origin',(0.,0.,0.)) ;
#49997 = CARTESIAN_POINT('Origin',(0.,0.,-3.)) ;
#49998 = CARTESIAN_POINT('Origin',(0.325,0.562916512459885,0.265)) ;
#49999 = CARTESIAN_POINT('',(0.,0.750555349946514,0.53)) ;
#50000 = CARTESIAN_POINT('',(0.,0.750555349946514,0.)) ;
#50001 = CARTESIAN_POINT('',(0.,0.750555349946514,0.265)) ;
#50002 = CARTESIAN_POINT('',(0.65,0.375277674973257,0.53)) ;
#50003 = CARTESIAN_POINT('',(0.325,0.562916512459885,0.53)) ;
#50004 = CARTESIAN_POINT('',(0.65,0.375277674973257,0.)) ;
#50005 = CARTESIAN_POINT('',(0.65,0.375277674973257,0.265)) ;
#50006 = CARTESIAN_POINT('',(0.325,0.562916512459885,0.)) ;
#50007 = CARTESIAN_POINT('Origin',(-0.325,-0.562916512459885,0.265)) ;
#50008 = CARTESIAN_POINT('',(0.,-0.750555349946514,0.53)) ;
#50009 = CARTESIAN_POINT('',(0.,-0.750555349946514,0.)) ;
#50010 = CARTESIAN_POINT('',(0.,-0.750555349946514,0.265)) ;
#50011 = CARTESIAN_POINT('',(-0.65,-0.375277674973257,0.53)) ;
#50012 = CARTESIAN_POINT('',(-0.325,-0.562916512459885,0.53)) ;
#50013 = CARTESIAN_POINT('',(-0.65,-0.375277674973257,0.)) ;
#50014 = CARTESIAN_POINT('',(-0.65,-0.375277674973257,0.265)) ;
#50015 = CARTESIAN_POINT('',(-0.325,-0.562916512459885,0.)) ;
#50016 = CARTESIAN_POINT('Origin',(0.,0.,0.53)) ;
#50017 = CARTESIAN_POINT('',(-0.65,0.375277674973257,0.53)) ;
#50018 = CARTESIAN_POINT('',(-0.325,0.562916512459885,0.53)) ;
#50019 = CARTESIAN_POINT('',(-0.65,0.,0.53)) ;
#50020 = CARTESIAN_POINT('',(0.65,-0.375277674973257,0.53)) ;
#50021 = CARTESIAN_POINT('',(0.325,-0.562916512459885,0.53)) ;
#50022 = CARTESIAN_POINT('',(0.65,0.,0.53)) ;
#50023 = CARTESIAN_POINT('Origin',(-0.325,0.562916512459885,0.265)) ;
#50024 = CARTESIAN_POINT('',(-0.65,0.375277674973257,0.)) ;
#50025 = CARTESIAN_POINT('',(-0.65,0.375277674973257,0.265)) ;
#50026 = CARTESIAN_POINT('',(-0.325,0.562916512459885,0.)) ;
#50027 = CARTESIAN_POINT('Origin',(0.325,-0.562916512459885,0.265)) ;
#50028 = CARTESIAN_POINT('',(0.65,-0.375277674973257,0.)) ;
#50029 = CARTESIAN_POINT('',(0.65,-0.375277674973257,0.265)) ;
#50030 = CARTESIAN_POINT('',(0.325,-0.562916512459885,0.)) ;
#50031 = CARTESIAN_POINT('Origin',(-0.65,0.,0.265)) ;
#50032 = CARTESIAN_POINT('',(-0.65,0.,0.)) ;
#50033 = CARTESIAN_POINT('Origin',(0.65,0.,0.265)) ;
#50034 = CARTESIAN_POINT('',(0.65,0.,0.)) ;
#50035 = CARTESIAN_POINT('Origin',(0.,0.,0.)) ;
#50036 = CARTESIAN_POINT('',(0.,0.,0.)) ;
#50037 = CARTESIAN_POINT('Origin',(-53.,20.,92.)) ;
#50038 = CARTESIAN_POINT('',(-53.5,19.7,92.)) ;
#50039 = CARTESIAN_POINT('Origin',(-53.,19.7,92.)) ;
#50040 = CARTESIAN_POINT('',(-53.5,20.3,92.)) ;
#50041 = CARTESIAN_POINT('',(-53.5,20.,92.)) ;
#50042 = CARTESIAN_POINT('Origin',(-53.,20.3,92.)) ;
#50043 = CARTESIAN_POINT('Origin',(-52.575,20.,92.7361215932168)) ;
#50044 = CARTESIAN_POINT('',(-53.,19.7,92.9814954576224)) ;
#50045 = CARTESIAN_POINT('',(-53.,20.3,92.9814954576224)) ;
#50046 = CARTESIAN_POINT('',(-53.,20.,92.9814954576224)) ;
#50047 = CARTESIAN_POINT('',(-52.15,19.7,92.4907477288112)) ;
#50048 = CARTESIAN_POINT('',(-52.575,19.7,92.7361215932168)) ;
#50049 = CARTESIAN_POINT('',(-52.15,20.3,92.4907477288112)) ;
#50050 = CARTESIAN_POINT('',(-52.15,20.,92.4907477288112)) ;
#50051 = CARTESIAN_POINT('',(-52.575,20.3,92.7361215932168)) ;
#50052 = CARTESIAN_POINT('Origin',(-53.425,20.,91.2638784067832)) ;
#50053 = CARTESIAN_POINT('',(-53.,19.7,91.0185045423776)) ;
#50054 = CARTESIAN_POINT('',(-53.,20.3,91.0185045423776)) ;
#50055 = CARTESIAN_POINT('',(-53.,20.,91.0185045423776)) ;
#50056 = CARTESIAN_POINT('',(-53.85,19.7,91.5092522711888)) ;
#50057 = CARTESIAN_POINT('',(-53.425,19.7,91.2638784067832)) ;
#50058 = CARTESIAN_POINT('',(-53.85,20.3,91.5092522711888)) ;
#50059 = CARTESIAN_POINT('',(-53.85,20.,91.5092522711888)) ;
#50060 = CARTESIAN_POINT('',(-53.425,20.3,91.2638784067832)) ;
#50061 = CARTESIAN_POINT('Origin',(-53.,19.7,92.)) ;
#50062 = CARTESIAN_POINT('',(-53.85,19.7,92.4907477288112)) ;
#50063 = CARTESIAN_POINT('',(-53.425,19.7,92.7361215932168)) ;
#50064 = CARTESIAN_POINT('',(-53.85,19.7,92.)) ;
#50065 = CARTESIAN_POINT('',(-52.15,19.7,91.5092522711888)) ;
#50066 = CARTESIAN_POINT('',(-52.575,19.7,91.2638784067832)) ;
#50067 = CARTESIAN_POINT('',(-52.15,19.7,92.)) ;
#50068 = CARTESIAN_POINT('Origin',(-53.425,20.,92.7361215932168)) ;
#50069 = CARTESIAN_POINT('',(-53.85,20.3,92.4907477288112)) ;
#50070 = CARTESIAN_POINT('',(-53.85,20.,92.4907477288112)) ;
#50071 = CARTESIAN_POINT('',(-53.425,20.3,92.7361215932168)) ;
#50072 = CARTESIAN_POINT('Origin',(-52.575,20.,91.2638784067832)) ;
#50073 = CARTESIAN_POINT('',(-52.15,20.3,91.5092522711888)) ;
#50074 = CARTESIAN_POINT('',(-52.15,20.,91.5092522711888)) ;
#50075 = CARTESIAN_POINT('',(-52.575,20.3,91.2638784067832)) ;
#50076 = CARTESIAN_POINT('Origin',(-53.85,20.,92.)) ;
#50077 = CARTESIAN_POINT('',(-53.85,20.3,92.)) ;
#50078 = CARTESIAN_POINT('Origin',(-52.15,20.,92.)) ;
#50079 = CARTESIAN_POINT('',(-52.15,20.3,92.)) ;
#50080 = CARTESIAN_POINT('Origin',(-53.,20.3,92.)) ;
#50081 = CARTESIAN_POINT('',(0.,0.,0.)) ;
#50082 = CARTESIAN_POINT('Origin',(0.,0.,44.)) ;
#50083 = CARTESIAN_POINT('',(-0.45,-5.51091059616309E-17,44.)) ;
#50084 = CARTESIAN_POINT('Origin',(0.,0.,44.)) ;
#50085 = CARTESIAN_POINT('',(-0.245,-3.00038465791102E-17,44.)) ;
#50086 = CARTESIAN_POINT('Origin',(0.,0.,44.)) ;
#50087 = CARTESIAN_POINT('Origin',(0.,0.,44.1)) ;
#50088 = CARTESIAN_POINT('',(-0.45,-5.51091059616309E-17,44.2)) ;
#50089 = CARTESIAN_POINT('Origin',(0.,0.,44.2)) ;
#50090 = CARTESIAN_POINT('',(-0.45,-5.51091059616309E-17,44.1)) ;
#50091 = CARTESIAN_POINT('Origin',(0.,0.,44.2)) ;
#50092 = CARTESIAN_POINT('Origin',(0.,0.,43.2)) ;
#50093 = CARTESIAN_POINT('',(-0.245,-3.00038465791102E-17,42.4)) ;
#50094 = CARTESIAN_POINT('',(-0.245,-3.00038465791102E-17,43.2)) ;
#50095 = CARTESIAN_POINT('Origin',(0.,0.,42.4)) ;
#50096 = CARTESIAN_POINT('Origin',(0.,0.,42.4)) ;
#50097 = CARTESIAN_POINT('',(0.,0.,0.)) ;
#50098 = CARTESIAN_POINT('Origin',(0.,0.,44.8)) ;
#50099 = CARTESIAN_POINT('',(-0.45,-5.51091059616309E-17,44.8)) ;
#50100 = CARTESIAN_POINT('Origin',(0.,0.,44.8)) ;
#50101 = CARTESIAN_POINT('',(-0.245,-3.00038465791102E-17,44.8)) ;
#50102 = CARTESIAN_POINT('Origin',(0.,0.,44.8)) ;
#50103 = CARTESIAN_POINT('Origin',(0.,0.,44.9)) ;
#50104 = CARTESIAN_POINT('',(-0.45,-5.51091059616309E-17,45.)) ;
#50105 = CARTESIAN_POINT('Origin',(0.,0.,45.)) ;
#50106 = CARTESIAN_POINT('',(-0.45,-5.51091059616309E-17,44.9)) ;
#50107 = CARTESIAN_POINT('Origin',(0.,0.,45.)) ;
#50108 = CARTESIAN_POINT('Origin',(0.,0.,43.7)) ;
#50109 = CARTESIAN_POINT('',(-0.245,-3.00038465791102E-17,42.6)) ;
#50110 = CARTESIAN_POINT('',(-0.245,-3.00038465791102E-17,43.7)) ;
#50111 = CARTESIAN_POINT('Origin',(0.,0.,42.6)) ;
#50112 = CARTESIAN_POINT('Origin',(0.,0.,42.6)) ;
#50113 = CARTESIAN_POINT('',(0.,0.,0.)) ;
#50114 = CARTESIAN_POINT('Origin',(0.25,0.,1.86698729810778)) ;
#50115 = CARTESIAN_POINT('',(0.171681132240627,-0.246019488725134,1.8)) ;
#50116 = CARTESIAN_POINT('',(1.64540693022728E-16,-0.25,1.8)) ;
#50117 = CARTESIAN_POINT('Origin',(5.27355936696949E-16,0.,1.8)) ;
#50118 = CARTESIAN_POINT('',(0.171681132240627,0.246019488725134,1.8)) ;
#50119 = CARTESIAN_POINT('Ctrl Pts',(0.171681132240627,0.246019488725134,
1.8)) ;
#50120 = CARTESIAN_POINT('Ctrl Pts',(0.171928929654082,0.245846566893906,
1.799075207463)) ;
#50121 = CARTESIAN_POINT('Ctrl Pts',(0.172184099341621,0.24566794421234,1.79815279520613)) ;
#50122 = CARTESIAN_POINT('Ctrl Pts',(0.176787603683127,0.242434088321297,
1.782012704586)) ;
#50123 = CARTESIAN_POINT('Ctrl Pts',(0.183141637145544,0.237803273510375,
1.76748264287115)) ;
#50124 = CARTESIAN_POINT('Ctrl Pts',(0.205276678568417,0.219605090033885,
1.72686655424502)) ;
#50125 = CARTESIAN_POINT('Ctrl Pts',(0.22386989322167,0.201428663227279,1.70350036667433)) ;
#50126 = CARTESIAN_POINT('Ctrl Pts',(0.256050927678194,0.158678076494978,
1.66597959949031)) ;
#50127 = CARTESIAN_POINT('Ctrl Pts',(0.272049768241992,0.13073954601732,1.6494715036482)) ;
#50128 = CARTESIAN_POINT('Ctrl Pts',(0.294064901325084,0.0680421958529071,
1.6272468646998)) ;
#50129 = CARTESIAN_POINT('Ctrl Pts',(0.3,0.0332423590517548,1.62156571262682)) ;
#50130 = CARTESIAN_POINT('Ctrl Pts',(0.3,-0.0332423590517547,1.62156571262682)) ;
#50131 = CARTESIAN_POINT('Ctrl Pts',(0.294064901325084,-0.068042195852907,
1.6272468646998)) ;
#50132 = CARTESIAN_POINT('Ctrl Pts',(0.272049768241992,-0.13073954601732,
1.6494715036482)) ;
#50133 = CARTESIAN_POINT('Ctrl Pts',(0.256050927678194,-0.158678076494978,
1.66597959949031)) ;
#50134 = CARTESIAN_POINT('Ctrl Pts',(0.22386989322167,-0.201428663227279,
1.70350036667433)) ;
#50135 = CARTESIAN_POINT('Ctrl Pts',(0.205276678568417,-0.219605090033885,
1.72686655424502)) ;
#50136 = CARTESIAN_POINT('Ctrl Pts',(0.183141637145543,-0.237803273510375,
1.76748264287115)) ;
#50137 = CARTESIAN_POINT('Ctrl Pts',(0.176787603683127,-0.242434088321297,
1.782012704586)) ;
#50138 = CARTESIAN_POINT('Ctrl Pts',(0.172184099341621,-0.24566794421234,
1.79815279520613)) ;
#50139 = CARTESIAN_POINT('Ctrl Pts',(0.171928929654082,-0.245846566893906,
1.799075207463)) ;
#50140 = CARTESIAN_POINT('Ctrl Pts',(0.171681132240627,-0.246019488725134,
1.8)) ;
#50141 = CARTESIAN_POINT('',(1.64540693022728E-16,0.25,1.8)) ;
#50142 = CARTESIAN_POINT('Origin',(5.27355936696949E-16,0.,1.8)) ;
#50143 = CARTESIAN_POINT('',(5.55111512312578E-17,3.06161699786839E-17,2.05881904510252)) ;
#50144 = CARTESIAN_POINT('Origin',(0.,0.,1.8)) ;
#50145 = CARTESIAN_POINT('',(0.370590477448738,3.06161699786838E-17,2.15811846425757)) ;
#50146 = CARTESIAN_POINT('',(0.18529523872437,3.06161699786838E-17,2.10846875468005)) ;
#50147 = CARTESIAN_POINT('',(0.5,0.25,1.93397459621556)) ;
#50148 = CARTESIAN_POINT('Origin',(0.499999999999999,0.,1.93397459621556)) ;
#50149 = CARTESIAN_POINT('',(0.5,-0.25,1.93397459621556)) ;
#50150 = CARTESIAN_POINT('Origin',(0.5,0.,1.93397459621556)) ;
#50151 = CARTESIAN_POINT('Origin',(0.499999999999999,0.,1.93397459621556)) ;
#50152 = CARTESIAN_POINT('Origin',(0.,0.,1.8)) ;
#50153 = CARTESIAN_POINT('Origin',(1.,0.,2.8)) ;
#50154 = CARTESIAN_POINT('',(1.,0.25,2.8)) ;
#50155 = CARTESIAN_POINT('',(1.,-0.25,2.8)) ;
#50156 = CARTESIAN_POINT('Origin',(1.,0.,2.8)) ;
#50157 = CARTESIAN_POINT('Origin',(1.,0.,2.8)) ;
#50158 = CARTESIAN_POINT('Origin',(0.866025403784438,0.,3.3)) ;
#50159 = CARTESIAN_POINT('',(0.866025403784438,-0.25,3.3)) ;
#50160 = CARTESIAN_POINT('',(0.866025403784438,0.25,3.3)) ;
#50161 = CARTESIAN_POINT('Origin',(0.866025403784438,0.,3.3)) ;
#50162 = CARTESIAN_POINT('Origin',(0.866025403784438,0.,3.3)) ;
#50163 = CARTESIAN_POINT('Origin',(0.5,0.,3.66602540378444)) ;
#50164 = CARTESIAN_POINT('',(0.499999999999999,-0.25,3.66602540378444)) ;
#50165 = CARTESIAN_POINT('',(0.499999999999999,0.25,3.66602540378444)) ;
#50166 = CARTESIAN_POINT('Origin',(0.5,0.,3.66602540378444)) ;
#50167 = CARTESIAN_POINT('Origin',(0.5,0.,3.66602540378444)) ;
#50168 = CARTESIAN_POINT('Origin',(-1.83697019872103E-16,0.,3.8)) ;
#50169 = CARTESIAN_POINT('',(-1.12986998865286E-18,-0.25,3.8)) ;
#50170 = CARTESIAN_POINT('',(-1.12986998865286E-18,0.25,3.8)) ;
#50171 = CARTESIAN_POINT('Origin',(-1.94289029309402E-16,0.,3.8)) ;
#50172 = CARTESIAN_POINT('',(-0.0647047612756307,-7.92404787857945E-18,4.04148145657227)) ;
#50173 = CARTESIAN_POINT('Origin',(-2.22044604925031E-16,0.,3.8)) ;
#50174 = CARTESIAN_POINT('',(-1.99005104861445E-16,-1.87469972832732E-33,
4.05)) ;
#50175 = CARTESIAN_POINT('Origin',(-1.83697019872103E-16,0.,3.8)) ;
#50176 = CARTESIAN_POINT('Origin',(-2.22044604925031E-16,0.,3.8)) ;
#50177 = CARTESIAN_POINT('Origin',(-0.5,0.,3.66602540378444)) ;
#50178 = CARTESIAN_POINT('',(-0.5,-0.25,3.66602540378444)) ;
#50179 = CARTESIAN_POINT('',(-0.564704761275631,-3.06161699786838E-17,3.90750686035671)) ;
#50180 = CARTESIAN_POINT('Origin',(-0.5,0.,3.66602540378444)) ;
#50181 = CARTESIAN_POINT('',(-0.5,0.25,3.66602540378444)) ;
#50182 = CARTESIAN_POINT('Origin',(-0.5,0.,3.66602540378444)) ;
#50183 = CARTESIAN_POINT('',(-0.676776695296637,-3.06161699786838E-17,3.84280209908108)) ;
#50184 = CARTESIAN_POINT('Origin',(-0.5,0.,3.66602540378444)) ;
#50185 = CARTESIAN_POINT('Origin',(-0.5,0.,3.66602540378444)) ;
#50186 = CARTESIAN_POINT('Origin',(-0.866025403784439,0.,3.3)) ;
#50187 = CARTESIAN_POINT('',(-0.866025403784439,-0.25,3.3)) ;
#50188 = CARTESIAN_POINT('',(-1.04280209908108,-3.06161699786838E-17,3.47677669529664)) ;
#50189 = CARTESIAN_POINT('Origin',(-0.866025403784439,0.,3.3)) ;
#50190 = CARTESIAN_POINT('',(-0.866025403784439,0.25,3.3)) ;
#50191 = CARTESIAN_POINT('Origin',(-0.866025403784439,0.,3.3)) ;
#50192 = CARTESIAN_POINT('',(-1.10750686035671,-3.06161699786838E-17,3.36470476127563)) ;
#50193 = CARTESIAN_POINT('Origin',(-0.866025403784439,0.,3.3)) ;
#50194 = CARTESIAN_POINT('Origin',(-0.866025403784439,0.,3.3)) ;
#50195 = CARTESIAN_POINT('Origin',(-1.,0.,2.8)) ;
#50196 = CARTESIAN_POINT('',(-1.,-0.25,2.8)) ;
#50197 = CARTESIAN_POINT('',(-1.24148145657227,-3.06161699786838E-17,2.86470476127563)) ;
#50198 = CARTESIAN_POINT('Origin',(-1.,0.,2.8)) ;
#50199 = CARTESIAN_POINT('',(-1.,0.25,2.8)) ;
#50200 = CARTESIAN_POINT('Origin',(-1.,0.,2.8)) ;
#50201 = CARTESIAN_POINT('',(-1.24148145657227,-3.06161699786838E-17,2.73529523872437)) ;
#50202 = CARTESIAN_POINT('Origin',(-1.,0.,2.8)) ;
#50203 = CARTESIAN_POINT('Origin',(-1.,0.,2.8)) ;
#50204 = CARTESIAN_POINT('Origin',(-0.866025403784439,0.,2.3)) ;
#50205 = CARTESIAN_POINT('',(-0.866025403784439,-0.25,2.3)) ;
#50206 = CARTESIAN_POINT('',(-1.10750686035671,-3.06161699786838E-17,2.23529523872437)) ;
#50207 = CARTESIAN_POINT('Origin',(-0.866025403784439,0.,2.3)) ;
#50208 = CARTESIAN_POINT('',(-0.866025403784439,0.25,2.3)) ;
#50209 = CARTESIAN_POINT('Origin',(-0.866025403784439,0.,2.3)) ;
#50210 = CARTESIAN_POINT('',(-1.04280209908108,-3.06161699786838E-17,2.12322330470336)) ;
#50211 = CARTESIAN_POINT('Origin',(-0.866025403784439,0.,2.3)) ;
#50212 = CARTESIAN_POINT('Origin',(-0.866025403784439,0.,2.3)) ;
#50213 = CARTESIAN_POINT('Origin',(-0.5,0.,1.93397459621556)) ;
#50214 = CARTESIAN_POINT('',(-0.5,-0.25,1.93397459621556)) ;
#50215 = CARTESIAN_POINT('',(-0.676776695296637,-3.06161699786838E-17,1.75719790091892)) ;
#50216 = CARTESIAN_POINT('Origin',(-0.5,0.,1.93397459621556)) ;
#50217 = CARTESIAN_POINT('',(-0.5,0.25,1.93397459621556)) ;
#50218 = CARTESIAN_POINT('Origin',(-0.5,0.,1.93397459621556)) ;
#50219 = CARTESIAN_POINT('',(-0.56470476127563,-3.06161699786838E-17,1.69249313964329)) ;
#50220 = CARTESIAN_POINT('Origin',(-0.5,0.,1.93397459621556)) ;
#50221 = CARTESIAN_POINT('Origin',(-0.5,0.,1.93397459621556)) ;
#50222 = CARTESIAN_POINT('Origin',(0.5,0.,1.93397459621556)) ;
#50223 = CARTESIAN_POINT('Origin',(0.5,0.,1.93397459621556)) ;
#50224 = CARTESIAN_POINT('Origin',(0.866025403784439,0.,2.3)) ;
#50225 = CARTESIAN_POINT('',(0.866025403784438,-0.25,2.3)) ;
#50226 = CARTESIAN_POINT('',(0.866025403784438,0.25,2.3)) ;
#50227 = CARTESIAN_POINT('Origin',(0.866025403784439,0.,2.3)) ;
#50228 = CARTESIAN_POINT('Origin',(0.866025403784439,0.,2.3)) ;
#50229 = CARTESIAN_POINT('Origin',(0.933012701892219,0.,3.05)) ;
#50230 = CARTESIAN_POINT('',(0.741180954897479,3.06161699786838E-17,2.8)) ;
#50231 = CARTESIAN_POINT('Origin',(1.,0.,2.8)) ;
#50232 = CARTESIAN_POINT('Origin',(1.,0.,2.8)) ;
#50233 = CARTESIAN_POINT('',(0.641881535742425,3.06161699786838E-17,3.17059047744874)) ;
#50234 = CARTESIAN_POINT('',(0.691531245319952,3.06161699786838E-17,2.98529523872437)) ;
#50235 = CARTESIAN_POINT('Origin',(0.866025403784438,0.,3.3)) ;
#50236 = CARTESIAN_POINT('Origin',(0.866025403784438,0.,3.3)) ;
#50237 = CARTESIAN_POINT('Origin',(0.683012701892219,0.,3.48301270189222)) ;
#50238 = CARTESIAN_POINT('',(0.370590477448739,3.06161699786838E-17,3.44188153574243)) ;
#50239 = CARTESIAN_POINT('',(0.506236006595582,3.06161699786838E-17,3.30623600659558)) ;
#50240 = CARTESIAN_POINT('Origin',(0.5,0.,3.66602540378444)) ;
#50241 = CARTESIAN_POINT('Origin',(0.5,0.,3.66602540378444)) ;
#50242 = CARTESIAN_POINT('Origin',(0.25,0.,3.73301270189222)) ;
#50243 = CARTESIAN_POINT('',(-3.46944695195361E-16,3.06161699786838E-17,3.54118095489748)) ;
#50244 = CARTESIAN_POINT('',(0.185295238724369,3.06161699786838E-17,3.49153124531995)) ;
#50245 = CARTESIAN_POINT('Origin',(-2.4980018054066E-16,0.,3.8)) ;
#50246 = CARTESIAN_POINT('Origin',(-2.4980018054066E-16,0.,3.8)) ;
#50247 = CARTESIAN_POINT('Origin',(-0.25,0.,3.73301270189222)) ;
#50248 = CARTESIAN_POINT('',(-0.314704761275631,-3.06161699786838E-17,3.97449415846449)) ;
#50249 = CARTESIAN_POINT('Origin',(-0.5,0.,3.66602540378444)) ;
#50250 = CARTESIAN_POINT('Origin',(-0.68301270189222,0.,3.48301270189222)) ;
#50251 = CARTESIAN_POINT('',(-0.859789397188856,-3.06161699786838E-17,3.65978939718886)) ;
#50252 = CARTESIAN_POINT('Origin',(-0.866025403784439,0.,3.3)) ;
#50253 = CARTESIAN_POINT('Origin',(-0.933012701892219,0.,3.05)) ;
#50254 = CARTESIAN_POINT('',(-1.17449415846449,-3.06161699786838E-17,3.11470476127563)) ;
#50255 = CARTESIAN_POINT('Origin',(-1.,0.,2.8)) ;
#50256 = CARTESIAN_POINT('Origin',(-0.933012701892219,0.,2.55)) ;
#50257 = CARTESIAN_POINT('',(-1.17449415846449,-3.06161699786838E-17,2.48529523872437)) ;
#50258 = CARTESIAN_POINT('Origin',(-0.866025403784439,0.,2.3)) ;
#50259 = CARTESIAN_POINT('Origin',(-0.683012701892219,0.,2.11698729810778)) ;
#50260 = CARTESIAN_POINT('',(-0.859789397188856,-3.06161699786838E-17,1.94021060281114)) ;
#50261 = CARTESIAN_POINT('Origin',(-0.5,0.,1.93397459621556)) ;
#50262 = CARTESIAN_POINT('Origin',(-0.25,0.,1.86698729810778)) ;
#50263 = CARTESIAN_POINT('',(-0.3,5.50859672237977E-18,1.62156571262682)) ;
#50264 = CARTESIAN_POINT('',(-0.31470476127563,-3.06161699786838E-17,1.62550584153551)) ;
#50265 = CARTESIAN_POINT('',(-0.171681132240627,-0.246019488725134,1.8)) ;
#50266 = CARTESIAN_POINT('Ctrl Pts',(-0.171681132240627,-0.246019488725134,
1.8)) ;
#50267 = CARTESIAN_POINT('Ctrl Pts',(-0.172207810962449,-0.245651953617416,
1.79803440825089)) ;
#50268 = CARTESIAN_POINT('Ctrl Pts',(-0.172767621079718,-0.245258790470191,
1.7960802634788)) ;
#50269 = CARTESIAN_POINT('Ctrl Pts',(-0.178257858233088,-0.241371425647844,
1.77805114730154)) ;
#50270 = CARTESIAN_POINT('Ctrl Pts',(-0.185355094601362,-0.236127799089863,
1.76280751800332)) ;
#50271 = CARTESIAN_POINT('Ctrl Pts',(-0.209709816425776,-0.215576225066061,
1.72038403302066)) ;
#50272 = CARTESIAN_POINT('Ctrl Pts',(-0.229722022348292,-0.195109377237531,
1.69623535556665)) ;
#50273 = CARTESIAN_POINT('Ctrl Pts',(-0.26112090484938,-0.149973351529612,
1.66067985684946)) ;
#50274 = CARTESIAN_POINT('Ctrl Pts',(-0.275367273146093,-0.123095023040758,
1.6460810308757)) ;
#50275 = CARTESIAN_POINT('Ctrl Pts',(-0.294844938349426,-0.063608040301515,
1.62651059381835)) ;
#50276 = CARTESIAN_POINT('Ctrl Pts',(-0.3,-0.0309656629660992,1.62156571262682)) ;
#50277 = CARTESIAN_POINT('Ctrl Pts',(-0.3,3.46944695195361E-17,1.62156571262682)) ;
#50278 = CARTESIAN_POINT('Origin',(5.55111512312578E-17,0.,1.8)) ;
#50279 = CARTESIAN_POINT('',(-0.171681132240627,0.246019488725134,1.8)) ;
#50280 = CARTESIAN_POINT('Origin',(5.55111512312578E-17,0.,1.8)) ;
#50281 = CARTESIAN_POINT('Ctrl Pts',(-0.3,2.77555756156289E-17,1.62156571262682)) ;
#50282 = CARTESIAN_POINT('Ctrl Pts',(-0.3,0.0309656629660992,1.62156571262682)) ;
#50283 = CARTESIAN_POINT('Ctrl Pts',(-0.294844938349426,0.0636080403015151,
1.62651059381835)) ;
#50284 = CARTESIAN_POINT('Ctrl Pts',(-0.275367273146093,0.123095023040759,
1.6460810308757)) ;
#50285 = CARTESIAN_POINT('Ctrl Pts',(-0.26112090484938,0.149973351529612,
1.66067985684946)) ;
#50286 = CARTESIAN_POINT('Ctrl Pts',(-0.229722022348292,0.195109377237531,
1.69623535556665)) ;
#50287 = CARTESIAN_POINT('Ctrl Pts',(-0.209709816425776,0.215576225066061,
1.72038403302066)) ;
#50288 = CARTESIAN_POINT('Ctrl Pts',(-0.185355094601362,0.236127799089863,
1.76280751800332)) ;
#50289 = CARTESIAN_POINT('Ctrl Pts',(-0.178257858233088,0.241371425647844,
1.77805114730154)) ;
#50290 = CARTESIAN_POINT('Ctrl Pts',(-0.172767621079718,0.245258790470192,
1.7960802634788)) ;
#50291 = CARTESIAN_POINT('Ctrl Pts',(-0.172207810962449,0.245651953617416,
1.79803440825089)) ;
#50292 = CARTESIAN_POINT('Ctrl Pts',(-0.171681132240627,0.246019488725134,
1.8)) ;
#50293 = CARTESIAN_POINT('Origin',(0.683012701892219,0.,2.11698729810778)) ;
#50294 = CARTESIAN_POINT('',(0.641881535742426,3.06161699786838E-17,2.42940952255126)) ;
#50295 = CARTESIAN_POINT('',(0.506236006595582,3.06161699786838E-17,2.29376399340442)) ;
#50296 = CARTESIAN_POINT('Origin',(0.866025403784439,0.,2.3)) ;
#50297 = CARTESIAN_POINT('Origin',(0.866025403784439,0.,2.3)) ;
#50298 = CARTESIAN_POINT('Origin',(0.933012701892219,0.,2.55)) ;
#50299 = CARTESIAN_POINT('',(0.691531245319952,3.06161699786838E-17,2.61470476127563)) ;
#50300 = CARTESIAN_POINT('Origin',(0.,0.,1.8)) ;
#50301 = CARTESIAN_POINT('Origin',(0.,0.,1.8)) ;
#50302 = CARTESIAN_POINT('Origin',(0.,0.,0.)) ;
#50303 = CARTESIAN_POINT('',(-0.3,-3.67394039744206E-17,-1.8)) ;
#50304 = CARTESIAN_POINT('',(-0.3,-3.67394039744206E-17,0.)) ;
#50305 = CARTESIAN_POINT('Origin',(0.,0.,-1.8)) ;
#50306 = CARTESIAN_POINT('Origin',(0.,0.,1.8)) ;
#50307 = CARTESIAN_POINT('Origin',(0.,0.,-1.8)) ;
#50308 = CARTESIAN_POINT('Origin',(0.,0.,1.8)) ;
#50309 = CARTESIAN_POINT('',(-53.,51.5,25.)) ;
#50310 = CARTESIAN_POINT('',(-53.,-51.5,25.)) ;
#50311 = CARTESIAN_POINT('',(-53.,6.2,90.)) ;
#50312 = CARTESIAN_POINT('',(8.5,22.,32.)) ;
#50313 = CARTESIAN_POINT('',(-8.5,22.,32.)) ;
#50314 = CARTESIAN_POINT('',(8.5,-22.,32.)) ;
#50315 = CARTESIAN_POINT('',(-8.5,-22.,32.)) ;
#50316 = CARTESIAN_POINT('',(8.5,22.,26.3)) ;
#50317 = CARTESIAN_POINT('',(-8.5,22.,26.3)) ;
#50318 = CARTESIAN_POINT('',(8.5,-22.,26.3)) ;
#50319 = CARTESIAN_POINT('',(-8.5,-22.,26.3)) ;
#50320 = CARTESIAN_POINT('',(11.,10.,43.2)) ;
#50321 = CARTESIAN_POINT('',(-11.,10.,43.2)) ;
#50322 = CARTESIAN_POINT('',(11.,-10.,43.2)) ;
#50323 = CARTESIAN_POINT('',(-11.,-10.,43.2)) ;
#50324 = CARTESIAN_POINT('',(0.,0.,0.)) ;
#50325 = CARTESIAN_POINT('',(21.5,0.,0.)) ;
#50326 = CARTESIAN_POINT('',(31.9,0.,0.)) ;
#50327 = CARTESIAN_POINT('',(11.5,0.,24.)) ;
#50328 = CARTESIAN_POINT('',(-11.5,0.,24.)) ;
#50329 = CARTESIAN_POINT('',(0.,0.,0.)) ;
#50330 = CARTESIAN_POINT('',(0.,0.,0.)) ;
#50331 = CARTESIAN_POINT('',(0.,0.,0.)) ;
#50332 = CARTESIAN_POINT('',(0.,0.,0.)) ;
#50333 = CARTESIAN_POINT('',(0.,0.,0.)) ;
#50334 = CARTESIAN_POINT('',(0.,0.,0.)) ;
#50335 = UNCERTAINTY_MEASURE_WITH_UNIT(LENGTH_MEASURE(0.001),#50441,
'DISTANCE_ACCURACY_VALUE',
'Maximum model space distance between geometric entities at asserted c
onnectivities') ;
#50336 = UNCERTAINTY_MEASURE_WITH_UNIT(LENGTH_MEASURE(0.001),#50441,
'DISTANCE_ACCURACY_VALUE',
'Maximum model space distance between geometric entities at asserted c
onnectivities') ;
#50337 = UNCERTAINTY_MEASURE_WITH_UNIT(LENGTH_MEASURE(0.001),#50441,
'DISTANCE_ACCURACY_VALUE',
'Maximum model space distance between geometric entities at asserted c
onnectivities') ;
#50338 = UNCERTAINTY_MEASURE_WITH_UNIT(LENGTH_MEASURE(0.001),#50441,
'DISTANCE_ACCURACY_VALUE',
'Maximum model space distance between geometric entities at asserted c
onnectivities') ;
#50339 = UNCERTAINTY_MEASURE_WITH_UNIT(LENGTH_MEASURE(0.001),#50441,
'DISTANCE_ACCURACY_VALUE',
'Maximum model space distance between geometric entities at asserted c
onnectivities') ;
#50340 = UNCERTAINTY_MEASURE_WITH_UNIT(LENGTH_MEASURE(0.001),#50441,
'DISTANCE_ACCURACY_VALUE',
'Maximum model space distance between geometric entities at asserted c
onnectivities') ;
#50341 = UNCERTAINTY_MEASURE_WITH_UNIT(LENGTH_MEASURE(0.001),#50441,
'DISTANCE_ACCURACY_VALUE',
'Maximum model space distance between geometric entities at asserted c
onnectivities') ;
#50342 = UNCERTAINTY_MEASURE_WITH_UNIT(LENGTH_MEASURE(0.001),#50441,
'DISTANCE_ACCURACY_VALUE',
'Maximum model space distance between geometric entities at asserted c
onnectivities') ;
#50343 = UNCERTAINTY_MEASURE_WITH_UNIT(LENGTH_MEASURE(0.001),#50441,
'DISTANCE_ACCURACY_VALUE',
'Maximum model space distance between geometric entities at asserted c
onnectivities') ;
#50344 = UNCERTAINTY_MEASURE_WITH_UNIT(LENGTH_MEASURE(0.001),#50441,
'DISTANCE_ACCURACY_VALUE',
'Maximum model space distance between geometric entities at asserted c
onnectivities') ;
#50345 = UNCERTAINTY_MEASURE_WITH_UNIT(LENGTH_MEASURE(0.001),#50441,
'DISTANCE_ACCURACY_VALUE',
'Maximum model space distance between geometric entities at asserted c
onnectivities') ;
#50346 = UNCERTAINTY_MEASURE_WITH_UNIT(LENGTH_MEASURE(0.001),#50441,
'DISTANCE_ACCURACY_VALUE',
'Maximum model space distance between geometric entities at asserted c
onnectivities') ;
#50347 = UNCERTAINTY_MEASURE_WITH_UNIT(LENGTH_MEASURE(0.001),#50441,
'DISTANCE_ACCURACY_VALUE',
'Maximum model space distance between geometric entities at asserted c
onnectivities') ;
#50348 = UNCERTAINTY_MEASURE_WITH_UNIT(LENGTH_MEASURE(0.001),#50441,
'DISTANCE_ACCURACY_VALUE',
'Maximum model space distance between geometric entities at asserted c
onnectivities') ;
#50349 = UNCERTAINTY_MEASURE_WITH_UNIT(LENGTH_MEASURE(0.001),#50441,
'DISTANCE_ACCURACY_VALUE',
'Maximum model space distance between geometric entities at asserted c
onnectivities') ;
#50350 = UNCERTAINTY_MEASURE_WITH_UNIT(LENGTH_MEASURE(0.001),#50441,
'DISTANCE_ACCURACY_VALUE',
'Maximum model space distance between geometric entities at asserted c
onnectivities') ;
#50351 = UNCERTAINTY_MEASURE_WITH_UNIT(LENGTH_MEASURE(0.001),#50441,
'DISTANCE_ACCURACY_VALUE',
'Maximum model space distance between geometric entities at asserted c
onnectivities') ;
#50352 = UNCERTAINTY_MEASURE_WITH_UNIT(LENGTH_MEASURE(0.001),#50441,
'DISTANCE_ACCURACY_VALUE',
'Maximum model space distance between geometric entities at asserted c
onnectivities') ;
#50353 = UNCERTAINTY_MEASURE_WITH_UNIT(LENGTH_MEASURE(0.001),#50441,
'DISTANCE_ACCURACY_VALUE',
'Maximum model space distance between geometric entities at asserted c
onnectivities') ;
#50354 = UNCERTAINTY_MEASURE_WITH_UNIT(LENGTH_MEASURE(0.001),#50441,
'DISTANCE_ACCURACY_VALUE',
'Maximum model space distance between geometric entities at asserted c
onnectivities') ;
#50355 = UNCERTAINTY_MEASURE_WITH_UNIT(LENGTH_MEASURE(0.001),#50441,
'DISTANCE_ACCURACY_VALUE',
'Maximum model space distance between geometric entities at asserted c
onnectivities') ;
#50356 = UNCERTAINTY_MEASURE_WITH_UNIT(LENGTH_MEASURE(0.001),#50441,
'DISTANCE_ACCURACY_VALUE',
'Maximum model space distance between geometric entities at asserted c
onnectivities') ;
#50357 = UNCERTAINTY_MEASURE_WITH_UNIT(LENGTH_MEASURE(0.001),#50441,
'DISTANCE_ACCURACY_VALUE',
'Maximum model space distance between geometric entities at asserted c
onnectivities') ;
#50358 = UNCERTAINTY_MEASURE_WITH_UNIT(LENGTH_MEASURE(0.001),#50441,
'DISTANCE_ACCURACY_VALUE',
'Maximum model space distance between geometric entities at asserted c
onnectivities') ;
#50359 = UNCERTAINTY_MEASURE_WITH_UNIT(LENGTH_MEASURE(0.001),#50441,
'DISTANCE_ACCURACY_VALUE',
'Maximum model space distance between geometric entities at asserted c
onnectivities') ;
#50360 = UNCERTAINTY_MEASURE_WITH_UNIT(LENGTH_MEASURE(0.001),#50441,
'DISTANCE_ACCURACY_VALUE',
'Maximum model space distance between geometric entities at asserted c
onnectivities') ;
#50361 = UNCERTAINTY_MEASURE_WITH_UNIT(LENGTH_MEASURE(0.001),#50441,
'DISTANCE_ACCURACY_VALUE',
'Maximum model space distance between geometric entities at asserted c
onnectivities') ;
#50362 = UNCERTAINTY_MEASURE_WITH_UNIT(LENGTH_MEASURE(0.001),#50441,
'DISTANCE_ACCURACY_VALUE',
'Maximum model space distance between geometric entities at asserted c
onnectivities') ;
#50363 = UNCERTAINTY_MEASURE_WITH_UNIT(LENGTH_MEASURE(0.001),#50441,
'DISTANCE_ACCURACY_VALUE',
'Maximum model space distance between geometric entities at asserted c
onnectivities') ;
#50364 = UNCERTAINTY_MEASURE_WITH_UNIT(LENGTH_MEASURE(0.001),#50441,
'DISTANCE_ACCURACY_VALUE',
'Maximum model space distance between geometric entities at asserted c
onnectivities') ;
#50365 = UNCERTAINTY_MEASURE_WITH_UNIT(LENGTH_MEASURE(0.001),#50441,
'DISTANCE_ACCURACY_VALUE',
'Maximum model space distance between geometric entities at asserted c
onnectivities') ;
#50366 = UNCERTAINTY_MEASURE_WITH_UNIT(LENGTH_MEASURE(0.001),#50441,
'DISTANCE_ACCURACY_VALUE',
'Maximum model space distance between geometric entities at asserted c
onnectivities') ;
#50367 = UNCERTAINTY_MEASURE_WITH_UNIT(LENGTH_MEASURE(0.001),#50441,
'DISTANCE_ACCURACY_VALUE',
'Maximum model space distance between geometric entities at asserted c
onnectivities') ;
#50368 = UNCERTAINTY_MEASURE_WITH_UNIT(LENGTH_MEASURE(0.001),#50441,
'DISTANCE_ACCURACY_VALUE',
'Maximum model space distance between geometric entities at asserted c
onnectivities') ;
#50369 = UNCERTAINTY_MEASURE_WITH_UNIT(LENGTH_MEASURE(0.001),#50441,
'DISTANCE_ACCURACY_VALUE',
'Maximum model space distance between geometric entities at asserted c
onnectivities') ;
#50370 = UNCERTAINTY_MEASURE_WITH_UNIT(LENGTH_MEASURE(0.001),#50441,
'DISTANCE_ACCURACY_VALUE',
'Maximum model space distance between geometric entities at asserted c
onnectivities') ;
#50371 = UNCERTAINTY_MEASURE_WITH_UNIT(LENGTH_MEASURE(0.001),#50441,
'DISTANCE_ACCURACY_VALUE',
'Maximum model space distance between geometric entities at asserted c
onnectivities') ;
#50372 = UNCERTAINTY_MEASURE_WITH_UNIT(LENGTH_MEASURE(0.001),#50441,
'DISTANCE_ACCURACY_VALUE',
'Maximum model space distance between geometric entities at asserted c
onnectivities') ;
#50373 = UNCERTAINTY_MEASURE_WITH_UNIT(LENGTH_MEASURE(0.001),#50441,
'DISTANCE_ACCURACY_VALUE',
'Maximum model space distance between geometric entities at asserted c
onnectivities') ;
#50374 = UNCERTAINTY_MEASURE_WITH_UNIT(LENGTH_MEASURE(0.001),#50441,
'DISTANCE_ACCURACY_VALUE',
'Maximum model space distance between geometric entities at asserted c
onnectivities') ;
#50375 = UNCERTAINTY_MEASURE_WITH_UNIT(LENGTH_MEASURE(0.001),#50441,
'DISTANCE_ACCURACY_VALUE',
'Maximum model space distance between geometric entities at asserted c
onnectivities') ;
#50376 = UNCERTAINTY_MEASURE_WITH_UNIT(LENGTH_MEASURE(0.001),#50441,
'DISTANCE_ACCURACY_VALUE',
'Maximum model space distance between geometric entities at asserted c
onnectivities') ;
#50377 = UNCERTAINTY_MEASURE_WITH_UNIT(LENGTH_MEASURE(0.001),#50441,
'DISTANCE_ACCURACY_VALUE',
'Maximum model space distance between geometric entities at asserted c
onnectivities') ;
#50378 = UNCERTAINTY_MEASURE_WITH_UNIT(LENGTH_MEASURE(0.001),#50441,
'DISTANCE_ACCURACY_VALUE',
'Maximum model space distance between geometric entities at asserted c
onnectivities') ;
#50379 = UNCERTAINTY_MEASURE_WITH_UNIT(LENGTH_MEASURE(0.001),#50441,
'DISTANCE_ACCURACY_VALUE',
'Maximum model space distance between geometric entities at asserted c
onnectivities') ;
#50380 = UNCERTAINTY_MEASURE_WITH_UNIT(LENGTH_MEASURE(0.001),#50441,
'DISTANCE_ACCURACY_VALUE',
'Maximum model space distance between geometric entities at asserted c
onnectivities') ;
#50381 = UNCERTAINTY_MEASURE_WITH_UNIT(LENGTH_MEASURE(0.001),#50441,
'DISTANCE_ACCURACY_VALUE',
'Maximum model space distance between geometric entities at asserted c
onnectivities') ;
#50382 = UNCERTAINTY_MEASURE_WITH_UNIT(LENGTH_MEASURE(0.001),#50441,
'DISTANCE_ACCURACY_VALUE',
'Maximum model space distance between geometric entities at asserted c
onnectivities') ;
#50383 = UNCERTAINTY_MEASURE_WITH_UNIT(LENGTH_MEASURE(0.001),#50441,
'DISTANCE_ACCURACY_VALUE',
'Maximum model space distance between geometric entities at asserted c
onnectivities') ;
#50384 = UNCERTAINTY_MEASURE_WITH_UNIT(LENGTH_MEASURE(0.001),#50441,
'DISTANCE_ACCURACY_VALUE',
'Maximum model space distance between geometric entities at asserted c
onnectivities') ;
#50385 = UNCERTAINTY_MEASURE_WITH_UNIT(LENGTH_MEASURE(0.001),#50441,
'DISTANCE_ACCURACY_VALUE',
'Maximum model space distance between geometric entities at asserted c
onnectivities') ;
#50386 = UNCERTAINTY_MEASURE_WITH_UNIT(LENGTH_MEASURE(0.001),#50441,
'DISTANCE_ACCURACY_VALUE',
'Maximum model space distance between geometric entities at asserted c
onnectivities') ;
#50387 = UNCERTAINTY_MEASURE_WITH_UNIT(LENGTH_MEASURE(0.001),#50441,
'DISTANCE_ACCURACY_VALUE',
'Maximum model space distance between geometric entities at asserted c
onnectivities') ;
#50388 = (
GEOMETRIC_REPRESENTATION_CONTEXT(3)
GLOBAL_UNCERTAINTY_ASSIGNED_CONTEXT((#50335))
GLOBAL_UNIT_ASSIGNED_CONTEXT((#50441,#50443,#50444))
REPRESENTATION_CONTEXT('','3D')
) ;
#50389 = (
GEOMETRIC_REPRESENTATION_CONTEXT(3)
GLOBAL_UNCERTAINTY_ASSIGNED_CONTEXT((#50336))
GLOBAL_UNIT_ASSIGNED_CONTEXT((#50441,#50443,#50444))
REPRESENTATION_CONTEXT('','3D')
) ;
#50390 = (
GEOMETRIC_REPRESENTATION_CONTEXT(3)
GLOBAL_UNCERTAINTY_ASSIGNED_CONTEXT((#50337))
GLOBAL_UNIT_ASSIGNED_CONTEXT((#50441,#50443,#50444))
REPRESENTATION_CONTEXT('','3D')
) ;
#50391 = (
GEOMETRIC_REPRESENTATION_CONTEXT(3)
GLOBAL_UNCERTAINTY_ASSIGNED_CONTEXT((#50338))
GLOBAL_UNIT_ASSIGNED_CONTEXT((#50441,#50443,#50444))
REPRESENTATION_CONTEXT('','3D')
) ;
#50392 = (
GEOMETRIC_REPRESENTATION_CONTEXT(3)
GLOBAL_UNCERTAINTY_ASSIGNED_CONTEXT((#50339))
GLOBAL_UNIT_ASSIGNED_CONTEXT((#50441,#50443,#50444))
REPRESENTATION_CONTEXT('','3D')
) ;
#50393 = (
GEOMETRIC_REPRESENTATION_CONTEXT(3)
GLOBAL_UNCERTAINTY_ASSIGNED_CONTEXT((#50340))
GLOBAL_UNIT_ASSIGNED_CONTEXT((#50441,#50443,#50444))
REPRESENTATION_CONTEXT('','3D')
) ;
#50394 = (
GEOMETRIC_REPRESENTATION_CONTEXT(3)
GLOBAL_UNCERTAINTY_ASSIGNED_CONTEXT((#50341))
GLOBAL_UNIT_ASSIGNED_CONTEXT((#50441,#50443,#50444))
REPRESENTATION_CONTEXT('','3D')
) ;
#50395 = (
GEOMETRIC_REPRESENTATION_CONTEXT(3)
GLOBAL_UNCERTAINTY_ASSIGNED_CONTEXT((#50342))
GLOBAL_UNIT_ASSIGNED_CONTEXT((#50441,#50443,#50444))
REPRESENTATION_CONTEXT('','3D')
) ;
#50396 = (
GEOMETRIC_REPRESENTATION_CONTEXT(3)
GLOBAL_UNCERTAINTY_ASSIGNED_CONTEXT((#50343))
GLOBAL_UNIT_ASSIGNED_CONTEXT((#50441,#50443,#50444))
REPRESENTATION_CONTEXT('','3D')
) ;
#50397 = (
GEOMETRIC_REPRESENTATION_CONTEXT(3)
GLOBAL_UNCERTAINTY_ASSIGNED_CONTEXT((#50344))
GLOBAL_UNIT_ASSIGNED_CONTEXT((#50441,#50443,#50444))
REPRESENTATION_CONTEXT('','3D')
) ;
#50398 = (
GEOMETRIC_REPRESENTATION_CONTEXT(3)
GLOBAL_UNCERTAINTY_ASSIGNED_CONTEXT((#50345))
GLOBAL_UNIT_ASSIGNED_CONTEXT((#50441,#50443,#50444))
REPRESENTATION_CONTEXT('','3D')
) ;
#50399 = (
GEOMETRIC_REPRESENTATION_CONTEXT(3)
GLOBAL_UNCERTAINTY_ASSIGNED_CONTEXT((#50346))
GLOBAL_UNIT_ASSIGNED_CONTEXT((#50441,#50443,#50444))
REPRESENTATION_CONTEXT('','3D')
) ;
#50400 = (
GEOMETRIC_REPRESENTATION_CONTEXT(3)
GLOBAL_UNCERTAINTY_ASSIGNED_CONTEXT((#50347))
GLOBAL_UNIT_ASSIGNED_CONTEXT((#50441,#50443,#50444))
REPRESENTATION_CONTEXT('','3D')
) ;
#50401 = (
GEOMETRIC_REPRESENTATION_CONTEXT(3)
GLOBAL_UNCERTAINTY_ASSIGNED_CONTEXT((#50348))
GLOBAL_UNIT_ASSIGNED_CONTEXT((#50441,#50443,#50444))
REPRESENTATION_CONTEXT('','3D')
) ;
#50402 = (
GEOMETRIC_REPRESENTATION_CONTEXT(3)
GLOBAL_UNCERTAINTY_ASSIGNED_CONTEXT((#50349))
GLOBAL_UNIT_ASSIGNED_CONTEXT((#50441,#50443,#50444))
REPRESENTATION_CONTEXT('','3D')
) ;
#50403 = (
GEOMETRIC_REPRESENTATION_CONTEXT(3)
GLOBAL_UNCERTAINTY_ASSIGNED_CONTEXT((#50350))
GLOBAL_UNIT_ASSIGNED_CONTEXT((#50441,#50443,#50444))
REPRESENTATION_CONTEXT('','3D')
) ;
#50404 = (
GEOMETRIC_REPRESENTATION_CONTEXT(3)
GLOBAL_UNCERTAINTY_ASSIGNED_CONTEXT((#50351))
GLOBAL_UNIT_ASSIGNED_CONTEXT((#50441,#50443,#50444))
REPRESENTATION_CONTEXT('','3D')
) ;
#50405 = (
GEOMETRIC_REPRESENTATION_CONTEXT(3)
GLOBAL_UNCERTAINTY_ASSIGNED_CONTEXT((#50352))
GLOBAL_UNIT_ASSIGNED_CONTEXT((#50441,#50443,#50444))
REPRESENTATION_CONTEXT('','3D')
) ;
#50406 = (
GEOMETRIC_REPRESENTATION_CONTEXT(3)
GLOBAL_UNCERTAINTY_ASSIGNED_CONTEXT((#50353))
GLOBAL_UNIT_ASSIGNED_CONTEXT((#50441,#50443,#50444))
REPRESENTATION_CONTEXT('','3D')
) ;
#50407 = (
GEOMETRIC_REPRESENTATION_CONTEXT(3)
GLOBAL_UNCERTAINTY_ASSIGNED_CONTEXT((#50354))
GLOBAL_UNIT_ASSIGNED_CONTEXT((#50441,#50443,#50444))
REPRESENTATION_CONTEXT('','3D')
) ;
#50408 = (
GEOMETRIC_REPRESENTATION_CONTEXT(3)
GLOBAL_UNCERTAINTY_ASSIGNED_CONTEXT((#50355))
GLOBAL_UNIT_ASSIGNED_CONTEXT((#50441,#50443,#50444))
REPRESENTATION_CONTEXT('','3D')
) ;
#50409 = (
GEOMETRIC_REPRESENTATION_CONTEXT(3)
GLOBAL_UNCERTAINTY_ASSIGNED_CONTEXT((#50356))
GLOBAL_UNIT_ASSIGNED_CONTEXT((#50441,#50443,#50444))
REPRESENTATION_CONTEXT('','3D')
) ;
#50410 = (
GEOMETRIC_REPRESENTATION_CONTEXT(3)
GLOBAL_UNCERTAINTY_ASSIGNED_CONTEXT((#50357))
GLOBAL_UNIT_ASSIGNED_CONTEXT((#50441,#50443,#50444))
REPRESENTATION_CONTEXT('','3D')
) ;
#50411 = (
GEOMETRIC_REPRESENTATION_CONTEXT(3)
GLOBAL_UNCERTAINTY_ASSIGNED_CONTEXT((#50358))
GLOBAL_UNIT_ASSIGNED_CONTEXT((#50441,#50443,#50444))
REPRESENTATION_CONTEXT('','3D')
) ;
#50412 = (
GEOMETRIC_REPRESENTATION_CONTEXT(3)
GLOBAL_UNCERTAINTY_ASSIGNED_CONTEXT((#50359))
GLOBAL_UNIT_ASSIGNED_CONTEXT((#50441,#50443,#50444))
REPRESENTATION_CONTEXT('','3D')
) ;
#50413 = (
GEOMETRIC_REPRESENTATION_CONTEXT(3)
GLOBAL_UNCERTAINTY_ASSIGNED_CONTEXT((#50360))
GLOBAL_UNIT_ASSIGNED_CONTEXT((#50441,#50443,#50444))
REPRESENTATION_CONTEXT('','3D')
) ;
#50414 = (
GEOMETRIC_REPRESENTATION_CONTEXT(3)
GLOBAL_UNCERTAINTY_ASSIGNED_CONTEXT((#50361))
GLOBAL_UNIT_ASSIGNED_CONTEXT((#50441,#50443,#50444))
REPRESENTATION_CONTEXT('','3D')
) ;
#50415 = (
GEOMETRIC_REPRESENTATION_CONTEXT(3)
GLOBAL_UNCERTAINTY_ASSIGNED_CONTEXT((#50362))
GLOBAL_UNIT_ASSIGNED_CONTEXT((#50441,#50443,#50444))
REPRESENTATION_CONTEXT('','3D')
) ;
#50416 = (
GEOMETRIC_REPRESENTATION_CONTEXT(3)
GLOBAL_UNCERTAINTY_ASSIGNED_CONTEXT((#50363))
GLOBAL_UNIT_ASSIGNED_CONTEXT((#50441,#50443,#50444))
REPRESENTATION_CONTEXT('','3D')
) ;
#50417 = (
GEOMETRIC_REPRESENTATION_CONTEXT(3)
GLOBAL_UNCERTAINTY_ASSIGNED_CONTEXT((#50364))
GLOBAL_UNIT_ASSIGNED_CONTEXT((#50441,#50443,#50444))
REPRESENTATION_CONTEXT('','3D')
) ;
#50418 = (
GEOMETRIC_REPRESENTATION_CONTEXT(3)
GLOBAL_UNCERTAINTY_ASSIGNED_CONTEXT((#50365))
GLOBAL_UNIT_ASSIGNED_CONTEXT((#50441,#50443,#50444))
REPRESENTATION_CONTEXT('','3D')
) ;
#50419 = (
GEOMETRIC_REPRESENTATION_CONTEXT(3)
GLOBAL_UNCERTAINTY_ASSIGNED_CONTEXT((#50366))
GLOBAL_UNIT_ASSIGNED_CONTEXT((#50441,#50443,#50444))
REPRESENTATION_CONTEXT('','3D')
) ;
#50420 = (
GEOMETRIC_REPRESENTATION_CONTEXT(3)
GLOBAL_UNCERTAINTY_ASSIGNED_CONTEXT((#50367))
GLOBAL_UNIT_ASSIGNED_CONTEXT((#50441,#50443,#50444))
REPRESENTATION_CONTEXT('','3D')
) ;
#50421 = (
GEOMETRIC_REPRESENTATION_CONTEXT(3)
GLOBAL_UNCERTAINTY_ASSIGNED_CONTEXT((#50368))
GLOBAL_UNIT_ASSIGNED_CONTEXT((#50441,#50443,#50444))
REPRESENTATION_CONTEXT('','3D')
) ;
#50422 = (
GEOMETRIC_REPRESENTATION_CONTEXT(3)
GLOBAL_UNCERTAINTY_ASSIGNED_CONTEXT((#50369))
GLOBAL_UNIT_ASSIGNED_CONTEXT((#50441,#50443,#50444))
REPRESENTATION_CONTEXT('','3D')
) ;
#50423 = (
GEOMETRIC_REPRESENTATION_CONTEXT(3)
GLOBAL_UNCERTAINTY_ASSIGNED_CONTEXT((#50370))
GLOBAL_UNIT_ASSIGNED_CONTEXT((#50441,#50443,#50444))
REPRESENTATION_CONTEXT('','3D')
) ;
#50424 = (
GEOMETRIC_REPRESENTATION_CONTEXT(3)
GLOBAL_UNCERTAINTY_ASSIGNED_CONTEXT((#50371))
GLOBAL_UNIT_ASSIGNED_CONTEXT((#50441,#50443,#50444))
REPRESENTATION_CONTEXT('','3D')
) ;
#50425 = (
GEOMETRIC_REPRESENTATION_CONTEXT(3)
GLOBAL_UNCERTAINTY_ASSIGNED_CONTEXT((#50372))
GLOBAL_UNIT_ASSIGNED_CONTEXT((#50441,#50443,#50444))
REPRESENTATION_CONTEXT('','3D')
) ;
#50426 = (
GEOMETRIC_REPRESENTATION_CONTEXT(3)
GLOBAL_UNCERTAINTY_ASSIGNED_CONTEXT((#50373))
GLOBAL_UNIT_ASSIGNED_CONTEXT((#50441,#50443,#50444))
REPRESENTATION_CONTEXT('','3D')
) ;
#50427 = (
GEOMETRIC_REPRESENTATION_CONTEXT(3)
GLOBAL_UNCERTAINTY_ASSIGNED_CONTEXT((#50374))
GLOBAL_UNIT_ASSIGNED_CONTEXT((#50441,#50443,#50444))
REPRESENTATION_CONTEXT('','3D')
) ;
#50428 = (
GEOMETRIC_REPRESENTATION_CONTEXT(3)
GLOBAL_UNCERTAINTY_ASSIGNED_CONTEXT((#50375))
GLOBAL_UNIT_ASSIGNED_CONTEXT((#50441,#50443,#50444))
REPRESENTATION_CONTEXT('','3D')
) ;
#50429 = (
GEOMETRIC_REPRESENTATION_CONTEXT(3)
GLOBAL_UNCERTAINTY_ASSIGNED_CONTEXT((#50376))
GLOBAL_UNIT_ASSIGNED_CONTEXT((#50441,#50443,#50444))
REPRESENTATION_CONTEXT('','3D')
) ;
#50430 = (
GEOMETRIC_REPRESENTATION_CONTEXT(3)
GLOBAL_UNCERTAINTY_ASSIGNED_CONTEXT((#50377))
GLOBAL_UNIT_ASSIGNED_CONTEXT((#50441,#50443,#50444))
REPRESENTATION_CONTEXT('','3D')
) ;
#50431 = (
GEOMETRIC_REPRESENTATION_CONTEXT(3)
GLOBAL_UNCERTAINTY_ASSIGNED_CONTEXT((#50378))
GLOBAL_UNIT_ASSIGNED_CONTEXT((#50441,#50443,#50444))
REPRESENTATION_CONTEXT('','3D')
) ;
#50432 = (
GEOMETRIC_REPRESENTATION_CONTEXT(3)
GLOBAL_UNCERTAINTY_ASSIGNED_CONTEXT((#50379))
GLOBAL_UNIT_ASSIGNED_CONTEXT((#50441,#50443,#50444))
REPRESENTATION_CONTEXT('','3D')
) ;
#50433 = (
GEOMETRIC_REPRESENTATION_CONTEXT(3)
GLOBAL_UNCERTAINTY_ASSIGNED_CONTEXT((#50380))
GLOBAL_UNIT_ASSIGNED_CONTEXT((#50441,#50443,#50444))
REPRESENTATION_CONTEXT('','3D')
) ;
#50434 = (
GEOMETRIC_REPRESENTATION_CONTEXT(3)
GLOBAL_UNCERTAINTY_ASSIGNED_CONTEXT((#50381))
GLOBAL_UNIT_ASSIGNED_CONTEXT((#50441,#50443,#50444))
REPRESENTATION_CONTEXT('','3D')
) ;
#50435 = (
GEOMETRIC_REPRESENTATION_CONTEXT(3)
GLOBAL_UNCERTAINTY_ASSIGNED_CONTEXT((#50382))
GLOBAL_UNIT_ASSIGNED_CONTEXT((#50441,#50443,#50444))
REPRESENTATION_CONTEXT('','3D')
) ;
#50436 = (
GEOMETRIC_REPRESENTATION_CONTEXT(3)
GLOBAL_UNCERTAINTY_ASSIGNED_CONTEXT((#50383))
GLOBAL_UNIT_ASSIGNED_CONTEXT((#50441,#50443,#50444))
REPRESENTATION_CONTEXT('','3D')
) ;
#50437 = (
GEOMETRIC_REPRESENTATION_CONTEXT(3)
GLOBAL_UNCERTAINTY_ASSIGNED_CONTEXT((#50384))
GLOBAL_UNIT_ASSIGNED_CONTEXT((#50441,#50443,#50444))
REPRESENTATION_CONTEXT('','3D')
) ;
#50438 = (
GEOMETRIC_REPRESENTATION_CONTEXT(3)
GLOBAL_UNCERTAINTY_ASSIGNED_CONTEXT((#50385))
GLOBAL_UNIT_ASSIGNED_CONTEXT((#50441,#50443,#50444))
REPRESENTATION_CONTEXT('','3D')
) ;
#50439 = (
GEOMETRIC_REPRESENTATION_CONTEXT(3)
GLOBAL_UNCERTAINTY_ASSIGNED_CONTEXT((#50386))
GLOBAL_UNIT_ASSIGNED_CONTEXT((#50441,#50443,#50444))
REPRESENTATION_CONTEXT('','3D')
) ;
#50440 = (
GEOMETRIC_REPRESENTATION_CONTEXT(3)
GLOBAL_UNCERTAINTY_ASSIGNED_CONTEXT((#50387))
GLOBAL_UNIT_ASSIGNED_CONTEXT((#50441,#50443,#50444))
REPRESENTATION_CONTEXT('','3D')
) ;
#50441 = (
LENGTH_UNIT()
NAMED_UNIT(*)
SI_UNIT(.CENTI.,.METRE.)
) ;
#50442 = (
LENGTH_UNIT()
NAMED_UNIT(*)
SI_UNIT($,.METRE.)
) ;
#50443 = (
NAMED_UNIT(*)
PLANE_ANGLE_UNIT()
SI_UNIT($,.RADIAN.)
) ;
#50444 = (
NAMED_UNIT(*)
SI_UNIT($,.STERADIAN.)
SOLID_ANGLE_UNIT()
) ;
#50445 = SHAPE_DEFINITION_REPRESENTATION(#50497,#50619) ;
#50446 = SHAPE_DEFINITION_REPRESENTATION(#50498,#50620) ;
#50447 = SHAPE_DEFINITION_REPRESENTATION(#50499,#50621) ;
#50448 = SHAPE_DEFINITION_REPRESENTATION(#50500,#50622) ;
#50449 = SHAPE_DEFINITION_REPRESENTATION(#50501,#50623) ;
#50450 = SHAPE_DEFINITION_REPRESENTATION(#50502,#50624) ;
#50451 = SHAPE_DEFINITION_REPRESENTATION(#50503,#50625) ;
#50452 = SHAPE_DEFINITION_REPRESENTATION(#50510,#50626) ;
#50453 = SHAPE_DEFINITION_REPRESENTATION(#50511,#50627) ;
#50454 = SHAPE_DEFINITION_REPRESENTATION(#50512,#50628) ;
#50455 = SHAPE_DEFINITION_REPRESENTATION(#50513,#50629) ;
#50456 = SHAPE_DEFINITION_REPRESENTATION(#50514,#50630) ;
#50457 = SHAPE_DEFINITION_REPRESENTATION(#50523,#50631) ;
#50458 = SHAPE_DEFINITION_REPRESENTATION(#50524,#50632) ;
#50459 = SHAPE_DEFINITION_REPRESENTATION(#50525,#50633) ;
#50460 = SHAPE_DEFINITION_REPRESENTATION(#50526,#50634) ;
#50461 = SHAPE_DEFINITION_REPRESENTATION(#50527,#50635) ;
#50462 = SHAPE_DEFINITION_REPRESENTATION(#50528,#50636) ;
#50463 = SHAPE_DEFINITION_REPRESENTATION(#50529,#50637) ;
#50464 = SHAPE_DEFINITION_REPRESENTATION(#50530,#50638) ;
#50465 = SHAPE_DEFINITION_REPRESENTATION(#50531,#50639) ;
#50466 = SHAPE_DEFINITION_REPRESENTATION(#50532,#50640) ;
#50467 = SHAPE_DEFINITION_REPRESENTATION(#50533,#50641) ;
#50468 = SHAPE_DEFINITION_REPRESENTATION(#50544,#50642) ;
#50469 = SHAPE_DEFINITION_REPRESENTATION(#50545,#50643) ;
#50470 = SHAPE_DEFINITION_REPRESENTATION(#50546,#50644) ;
#50471 = SHAPE_DEFINITION_REPRESENTATION(#50547,#50645) ;
#50472 = SHAPE_DEFINITION_REPRESENTATION(#50548,#50646) ;
#50473 = SHAPE_DEFINITION_REPRESENTATION(#50549,#50647) ;
#50474 = SHAPE_DEFINITION_REPRESENTATION(#50550,#50648) ;
#50475 = SHAPE_DEFINITION_REPRESENTATION(#50551,#50649) ;
#50476 = SHAPE_DEFINITION_REPRESENTATION(#50552,#50650) ;
#50477 = SHAPE_DEFINITION_REPRESENTATION(#50553,#50651) ;
#50478 = SHAPE_DEFINITION_REPRESENTATION(#50554,#50652) ;
#50479 = SHAPE_DEFINITION_REPRESENTATION(#50555,#50653) ;
#50480 = SHAPE_DEFINITION_REPRESENTATION(#50556,#50654) ;
#50481 = SHAPE_DEFINITION_REPRESENTATION(#50557,#50655) ;
#50482 = SHAPE_DEFINITION_REPRESENTATION(#50558,#50656) ;
#50483 = SHAPE_DEFINITION_REPRESENTATION(#50573,#50657) ;
#50484 = SHAPE_DEFINITION_REPRESENTATION(#50574,#50658) ;
#50485 = SHAPE_DEFINITION_REPRESENTATION(#50575,#50659) ;
#50486 = SHAPE_DEFINITION_REPRESENTATION(#50576,#50660) ;
#50487 = SHAPE_DEFINITION_REPRESENTATION(#50577,#50661) ;
#50488 = SHAPE_DEFINITION_REPRESENTATION(#50578,#50662) ;
#50489 = SHAPE_DEFINITION_REPRESENTATION(#50585,#50663) ;
#50490 = SHAPE_DEFINITION_REPRESENTATION(#50586,#50664) ;
#50491 = SHAPE_DEFINITION_REPRESENTATION(#50587,#50665) ;
#50492 = SHAPE_DEFINITION_REPRESENTATION(#50588,#50666) ;
#50493 = SHAPE_DEFINITION_REPRESENTATION(#50589,#50667) ;
#50494 = SHAPE_DEFINITION_REPRESENTATION(#50590,#50668) ;
#50495 = SHAPE_DEFINITION_REPRESENTATION(#50591,#50669) ;
#50496 = SHAPE_DEFINITION_REPRESENTATION(#50592,#50670) ;
#50497 = PRODUCT_DEFINITION_SHAPE('',$,#50672) ;
#50498 = PRODUCT_DEFINITION_SHAPE('',$,#50673) ;
#50499 = PRODUCT_DEFINITION_SHAPE('',$,#50674) ;
#50500 = PRODUCT_DEFINITION_SHAPE('',$,#50675) ;
#50501 = PRODUCT_DEFINITION_SHAPE('',$,#50676) ;
#50502 = PRODUCT_DEFINITION_SHAPE('',$,#50677) ;
#50503 = PRODUCT_DEFINITION_SHAPE('',$,#50678) ;
#50504 = PRODUCT_DEFINITION_SHAPE($,$,#292) ;
#50505 = PRODUCT_DEFINITION_SHAPE($,$,#293) ;
#50506 = PRODUCT_DEFINITION_SHAPE($,$,#294) ;
#50507 = PRODUCT_DEFINITION_SHAPE($,$,#295) ;
#50508 = PRODUCT_DEFINITION_SHAPE($,$,#296) ;
#50509 = PRODUCT_DEFINITION_SHAPE($,$,#297) ;
#50510 = PRODUCT_DEFINITION_SHAPE('',$,#50679) ;
#50511 = PRODUCT_DEFINITION_SHAPE('',$,#50680) ;
#50512 = PRODUCT_DEFINITION_SHAPE('',$,#50681) ;
#50513 = PRODUCT_DEFINITION_SHAPE('',$,#50682) ;
#50514 = PRODUCT_DEFINITION_SHAPE('',$,#50683) ;
#50515 = PRODUCT_DEFINITION_SHAPE($,$,#298) ;
#50516 = PRODUCT_DEFINITION_SHAPE($,$,#299) ;
#50517 = PRODUCT_DEFINITION_SHAPE($,$,#300) ;
#50518 = PRODUCT_DEFINITION_SHAPE($,$,#301) ;
#50519 = PRODUCT_DEFINITION_SHAPE($,$,#302) ;
#50520 = PRODUCT_DEFINITION_SHAPE($,$,#303) ;
#50521 = PRODUCT_DEFINITION_SHAPE($,$,#304) ;
#50522 = PRODUCT_DEFINITION_SHAPE($,$,#305) ;
#50523 = PRODUCT_DEFINITION_SHAPE('',$,#50684) ;
#50524 = PRODUCT_DEFINITION_SHAPE('',$,#50685) ;
#50525 = PRODUCT_DEFINITION_SHAPE('',$,#50686) ;
#50526 = PRODUCT_DEFINITION_SHAPE('',$,#50687) ;
#50527 = PRODUCT_DEFINITION_SHAPE('',$,#50688) ;
#50528 = PRODUCT_DEFINITION_SHAPE('',$,#50689) ;
#50529 = PRODUCT_DEFINITION_SHAPE('',$,#50690) ;
#50530 = PRODUCT_DEFINITION_SHAPE('',$,#50691) ;
#50531 = PRODUCT_DEFINITION_SHAPE('',$,#50692) ;
#50532 = PRODUCT_DEFINITION_SHAPE('',$,#50693) ;
#50533 = PRODUCT_DEFINITION_SHAPE('',$,#50694) ;
#50534 = PRODUCT_DEFINITION_SHAPE($,$,#306) ;
#50535 = PRODUCT_DEFINITION_SHAPE($,$,#307) ;
#50536 = PRODUCT_DEFINITION_SHAPE($,$,#308) ;
#50537 = PRODUCT_DEFINITION_SHAPE($,$,#309) ;
#50538 = PRODUCT_DEFINITION_SHAPE($,$,#310) ;
#50539 = PRODUCT_DEFINITION_SHAPE($,$,#311) ;
#50540 = PRODUCT_DEFINITION_SHAPE($,$,#312) ;
#50541 = PRODUCT_DEFINITION_SHAPE($,$,#313) ;
#50542 = PRODUCT_DEFINITION_SHAPE($,$,#314) ;
#50543 = PRODUCT_DEFINITION_SHAPE($,$,#315) ;
#50544 = PRODUCT_DEFINITION_SHAPE('',$,#50695) ;
#50545 = PRODUCT_DEFINITION_SHAPE('',$,#50696) ;
#50546 = PRODUCT_DEFINITION_SHAPE('',$,#50697) ;
#50547 = PRODUCT_DEFINITION_SHAPE('',$,#50698) ;
#50548 = PRODUCT_DEFINITION_SHAPE('',$,#50699) ;
#50549 = PRODUCT_DEFINITION_SHAPE('',$,#50700) ;
#50550 = PRODUCT_DEFINITION_SHAPE('',$,#50701) ;
#50551 = PRODUCT_DEFINITION_SHAPE('',$,#50702) ;
#50552 = PRODUCT_DEFINITION_SHAPE('',$,#50703) ;
#50553 = PRODUCT_DEFINITION_SHAPE('',$,#50704) ;
#50554 = PRODUCT_DEFINITION_SHAPE('',$,#50705) ;
#50555 = PRODUCT_DEFINITION_SHAPE('',$,#50706) ;
#50556 = PRODUCT_DEFINITION_SHAPE('',$,#50707) ;
#50557 = PRODUCT_DEFINITION_SHAPE('',$,#50708) ;
#50558 = PRODUCT_DEFINITION_SHAPE('',$,#50709) ;
#50559 = PRODUCT_DEFINITION_SHAPE($,$,#316) ;
#50560 = PRODUCT_DEFINITION_SHAPE($,$,#317) ;
#50561 = PRODUCT_DEFINITION_SHAPE($,$,#318) ;
#50562 = PRODUCT_DEFINITION_SHAPE($,$,#319) ;
#50563 = PRODUCT_DEFINITION_SHAPE($,$,#320) ;
#50564 = PRODUCT_DEFINITION_SHAPE($,$,#321) ;
#50565 = PRODUCT_DEFINITION_SHAPE($,$,#322) ;
#50566 = PRODUCT_DEFINITION_SHAPE($,$,#323) ;
#50567 = PRODUCT_DEFINITION_SHAPE($,$,#324) ;
#50568 = PRODUCT_DEFINITION_SHAPE($,$,#325) ;
#50569 = PRODUCT_DEFINITION_SHAPE($,$,#326) ;
#50570 = PRODUCT_DEFINITION_SHAPE($,$,#327) ;
#50571 = PRODUCT_DEFINITION_SHAPE($,$,#328) ;
#50572 = PRODUCT_DEFINITION_SHAPE($,$,#329) ;
#50573 = PRODUCT_DEFINITION_SHAPE('',$,#50710) ;
#50574 = PRODUCT_DEFINITION_SHAPE('',$,#50711) ;
#50575 = PRODUCT_DEFINITION_SHAPE('',$,#50712) ;
#50576 = PRODUCT_DEFINITION_SHAPE('',$,#50713) ;
#50577 = PRODUCT_DEFINITION_SHAPE('',$,#50714) ;
#50578 = PRODUCT_DEFINITION_SHAPE('',$,#50715) ;
#50579 = PRODUCT_DEFINITION_SHAPE($,$,#330) ;
#50580 = PRODUCT_DEFINITION_SHAPE($,$,#331) ;
#50581 = PRODUCT_DEFINITION_SHAPE($,$,#332) ;
#50582 = PRODUCT_DEFINITION_SHAPE($,$,#333) ;
#50583 = PRODUCT_DEFINITION_SHAPE($,$,#334) ;
#50584 = PRODUCT_DEFINITION_SHAPE($,$,#335) ;
#50585 = PRODUCT_DEFINITION_SHAPE('',$,#50716) ;
#50586 = PRODUCT_DEFINITION_SHAPE('',$,#50717) ;
#50587 = PRODUCT_DEFINITION_SHAPE('',$,#50718) ;
#50588 = PRODUCT_DEFINITION_SHAPE('',$,#50719) ;
#50589 = PRODUCT_DEFINITION_SHAPE('',$,#50720) ;
#50590 = PRODUCT_DEFINITION_SHAPE('',$,#50721) ;
#50591 = PRODUCT_DEFINITION_SHAPE('',$,#50722) ;
#50592 = PRODUCT_DEFINITION_SHAPE('',$,#50723) ;
#50593 = PRODUCT_DEFINITION_SHAPE($,$,#336) ;
#50594 = PRODUCT_DEFINITION_SHAPE($,$,#337) ;
#50595 = PRODUCT_DEFINITION_SHAPE($,$,#338) ;
#50596 = PRODUCT_DEFINITION_SHAPE($,$,#339) ;
#50597 = PRODUCT_DEFINITION_SHAPE($,$,#340) ;
#50598 = PRODUCT_DEFINITION_SHAPE($,$,#341) ;
#50599 = PRODUCT_DEFINITION_SHAPE($,$,#342) ;
#50600 = PRODUCT_DEFINITION_SHAPE($,$,#343) ;
#50601 = PRODUCT_DEFINITION_SHAPE($,$,#344) ;
#50602 = PRODUCT_DEFINITION_SHAPE($,$,#345) ;
#50603 = PRODUCT_DEFINITION_SHAPE($,$,#346) ;
#50604 = PRODUCT_DEFINITION_SHAPE($,$,#347) ;
#50605 = PRODUCT_DEFINITION_SHAPE($,$,#348) ;
#50606 = PRODUCT_DEFINITION_SHAPE($,$,#349) ;
#50607 = PRODUCT_DEFINITION_SHAPE($,$,#350) ;
#50608 = PRODUCT_DEFINITION_SHAPE($,$,#351) ;
#50609 = PRODUCT_DEFINITION_SHAPE($,$,#352) ;
#50610 = PRODUCT_DEFINITION_SHAPE($,$,#353) ;
#50611 = PRODUCT_DEFINITION_SHAPE($,$,#354) ;
#50612 = PRODUCT_DEFINITION_SHAPE($,$,#355) ;
#50613 = PRODUCT_DEFINITION_SHAPE($,$,#356) ;
#50614 = PRODUCT_DEFINITION_SHAPE($,$,#357) ;
#50615 = PRODUCT_DEFINITION_SHAPE($,$,#358) ;
#50616 = PRODUCT_DEFINITION_SHAPE($,$,#359) ;
#50617 = PRODUCT_DEFINITION_SHAPE($,$,#360) ;
#50618 = PRODUCT_DEFINITION_SHAPE($,$,#361) ;
#50619 = SHAPE_REPRESENTATION('',(#29211,#32385,#32386,#32387,#32388,#32389,
#32390),#50388) ;
#50620 = SHAPE_REPRESENTATION('',(#29212,#29914,#29915,#29916,#29917,#29918,
#29919),#50389) ;
#50621 = SHAPE_REPRESENTATION('',(#29213),#50390) ;
#50622 = SHAPE_REPRESENTATION('',(#29312),#50391) ;
#50623 = SHAPE_REPRESENTATION('',(#29330),#50392) ;
#50624 = SHAPE_REPRESENTATION('',(#29339),#50393) ;
#50625 = SHAPE_REPRESENTATION('',(#29730),#50394) ;
#50626 = SHAPE_REPRESENTATION('',(#29920,#30275,#30276,#30277,#30278,#30279,
#30280,#30281,#30282),#50395) ;
#50627 = SHAPE_REPRESENTATION('',(#29921),#50396) ;
#50628 = SHAPE_REPRESENTATION('',(#30246),#50397) ;
#50629 = SHAPE_REPRESENTATION('',(#30253),#50398) ;
#50630 = SHAPE_REPRESENTATION('',(#30264),#50399) ;
#50631 = SHAPE_REPRESENTATION('',(#30283,#30663,#30664,#30665,#30666,#30667,
#30668,#30669,#30670,#30671,#30672),#50400) ;
#50632 = SHAPE_REPRESENTATION('',(#30284),#50401) ;
#50633 = SHAPE_REPRESENTATION('',(#30394),#50402) ;
#50634 = SHAPE_REPRESENTATION('',(#30407),#50403) ;
#50635 = SHAPE_REPRESENTATION('',(#30509),#50404) ;
#50636 = SHAPE_REPRESENTATION('',(#30518),#50405) ;
#50637 = SHAPE_REPRESENTATION('',(#30539),#50406) ;
#50638 = SHAPE_REPRESENTATION('',(#30545),#50407) ;
#50639 = SHAPE_REPRESENTATION('',(#30558),#50408) ;
#50640 = SHAPE_REPRESENTATION('',(#30580),#50409) ;
#50641 = SHAPE_REPRESENTATION('',(#30654),#50410) ;
#50642 = SHAPE_REPRESENTATION('',(#30673,#32067,#32068,#32069,#32070,#32071,
#32072,#32073,#32074,#32075,#32076,#32077,#32078,#32079,#32080),#50411) ;
#50643 = SHAPE_REPRESENTATION('',(#30674),#50412) ;
#50644 = SHAPE_REPRESENTATION('',(#30734),#50413) ;
#50645 = SHAPE_REPRESENTATION('',(#30765),#50414) ;
#50646 = SHAPE_REPRESENTATION('',(#30808),#50415) ;
#50647 = SHAPE_REPRESENTATION('',(#30841),#50416) ;
#50648 = SHAPE_REPRESENTATION('',(#30860),#50417) ;
#50649 = SHAPE_REPRESENTATION('',(#30891),#50418) ;
#50650 = SHAPE_REPRESENTATION('',(#30925),#50419) ;
#50651 = SHAPE_REPRESENTATION('',(#30932),#50420) ;
#50652 = SHAPE_REPRESENTATION('',(#30942),#50421) ;
#50653 = SHAPE_REPRESENTATION('',(#31036),#50422) ;
#50654 = SHAPE_REPRESENTATION('',(#31057),#50423) ;
#50655 = SHAPE_REPRESENTATION('',(#31063),#50424) ;
#50656 = SHAPE_REPRESENTATION('',(#31069),#50425) ;
#50657 = SHAPE_REPRESENTATION('',(#32081,#32200,#32201,#32202,#32203,#32204,
#32205),#50426) ;
#50658 = SHAPE_REPRESENTATION('',(#32082),#50427) ;
#50659 = SHAPE_REPRESENTATION('',(#32118),#50428) ;
#50660 = SHAPE_REPRESENTATION('',(#32157),#50429) ;
#50661 = SHAPE_REPRESENTATION('',(#32166),#50430) ;
#50662 = SHAPE_REPRESENTATION('',(#32183),#50431) ;
#50663 = SHAPE_REPRESENTATION('',(#32206,#32365,#32366,#32367,#32368,#32369,
#32370,#32371,#32372,#32373,#32374,#32375,#32376,#32377,#32378,#32379,#32380,
#32381,#32382,#32383,#32384),#50432) ;
#50664 = SHAPE_REPRESENTATION('',(#32207),#50433) ;
#50665 = SHAPE_REPRESENTATION('',(#32220),#50434) ;
#50666 = SHAPE_REPRESENTATION('',(#32232),#50435) ;
#50667 = SHAPE_REPRESENTATION('',(#32245),#50436) ;
#50668 = SHAPE_REPRESENTATION('',(#32257),#50437) ;
#50669 = SHAPE_REPRESENTATION('',(#32267),#50438) ;
#50670 = SHAPE_REPRESENTATION('',(#32277),#50439) ;
#50671 = PRODUCT_DEFINITION_CONTEXT('part definition',#50829,'design') ;
#50672 = PRODUCT_DEFINITION('MAS-603',
'MAS-603',#50724,#50671) ;
#50673 = PRODUCT_DEFINITION('HOPPER_UNIT','HOPPER_UNIT',#50725,
#50671) ;
#50674 = PRODUCT_DEFINITION('CONICAL_POLYETHYLENE_HOPPER',
'CONICAL_POLYETHYLENE_HOPPER',#50726,#50671) ;
#50675 = PRODUCT_DEFINITION('HOPPER_LID','HOPPER_LID',#50727,
#50671) ;
#50676 = PRODUCT_DEFINITION('LID_HINGE_STRAP','LID_HINGE_STRAP',#50728,
#50671) ;
#50677 = PRODUCT_DEFINITION('HOPPER_SIEVE_GRID','HOPPER_SIEVE_GRID',
#50729,#50671) ;
#50678 = PRODUCT_DEFINITION('HOPPER_SUPPORT_RING',
'HOPPER_SUPPORT_RING',#50730,#50671) ;
#50679 = PRODUCT_DEFINITION('HITCH_FRAME_UNIT','HITCH_FRAME_UNIT',
#50731,#50671) ;
#50680 = PRODUCT_DEFINITION('TUBULAR_3POINT_HITCH_FRAME',
'TUBULAR_3POINT_HITCH_FRAME',#50732,#50671) ;
#50681 = PRODUCT_DEFINITION('STAND_FOOT_PLATE','STAND_FOOT_PLATE',
#50733,#50671) ;
#50682 = PRODUCT_DEFINITION('LOWER_LINK_PIN_CAT2',
'LOWER_LINK_PIN_CAT2',#50734,#50671) ;
#50683 = PRODUCT_DEFINITION('TOP_LINK_PIN_CAT2','TOP_LINK_PIN_CAT2',
#50735,#50671) ;
#50684 = PRODUCT_DEFINITION('GEARBOX_DRIVE_UNIT',
'GEARBOX_DRIVE_UNIT',#50736,#50671) ;
#50685 = PRODUCT_DEFINITION('GEARBOX_OSCILLATION_HOUSING',
'GEARBOX_OSCILLATION_HOUSING',#50737,#50671) ;
#50686 = PRODUCT_DEFINITION('GEARBOX_OIL_PLUG','GEARBOX_OIL_PLUG',
#50738,#50671) ;
#50687 = PRODUCT_DEFINITION('PTO_INPUT_SHAFT_SPLINE',
'PTO_INPUT_SHAFT_SPLINE',#50739,#50671) ;
#50688 = PRODUCT_DEFINITION('PTO_SHAFT_SEAL','PTO_SHAFT_SEAL',#50740,
#50671) ;
#50689 = PRODUCT_DEFINITION('PTO_SHIELD_GUARD','PTO_SHIELD_GUARD',
#50741,#50671) ;
#50690 = PRODUCT_DEFINITION('OSCILLATION_OUTPUT_SHAFT',
'OSCILLATION_OUTPUT_SHAFT',#50742,#50671) ;
#50691 = PRODUCT_DEFINITION('OSCILLATION_CRANK_DISC',
'OSCILLATION_CRANK_DISC',#50743,#50671) ;
#50692 = PRODUCT_DEFINITION('CONNECTING_ROD','CONNECTING_ROD',#50744,
#50671) ;
#50693 = PRODUCT_DEFINITION('AGITATOR_SHAFT_ASSEMBLY',
'AGITATOR_SHAFT_ASSEMBLY',#50745,#50671) ;
#50694 = PRODUCT_DEFINITION('AGITATOR_SHAFT_SEAL',
'AGITATOR_SHAFT_SEAL',#50746,#50671) ;
#50695 = PRODUCT_DEFINITION('METERING_GATE_UNIT',
'METERING_GATE_UNIT',#50747,#50671) ;
#50696 = PRODUCT_DEFINITION('GATE_HOUSING_PLATE',
'GATE_HOUSING_PLATE',#50748,#50671) ;
#50697 = PRODUCT_DEFINITION('METERING_GATE_ORIFICE_PLATE',
'METERING_GATE_ORIFICE_PLATE',#50749,#50671) ;
#50698 = PRODUCT_DEFINITION('FLOW_RATE_SCALE_STRIP',
'FLOW_RATE_SCALE_STRIP',#50750,#50671) ;
#50699 = PRODUCT_DEFINITION('OUTLET_FUNNEL','OUTLET_FUNNEL',#50751,
#50671) ;
#50700 = PRODUCT_DEFINITION('SPOUT_FEED_FUNNEL','SPOUT_FEED_FUNNEL',
#50752,#50671) ;
#50701 = PRODUCT_DEFINITION('FLOW_CONTROL_QUADRANT',
'FLOW_CONTROL_QUADRANT',#50753,#50671) ;
#50702 = PRODUCT_DEFINITION('CABLE_ACTUATED_FLOW_CONTROL_LEVER',
'CABLE_ACTUATED_FLOW_CONTROL_LEVER',#50754,#50671) ;
#50703 = PRODUCT_DEFINITION('LEVER_KNOB','LEVER_KNOB',#50755,
#50671) ;
#50704 = PRODUCT_DEFINITION('LEVER_PIVOT_PIN','LEVER_PIVOT_PIN',#50756,
#50671) ;
#50705 = PRODUCT_DEFINITION('CONTROL_CABLE_SHEATH',
'CONTROL_CABLE_SHEATH',#50757,#50671) ;
#50706 = PRODUCT_DEFINITION('CONTROL_CABLE_INNER_WIRE',
'CONTROL_CABLE_INNER_WIRE',#50758,#50671) ;
#50707 = PRODUCT_DEFINITION('CABLE_END_NIPPLE','CABLE_END_NIPPLE',
#50759,#50671) ;
#50708 = PRODUCT_DEFINITION('LEVER_END_NIPPLE','LEVER_END_NIPPLE',
#50760,#50671) ;
#50709 = PRODUCT_DEFINITION('RETURN_TENSION_SPRING_ASSEMBLY',
'RETURN_TENSION_SPRING_ASSEMBLY',#50761,#50671) ;
#50710 = PRODUCT_DEFINITION('SPOUT_UNIT','SPOUT_UNIT',#50762,
#50671) ;
#50711 = PRODUCT_DEFINITION('OSCILLATING_SPOUT_TUBE',
'OSCILLATING_SPOUT_TUBE',#50763,#50671) ;
#50712 = PRODUCT_DEFINITION('PENDULUM_TRUNNION_YOKE',
'PENDULUM_TRUNNION_YOKE',#50764,#50671) ;
#50713 = PRODUCT_DEFINITION('TRUNNION_BUSHING','TRUNNION_BUSHING',
#50765,#50671) ;
#50714 = PRODUCT_DEFINITION('SPOUT_DEFLECTOR_PLATE',
'SPOUT_DEFLECTOR_PLATE',#50766,#50671) ;
#50715 = PRODUCT_DEFINITION('SPOUT_CLAMP_BAND','SPOUT_CLAMP_BAND',
#50767,#50671) ;
#50716 = PRODUCT_DEFINITION('FASTENERS','FASTENERS',#50768,
#50671) ;
#50717 = PRODUCT_DEFINITION('GEARBOX_MOUNT_BOLT_M12x65',
'GEARBOX_MOUNT_BOLT_M12x65',#50769,#50671) ;
#50718 = PRODUCT_DEFINITION('GEARBOX_MOUNT_NUT_M12',
'GEARBOX_MOUNT_NUT_M12',#50770,#50671) ;
#50719 = PRODUCT_DEFINITION('GATE_HOUSING_BOLT_M8x30',
'GATE_HOUSING_BOLT_M8x30',#50771,#50671) ;
#50720 = PRODUCT_DEFINITION('LEVER_PIVOT_NUT_M10',
'LEVER_PIVOT_NUT_M10',#50772,#50671) ;
#50721 = PRODUCT_DEFINITION('SPRING_HOOK_PIN','SPRING_HOOK_PIN',#50773,
#50671) ;
#50722 = PRODUCT_DEFINITION('SPRING_ANCHOR_PIN','SPRING_ANCHOR_PIN',
#50774,#50671) ;
#50723 = PRODUCT_DEFINITION('LINCH_PIN','LINCH_PIN',#50775,
#50671) ;
#50724 = PRODUCT_DEFINITION_FORMATION('',$,#50831) ;
#50725 = PRODUCT_DEFINITION_FORMATION('',$,#50832) ;
#50726 = PRODUCT_DEFINITION_FORMATION('',$,#50833) ;
#50727 = PRODUCT_DEFINITION_FORMATION('',$,#50834) ;
#50728 = PRODUCT_DEFINITION_FORMATION('',$,#50835) ;
#50729 = PRODUCT_DEFINITION_FORMATION('',$,#50836) ;
#50730 = PRODUCT_DEFINITION_FORMATION('',$,#50837) ;
#50731 = PRODUCT_DEFINITION_FORMATION('',$,#50838) ;
#50732 = PRODUCT_DEFINITION_FORMATION('',$,#50839) ;
#50733 = PRODUCT_DEFINITION_FORMATION('',$,#50840) ;
#50734 = PRODUCT_DEFINITION_FORMATION('',$,#50841) ;
#50735 = PRODUCT_DEFINITION_FORMATION('',$,#50842) ;
#50736 = PRODUCT_DEFINITION_FORMATION('',$,#50843) ;
#50737 = PRODUCT_DEFINITION_FORMATION('',$,#50844) ;
#50738 = PRODUCT_DEFINITION_FORMATION('',$,#50845) ;
#50739 = PRODUCT_DEFINITION_FORMATION('',$,#50846) ;
#50740 = PRODUCT_DEFINITION_FORMATION('',$,#50847) ;
#50741 = PRODUCT_DEFINITION_FORMATION('',$,#50848) ;
#50742 = PRODUCT_DEFINITION_FORMATION('',$,#50849) ;
#50743 = PRODUCT_DEFINITION_FORMATION('',$,#50850) ;
#50744 = PRODUCT_DEFINITION_FORMATION('',$,#50851) ;
#50745 = PRODUCT_DEFINITION_FORMATION('',$,#50852) ;
#50746 = PRODUCT_DEFINITION_FORMATION('',$,#50853) ;
#50747 = PRODUCT_DEFINITION_FORMATION('',$,#50854) ;
#50748 = PRODUCT_DEFINITION_FORMATION('',$,#50855) ;
#50749 = PRODUCT_DEFINITION_FORMATION('',$,#50856) ;
#50750 = PRODUCT_DEFINITION_FORMATION('',$,#50857) ;
#50751 = PRODUCT_DEFINITION_FORMATION('',$,#50858) ;
#50752 = PRODUCT_DEFINITION_FORMATION('',$,#50859) ;
#50753 = PRODUCT_DEFINITION_FORMATION('',$,#50860) ;
#50754 = PRODUCT_DEFINITION_FORMATION('',$,#50861) ;
#50755 = PRODUCT_DEFINITION_FORMATION('',$,#50862) ;
#50756 = PRODUCT_DEFINITION_FORMATION('',$,#50863) ;
#50757 = PRODUCT_DEFINITION_FORMATION('',$,#50864) ;
#50758 = PRODUCT_DEFINITION_FORMATION('',$,#50865) ;
#50759 = PRODUCT_DEFINITION_FORMATION('',$,#50866) ;
#50760 = PRODUCT_DEFINITION_FORMATION('',$,#50867) ;
#50761 = PRODUCT_DEFINITION_FORMATION('',$,#50868) ;
#50762 = PRODUCT_DEFINITION_FORMATION('',$,#50869) ;
#50763 = PRODUCT_DEFINITION_FORMATION('',$,#50870) ;
#50764 = PRODUCT_DEFINITION_FORMATION('',$,#50871) ;
#50765 = PRODUCT_DEFINITION_FORMATION('',$,#50872) ;
#50766 = PRODUCT_DEFINITION_FORMATION('',$,#50873) ;
#50767 = PRODUCT_DEFINITION_FORMATION('',$,#50874) ;
#50768 = PRODUCT_DEFINITION_FORMATION('',$,#50875) ;
#50769 = PRODUCT_DEFINITION_FORMATION('',$,#50876) ;
#50770 = PRODUCT_DEFINITION_FORMATION('',$,#50877) ;
#50771 = PRODUCT_DEFINITION_FORMATION('',$,#50878) ;
#50772 = PRODUCT_DEFINITION_FORMATION('',$,#50879) ;
#50773 = PRODUCT_DEFINITION_FORMATION('',$,#50880) ;
#50774 = PRODUCT_DEFINITION_FORMATION('',$,#50881) ;
#50775 = PRODUCT_DEFINITION_FORMATION('',$,#50882) ;
#50776 = PRODUCT_RELATED_PRODUCT_CATEGORY(
'MAS-603','MAS-603',
(#50831)) ;
#50777 = PRODUCT_RELATED_PRODUCT_CATEGORY('HOPPER_UNIT','HOPPER_UNIT',(#50832)) ;
#50778 = PRODUCT_RELATED_PRODUCT_CATEGORY('CONICAL_POLYETHYLENE_HOPPER',
'CONICAL_POLYETHYLENE_HOPPER',(#50833)) ;
#50779 = PRODUCT_RELATED_PRODUCT_CATEGORY('HOPPER_LID','HOPPER_LID',(#50834)) ;
#50780 = PRODUCT_RELATED_PRODUCT_CATEGORY('LID_HINGE_STRAP',
'LID_HINGE_STRAP',(#50835)) ;
#50781 = PRODUCT_RELATED_PRODUCT_CATEGORY('HOPPER_SIEVE_GRID',
'HOPPER_SIEVE_GRID',(#50836)) ;
#50782 = PRODUCT_RELATED_PRODUCT_CATEGORY('HOPPER_SUPPORT_RING',
'HOPPER_SUPPORT_RING',(#50837)) ;
#50783 = PRODUCT_RELATED_PRODUCT_CATEGORY('HITCH_FRAME_UNIT',
'HITCH_FRAME_UNIT',(#50838)) ;
#50784 = PRODUCT_RELATED_PRODUCT_CATEGORY('TUBULAR_3POINT_HITCH_FRAME',
'TUBULAR_3POINT_HITCH_FRAME',(#50839)) ;
#50785 = PRODUCT_RELATED_PRODUCT_CATEGORY('STAND_FOOT_PLATE',
'STAND_FOOT_PLATE',(#50840)) ;
#50786 = PRODUCT_RELATED_PRODUCT_CATEGORY('LOWER_LINK_PIN_CAT2',
'LOWER_LINK_PIN_CAT2',(#50841)) ;
#50787 = PRODUCT_RELATED_PRODUCT_CATEGORY('TOP_LINK_PIN_CAT2',
'TOP_LINK_PIN_CAT2',(#50842)) ;
#50788 = PRODUCT_RELATED_PRODUCT_CATEGORY('GEARBOX_DRIVE_UNIT',
'GEARBOX_DRIVE_UNIT',(#50843)) ;
#50789 = PRODUCT_RELATED_PRODUCT_CATEGORY('GEARBOX_OSCILLATION_HOUSING',
'GEARBOX_OSCILLATION_HOUSING',(#50844)) ;
#50790 = PRODUCT_RELATED_PRODUCT_CATEGORY('GEARBOX_OIL_PLUG',
'GEARBOX_OIL_PLUG',(#50845)) ;
#50791 = PRODUCT_RELATED_PRODUCT_CATEGORY('PTO_INPUT_SHAFT_SPLINE',
'PTO_INPUT_SHAFT_SPLINE',(#50846)) ;
#50792 = PRODUCT_RELATED_PRODUCT_CATEGORY('PTO_SHAFT_SEAL',
'PTO_SHAFT_SEAL',(#50847)) ;
#50793 = PRODUCT_RELATED_PRODUCT_CATEGORY('PTO_SHIELD_GUARD',
'PTO_SHIELD_GUARD',(#50848)) ;
#50794 = PRODUCT_RELATED_PRODUCT_CATEGORY('OSCILLATION_OUTPUT_SHAFT',
'OSCILLATION_OUTPUT_SHAFT',(#50849)) ;
#50795 = PRODUCT_RELATED_PRODUCT_CATEGORY('OSCILLATION_CRANK_DISC',
'OSCILLATION_CRANK_DISC',(#50850)) ;
#50796 = PRODUCT_RELATED_PRODUCT_CATEGORY('CONNECTING_ROD',
'CONNECTING_ROD',(#50851)) ;
#50797 = PRODUCT_RELATED_PRODUCT_CATEGORY('AGITATOR_SHAFT_ASSEMBLY',
'AGITATOR_SHAFT_ASSEMBLY',(#50852)) ;
#50798 = PRODUCT_RELATED_PRODUCT_CATEGORY('AGITATOR_SHAFT_SEAL',
'AGITATOR_SHAFT_SEAL',(#50853)) ;
#50799 = PRODUCT_RELATED_PRODUCT_CATEGORY('METERING_GATE_UNIT',
'METERING_GATE_UNIT',(#50854)) ;
#50800 = PRODUCT_RELATED_PRODUCT_CATEGORY('GATE_HOUSING_PLATE',
'GATE_HOUSING_PLATE',(#50855)) ;
#50801 = PRODUCT_RELATED_PRODUCT_CATEGORY('METERING_GATE_ORIFICE_PLATE',
'METERING_GATE_ORIFICE_PLATE',(#50856)) ;
#50802 = PRODUCT_RELATED_PRODUCT_CATEGORY('FLOW_RATE_SCALE_STRIP',
'FLOW_RATE_SCALE_STRIP',(#50857)) ;
#50803 = PRODUCT_RELATED_PRODUCT_CATEGORY('OUTLET_FUNNEL','OUTLET_FUNNEL',
(#50858)) ;
#50804 = PRODUCT_RELATED_PRODUCT_CATEGORY('SPOUT_FEED_FUNNEL',
'SPOUT_FEED_FUNNEL',(#50859)) ;
#50805 = PRODUCT_RELATED_PRODUCT_CATEGORY('FLOW_CONTROL_QUADRANT',
'FLOW_CONTROL_QUADRANT',(#50860)) ;
#50806 = PRODUCT_RELATED_PRODUCT_CATEGORY(
'CABLE_ACTUATED_FLOW_CONTROL_LEVER','CABLE_ACTUATED_FLOW_CONTROL_LEVER',
(#50861)) ;
#50807 = PRODUCT_RELATED_PRODUCT_CATEGORY('LEVER_KNOB','LEVER_KNOB',(#50862)) ;
#50808 = PRODUCT_RELATED_PRODUCT_CATEGORY('LEVER_PIVOT_PIN',
'LEVER_PIVOT_PIN',(#50863)) ;
#50809 = PRODUCT_RELATED_PRODUCT_CATEGORY('CONTROL_CABLE_SHEATH',
'CONTROL_CABLE_SHEATH',(#50864)) ;
#50810 = PRODUCT_RELATED_PRODUCT_CATEGORY('CONTROL_CABLE_INNER_WIRE',
'CONTROL_CABLE_INNER_WIRE',(#50865)) ;
#50811 = PRODUCT_RELATED_PRODUCT_CATEGORY('CABLE_END_NIPPLE',
'CABLE_END_NIPPLE',(#50866)) ;
#50812 = PRODUCT_RELATED_PRODUCT_CATEGORY('LEVER_END_NIPPLE',
'LEVER_END_NIPPLE',(#50867)) ;
#50813 = PRODUCT_RELATED_PRODUCT_CATEGORY(
'RETURN_TENSION_SPRING_ASSEMBLY','RETURN_TENSION_SPRING_ASSEMBLY',(#50868)) ;
#50814 = PRODUCT_RELATED_PRODUCT_CATEGORY('SPOUT_UNIT','SPOUT_UNIT',(#50869)) ;
#50815 = PRODUCT_RELATED_PRODUCT_CATEGORY('OSCILLATING_SPOUT_TUBE',
'OSCILLATING_SPOUT_TUBE',(#50870)) ;
#50816 = PRODUCT_RELATED_PRODUCT_CATEGORY('PENDULUM_TRUNNION_YOKE',
'PENDULUM_TRUNNION_YOKE',(#50871)) ;
#50817 = PRODUCT_RELATED_PRODUCT_CATEGORY('TRUNNION_BUSHING',
'TRUNNION_BUSHING',(#50872)) ;
#50818 = PRODUCT_RELATED_PRODUCT_CATEGORY('SPOUT_DEFLECTOR_PLATE',
'SPOUT_DEFLECTOR_PLATE',(#50873)) ;
#50819 = PRODUCT_RELATED_PRODUCT_CATEGORY('SPOUT_CLAMP_BAND',
'SPOUT_CLAMP_BAND',(#50874)) ;
#50820 = PRODUCT_RELATED_PRODUCT_CATEGORY('FASTENERS','FASTENERS',(#50875)) ;
#50821 = PRODUCT_RELATED_PRODUCT_CATEGORY('GEARBOX_MOUNT_BOLT_M12x65',
'GEARBOX_MOUNT_BOLT_M12x65',(#50876)) ;
#50822 = PRODUCT_RELATED_PRODUCT_CATEGORY('GEARBOX_MOUNT_NUT_M12',
'GEARBOX_MOUNT_NUT_M12',(#50877)) ;
#50823 = PRODUCT_RELATED_PRODUCT_CATEGORY('GATE_HOUSING_BOLT_M8x30',
'GATE_HOUSING_BOLT_M8x30',(#50878)) ;
#50824 = PRODUCT_RELATED_PRODUCT_CATEGORY('LEVER_PIVOT_NUT_M10',
'LEVER_PIVOT_NUT_M10',(#50879)) ;
#50825 = PRODUCT_RELATED_PRODUCT_CATEGORY('SPRING_HOOK_PIN',
'SPRING_HOOK_PIN',(#50880)) ;
#50826 = PRODUCT_RELATED_PRODUCT_CATEGORY('SPRING_ANCHOR_PIN',
'SPRING_ANCHOR_PIN',(#50881)) ;
#50827 = PRODUCT_RELATED_PRODUCT_CATEGORY('LINCH_PIN','LINCH_PIN',(#50882)) ;
#50828 = APPLICATION_PROTOCOL_DEFINITION('international standard',
'automotive_design',2009,#50829) ;
#50829 = APPLICATION_CONTEXT(
'Core Data for Automotive Mechanical Design Process') ;
#50830 = PRODUCT_CONTEXT('part definition',#50829,'mechanical') ;
#50831 = PRODUCT('MAS-603',
'MAS-603',$,(#50830)) ;
#50832 = PRODUCT('HOPPER_UNIT','HOPPER_UNIT',$,(#50830)) ;
#50833 = PRODUCT('CONICAL_POLYETHYLENE_HOPPER','CONICAL_POLYETHYLENE_HOPPER',
$,(#50830)) ;
#50834 = PRODUCT('HOPPER_LID','HOPPER_LID',$,(#50830)) ;
#50835 = PRODUCT('LID_HINGE_STRAP','LID_HINGE_STRAP',$,(#50830)) ;
#50836 = PRODUCT('HOPPER_SIEVE_GRID','HOPPER_SIEVE_GRID',$,(#50830)) ;
#50837 = PRODUCT('HOPPER_SUPPORT_RING','HOPPER_SUPPORT_RING',$,(#50830)) ;
#50838 = PRODUCT('HITCH_FRAME_UNIT','HITCH_FRAME_UNIT',$,(#50830)) ;
#50839 = PRODUCT('TUBULAR_3POINT_HITCH_FRAME','TUBULAR_3POINT_HITCH_FRAME',$,
(#50830)) ;
#50840 = PRODUCT('STAND_FOOT_PLATE','STAND_FOOT_PLATE',$,(#50830)) ;
#50841 = PRODUCT('LOWER_LINK_PIN_CAT2','LOWER_LINK_PIN_CAT2',$,(#50830)) ;
#50842 = PRODUCT('TOP_LINK_PIN_CAT2','TOP_LINK_PIN_CAT2',$,(#50830)) ;
#50843 = PRODUCT('GEARBOX_DRIVE_UNIT','GEARBOX_DRIVE_UNIT',$,(#50830)) ;
#50844 = PRODUCT('GEARBOX_OSCILLATION_HOUSING','GEARBOX_OSCILLATION_HOUSING',
$,(#50830)) ;
#50845 = PRODUCT('GEARBOX_OIL_PLUG','GEARBOX_OIL_PLUG',$,(#50830)) ;
#50846 = PRODUCT('PTO_INPUT_SHAFT_SPLINE','PTO_INPUT_SHAFT_SPLINE',$,(#50830)) ;
#50847 = PRODUCT('PTO_SHAFT_SEAL','PTO_SHAFT_SEAL',$,(#50830)) ;
#50848 = PRODUCT('PTO_SHIELD_GUARD','PTO_SHIELD_GUARD',$,(#50830)) ;
#50849 = PRODUCT('OSCILLATION_OUTPUT_SHAFT','OSCILLATION_OUTPUT_SHAFT',$,(#50830)) ;
#50850 = PRODUCT('OSCILLATION_CRANK_DISC','OSCILLATION_CRANK_DISC',$,(#50830)) ;
#50851 = PRODUCT('CONNECTING_ROD','CONNECTING_ROD',$,(#50830)) ;
#50852 = PRODUCT('AGITATOR_SHAFT_ASSEMBLY','AGITATOR_SHAFT_ASSEMBLY',$,(#50830)) ;
#50853 = PRODUCT('AGITATOR_SHAFT_SEAL','AGITATOR_SHAFT_SEAL',$,(#50830)) ;
#50854 = PRODUCT('METERING_GATE_UNIT','METERING_GATE_UNIT',$,(#50830)) ;
#50855 = PRODUCT('GATE_HOUSING_PLATE','GATE_HOUSING_PLATE',$,(#50830)) ;
#50856 = PRODUCT('METERING_GATE_ORIFICE_PLATE','METERING_GATE_ORIFICE_PLATE',
$,(#50830)) ;
#50857 = PRODUCT('FLOW_RATE_SCALE_STRIP','FLOW_RATE_SCALE_STRIP',$,(#50830)) ;
#50858 = PRODUCT('OUTLET_FUNNEL','OUTLET_FUNNEL',$,(#50830)) ;
#50859 = PRODUCT('SPOUT_FEED_FUNNEL','SPOUT_FEED_FUNNEL',$,(#50830)) ;
#50860 = PRODUCT('FLOW_CONTROL_QUADRANT','FLOW_CONTROL_QUADRANT',$,(#50830)) ;
#50861 = PRODUCT('CABLE_ACTUATED_FLOW_CONTROL_LEVER',
'CABLE_ACTUATED_FLOW_CONTROL_LEVER',$,(#50830)) ;
#50862 = PRODUCT('LEVER_KNOB','LEVER_KNOB',$,(#50830)) ;
#50863 = PRODUCT('LEVER_PIVOT_PIN','LEVER_PIVOT_PIN',$,(#50830)) ;
#50864 = PRODUCT('CONTROL_CABLE_SHEATH','CONTROL_CABLE_SHEATH',$,(#50830)) ;
#50865 = PRODUCT('CONTROL_CABLE_INNER_WIRE','CONTROL_CABLE_INNER_WIRE',$,(#50830)) ;
#50866 = PRODUCT('CABLE_END_NIPPLE','CABLE_END_NIPPLE',$,(#50830)) ;
#50867 = PRODUCT('LEVER_END_NIPPLE','LEVER_END_NIPPLE',$,(#50830)) ;
#50868 = PRODUCT('RETURN_TENSION_SPRING_ASSEMBLY',
'RETURN_TENSION_SPRING_ASSEMBLY',$,(#50830)) ;
#50869 = PRODUCT('SPOUT_UNIT','SPOUT_UNIT',$,(#50830)) ;
#50870 = PRODUCT('OSCILLATING_SPOUT_TUBE','OSCILLATING_SPOUT_TUBE',$,(#50830)) ;
#50871 = PRODUCT('PENDULUM_TRUNNION_YOKE','PENDULUM_TRUNNION_YOKE',$,(#50830)) ;
#50872 = PRODUCT('TRUNNION_BUSHING','TRUNNION_BUSHING',$,(#50830)) ;
#50873 = PRODUCT('SPOUT_DEFLECTOR_PLATE','SPOUT_DEFLECTOR_PLATE',$,(#50830)) ;
#50874 = PRODUCT('SPOUT_CLAMP_BAND','SPOUT_CLAMP_BAND',$,(#50830)) ;
#50875 = PRODUCT('FASTENERS','FASTENERS',$,(#50830)) ;
#50876 = PRODUCT('GEARBOX_MOUNT_BOLT_M12x65','GEARBOX_MOUNT_BOLT_M12x65',$,
(#50830)) ;
#50877 = PRODUCT('GEARBOX_MOUNT_NUT_M12','GEARBOX_MOUNT_NUT_M12',$,(#50830)) ;
#50878 = PRODUCT('GATE_HOUSING_BOLT_M8x30','GATE_HOUSING_BOLT_M8x30',$,(#50830)) ;
#50879 = PRODUCT('LEVER_PIVOT_NUT_M10','LEVER_PIVOT_NUT_M10',$,(#50830)) ;
#50880 = PRODUCT('SPRING_HOOK_PIN','SPRING_HOOK_PIN',$,(#50830)) ;
#50881 = PRODUCT('SPRING_ANCHOR_PIN','SPRING_ANCHOR_PIN',$,(#50830)) ;
#50882 = PRODUCT('LINCH_PIN','LINCH_PIN',$,(#50830)) ;
#50883 = PRESENTATION_STYLE_ASSIGNMENT((#50890)) ;
#50884 = PRESENTATION_STYLE_ASSIGNMENT((#50891)) ;
#50885 = PRESENTATION_STYLE_ASSIGNMENT((#50892)) ;
#50886 = PRESENTATION_STYLE_ASSIGNMENT((#50893)) ;
#50887 = PRESENTATION_STYLE_ASSIGNMENT((#50894)) ;
#50888 = PRESENTATION_STYLE_ASSIGNMENT((#50895)) ;
#50889 = PRESENTATION_STYLE_ASSIGNMENT((#50896)) ;
#50890 = SURFACE_STYLE_USAGE(.BOTH.,#50897) ;
#50891 = SURFACE_STYLE_USAGE(.BOTH.,#50898) ;
#50892 = SURFACE_STYLE_USAGE(.BOTH.,#50899) ;
#50893 = SURFACE_STYLE_USAGE(.BOTH.,#50900) ;
#50894 = SURFACE_STYLE_USAGE(.BOTH.,#50901) ;
#50895 = SURFACE_STYLE_USAGE(.BOTH.,#50902) ;
#50896 = SURFACE_STYLE_USAGE(.BOTH.,#50903) ;
#50897 = SURFACE_SIDE_STYLE('',(#50904)) ;
#50898 = SURFACE_SIDE_STYLE('',(#50905)) ;
#50899 = SURFACE_SIDE_STYLE('',(#50906)) ;
#50900 = SURFACE_SIDE_STYLE('',(#50907)) ;
#50901 = SURFACE_SIDE_STYLE('',(#50908)) ;
#50902 = SURFACE_SIDE_STYLE('',(#50909)) ;
#50903 = SURFACE_SIDE_STYLE('',(#50910)) ;
#50904 = SURFACE_STYLE_FILL_AREA(#50911) ;
#50905 = SURFACE_STYLE_FILL_AREA(#50912) ;
#50906 = SURFACE_STYLE_FILL_AREA(#50913) ;
#50907 = SURFACE_STYLE_FILL_AREA(#50914) ;
#50908 = SURFACE_STYLE_FILL_AREA(#50915) ;
#50909 = SURFACE_STYLE_FILL_AREA(#50916) ;
#50910 = SURFACE_STYLE_FILL_AREA(#50917) ;
#50911 = FILL_AREA_STYLE('Steel - Satin',(#50918)) ;
#50912 = FILL_AREA_STYLE('Surface - Matte',(#50919)) ;
#50913 = FILL_AREA_STYLE('Steel - Galvanized (Small)',(#50920)) ;
#50914 = FILL_AREA_STYLE('Aluminum - Satin',(#50921)) ;
#50915 = FILL_AREA_STYLE('Brass - Polished',(#50922)) ;
#50916 = FILL_AREA_STYLE('Rubber - Soft',(#50923)) ;
#50917 = FILL_AREA_STYLE('Stainless Steel - Satin',(#50924)) ;
#50918 = FILL_AREA_STYLE_COLOUR('Steel - Satin',#50925) ;
#50919 = FILL_AREA_STYLE_COLOUR('Surface - Matte',#50926) ;
#50920 = FILL_AREA_STYLE_COLOUR('Steel - Galvanized (Small)',#50927) ;
#50921 = FILL_AREA_STYLE_COLOUR('Aluminum - Satin',#50928) ;
#50922 = FILL_AREA_STYLE_COLOUR('Brass - Polished',#50929) ;
#50923 = FILL_AREA_STYLE_COLOUR('Rubber - Soft',#50930) ;
#50924 = FILL_AREA_STYLE_COLOUR('Stainless Steel - Satin',#50931) ;
#50925 = COLOUR_RGB('Steel - Satin', 0.31764706, 0.68627451, 0.89019608) ;
#50926 = COLOUR_RGB('Surface - Matte', 0.72549020, 0.75294118, 0.79215686) ;
#50927 = COLOUR_RGB('Steel - Galvanized (Small)', 0.09019608, 0.27058824, 0.51372549) ;
#50928 = COLOUR_RGB('Aluminum - Satin', 0.09019608, 0.27058824, 0.51372549) ;
#50929 = COLOUR_RGB('Brass - Polished', 0.66274510, 0.83137255, 0.94901961) ;
#50930 = COLOUR_RGB('Rubber - Soft', 0.40784314, 0.44705882, 0.49803922) ;
#50931 = COLOUR_RGB('Stainless Steel - Satin', 0.72549020, 0.75294118, 0.79215686) ;
ENDSEC;
END-ISO-10303-21;
